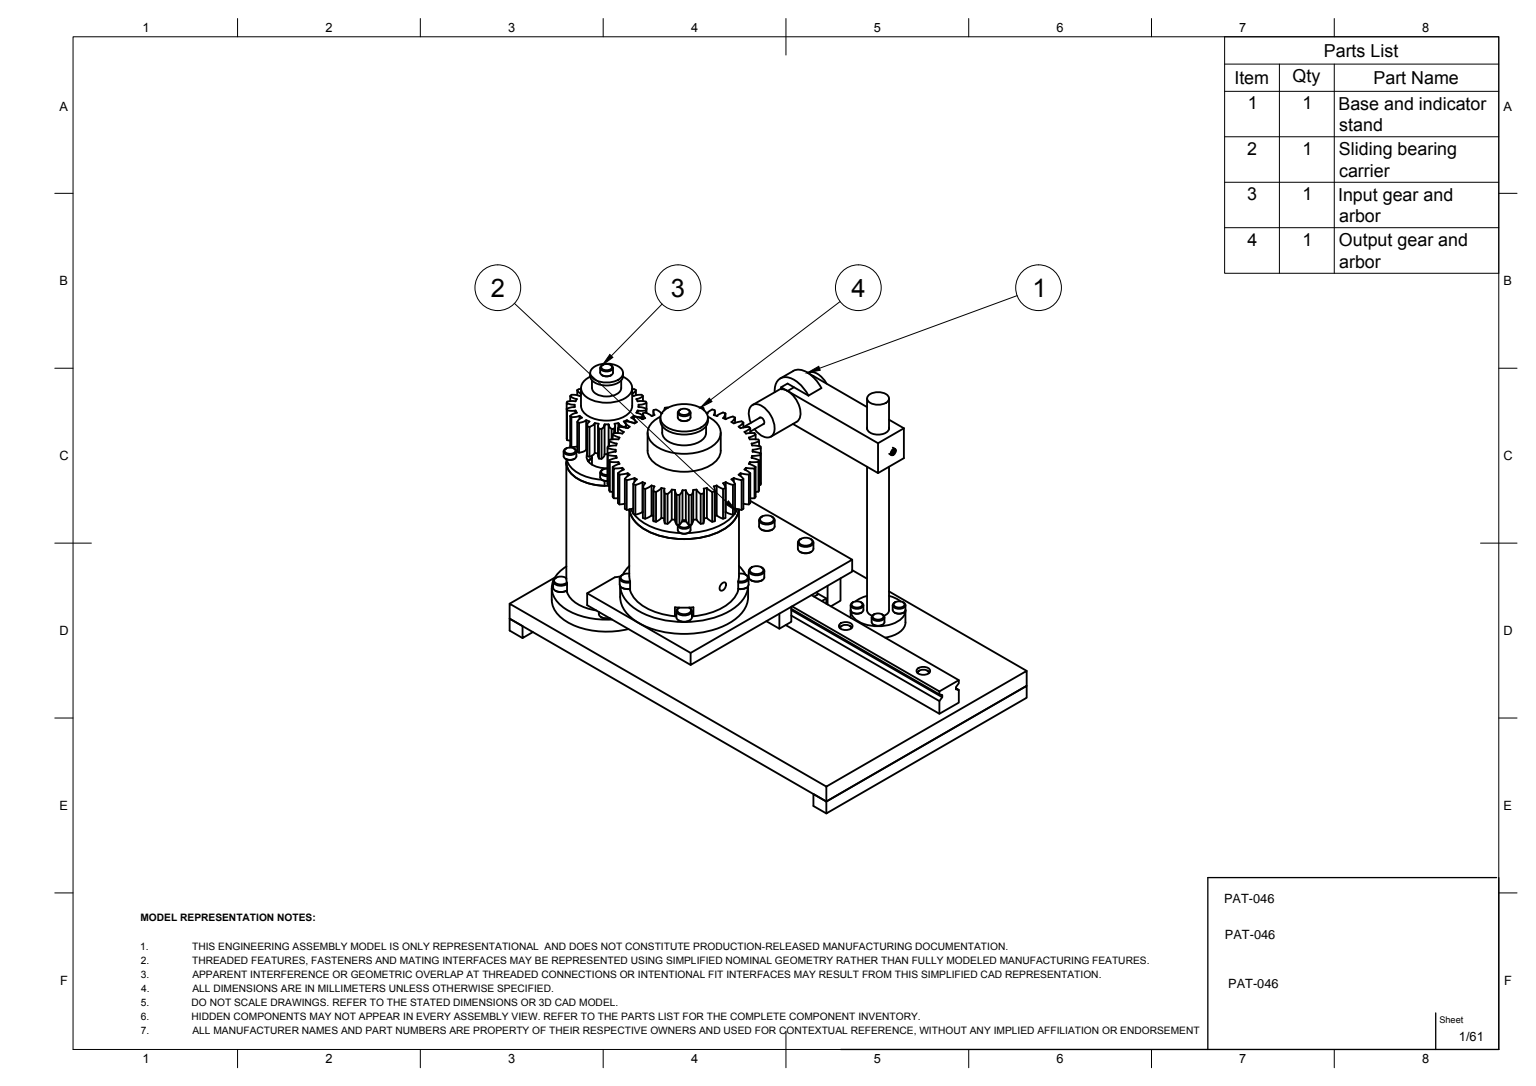
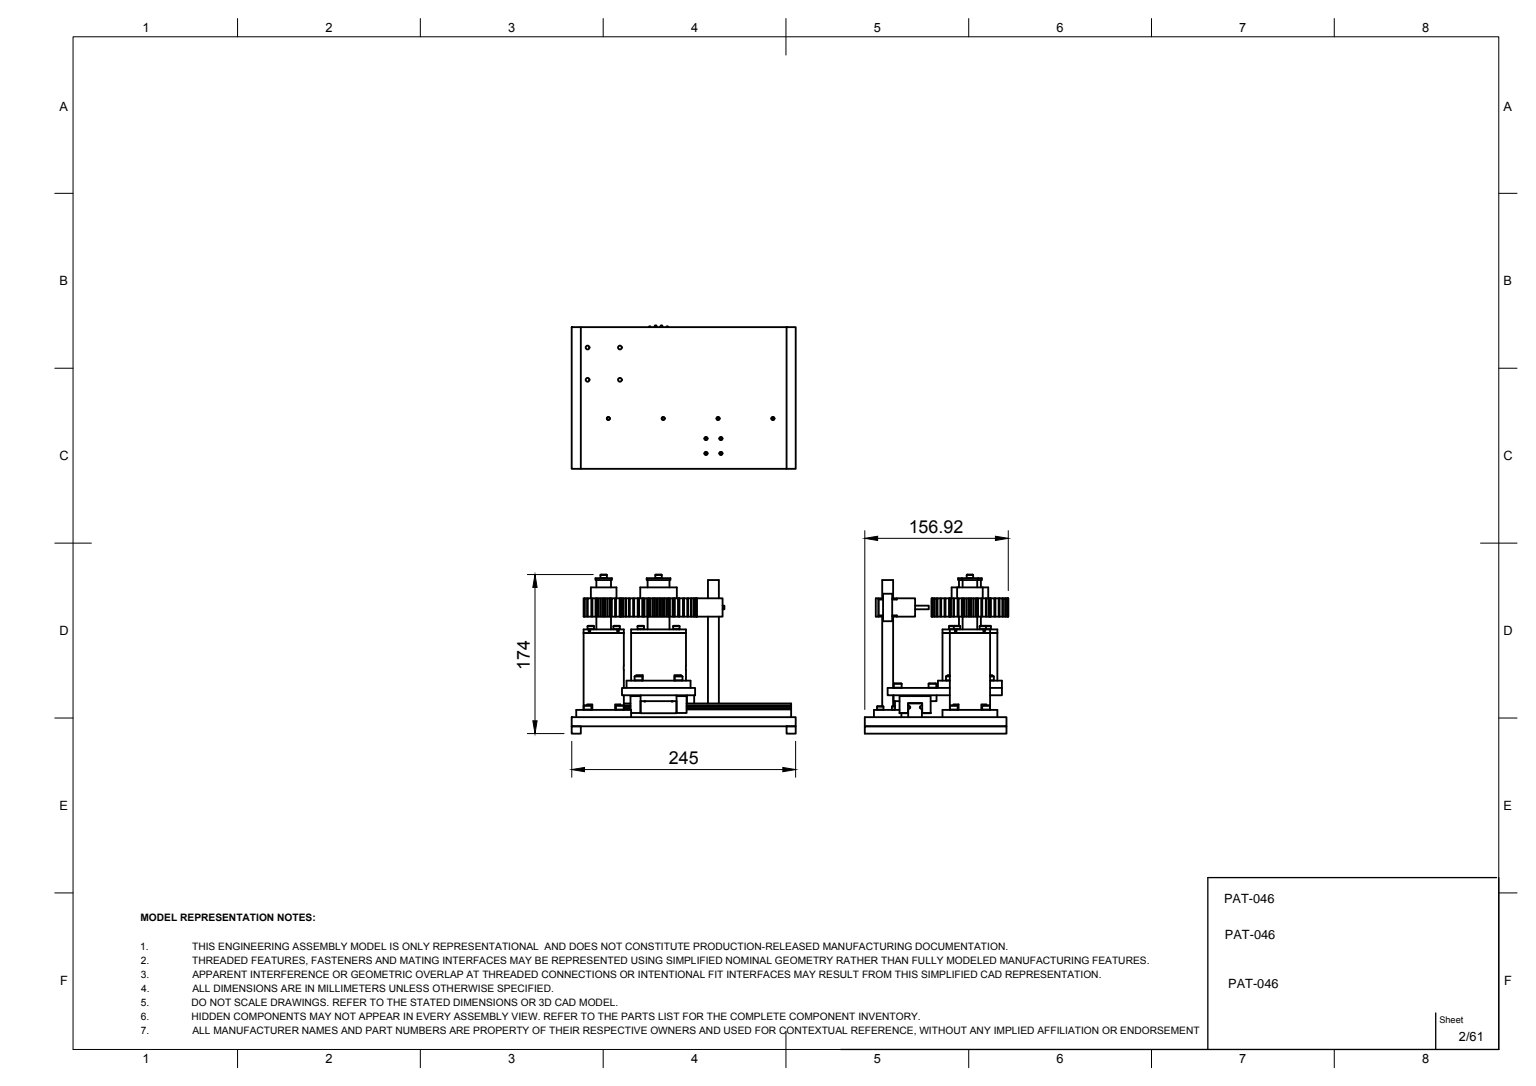
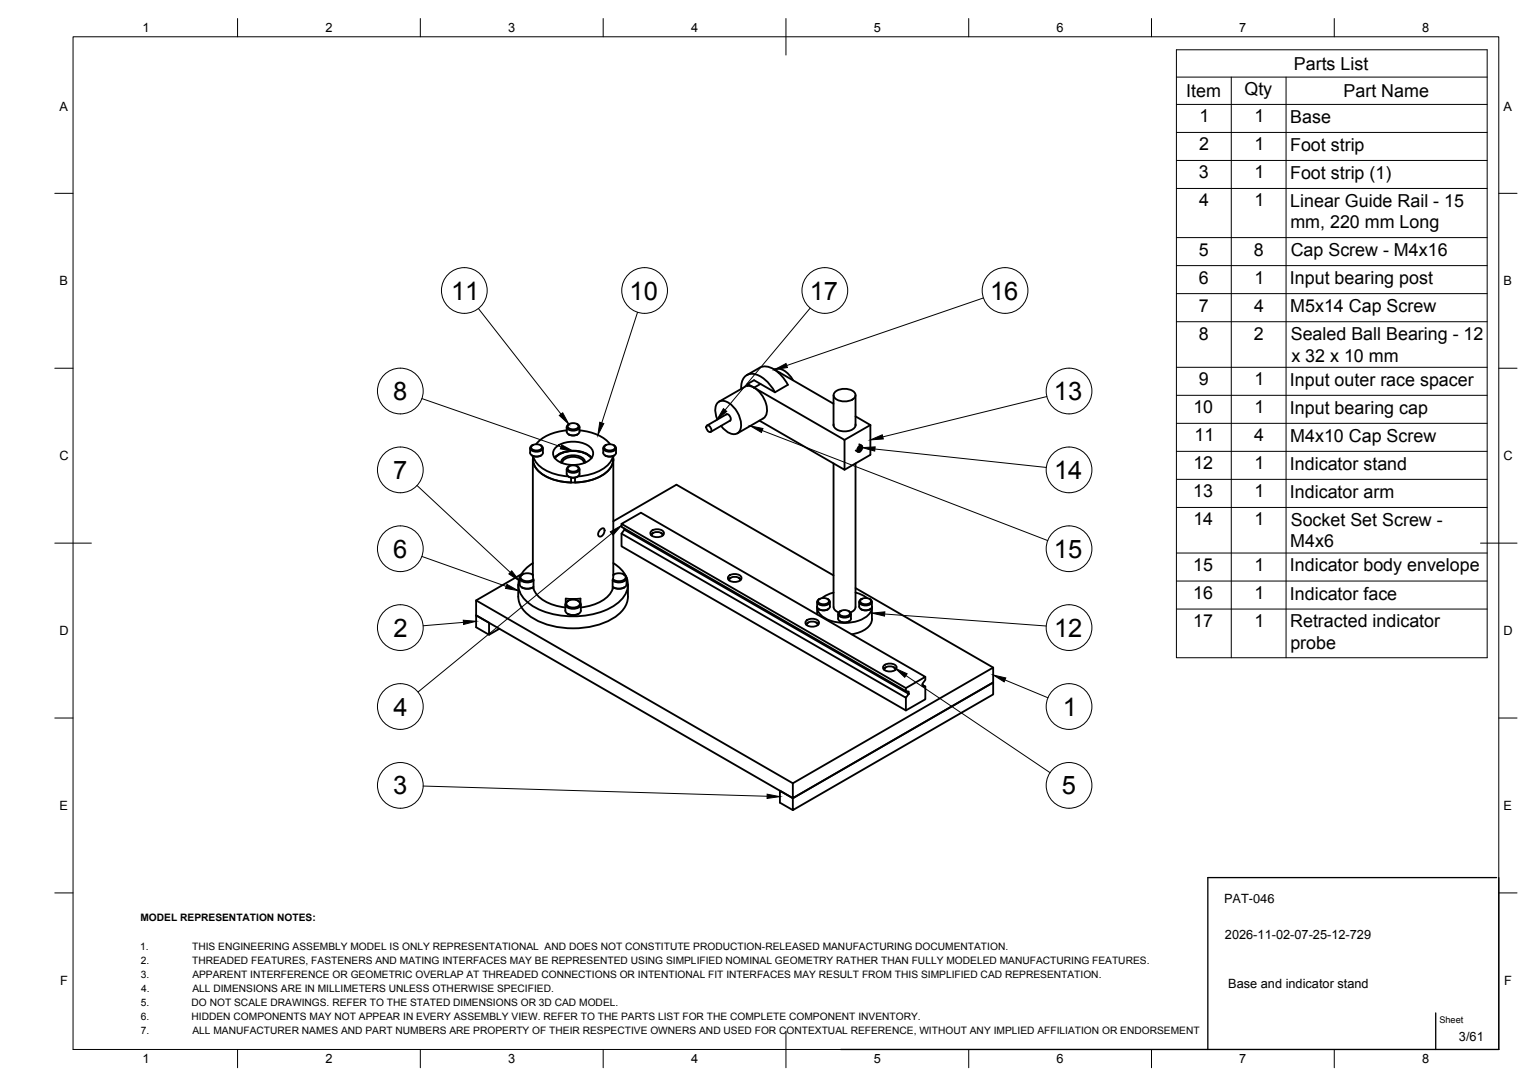
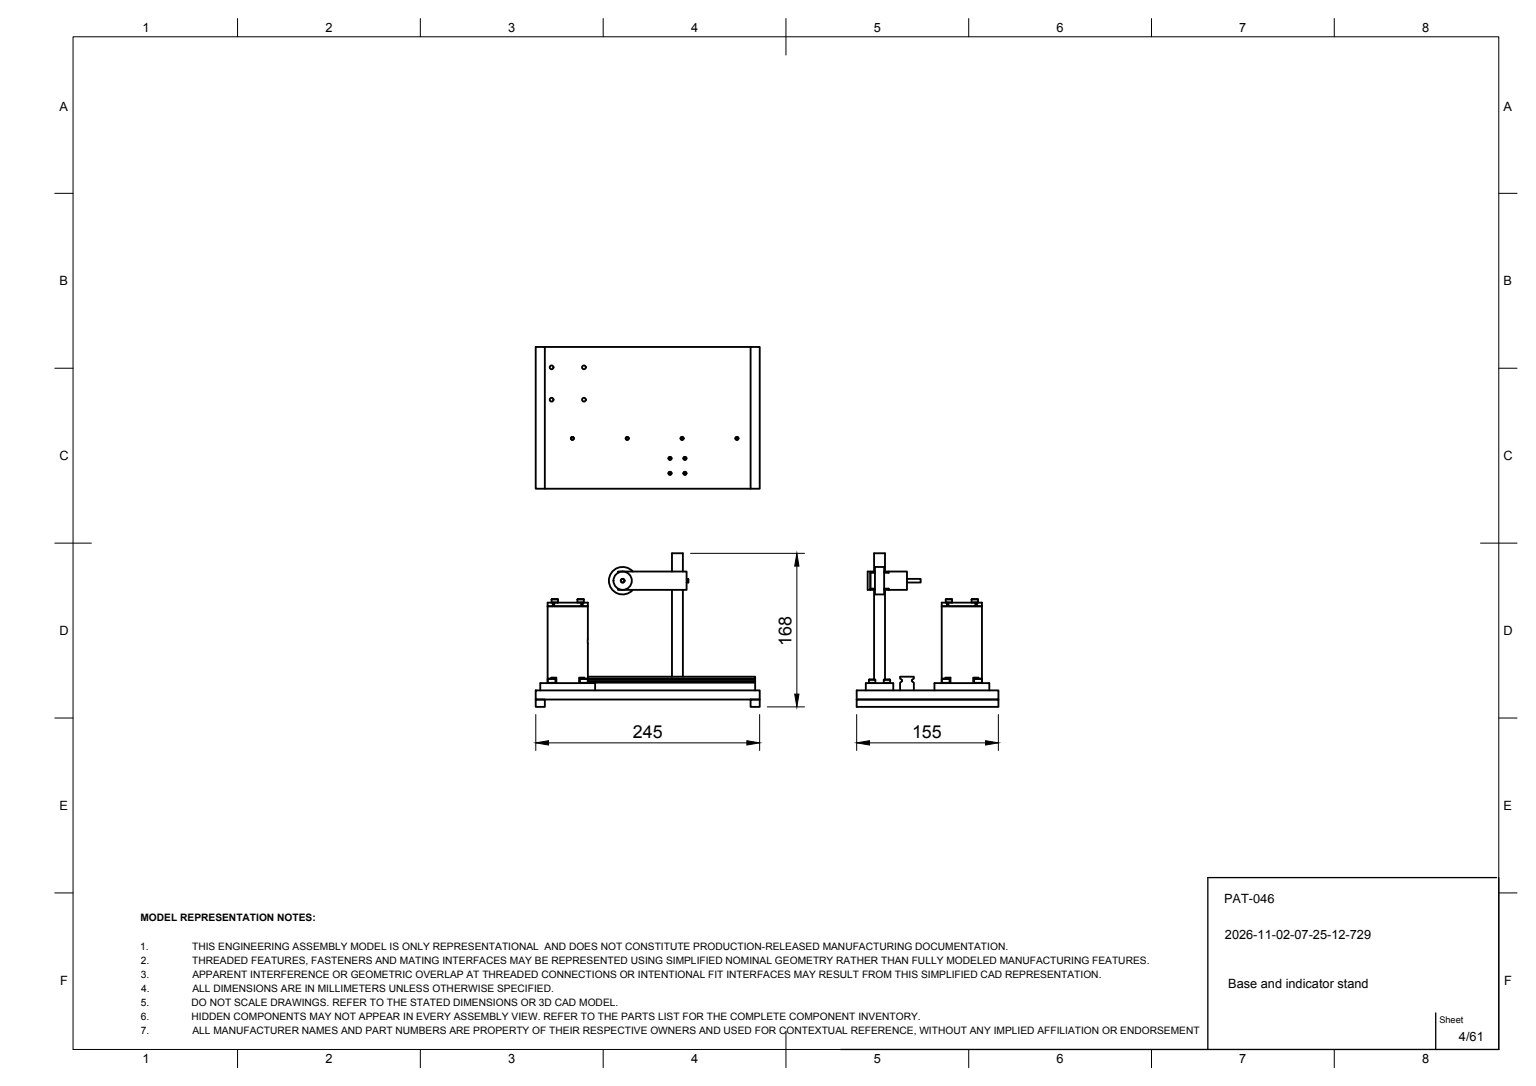
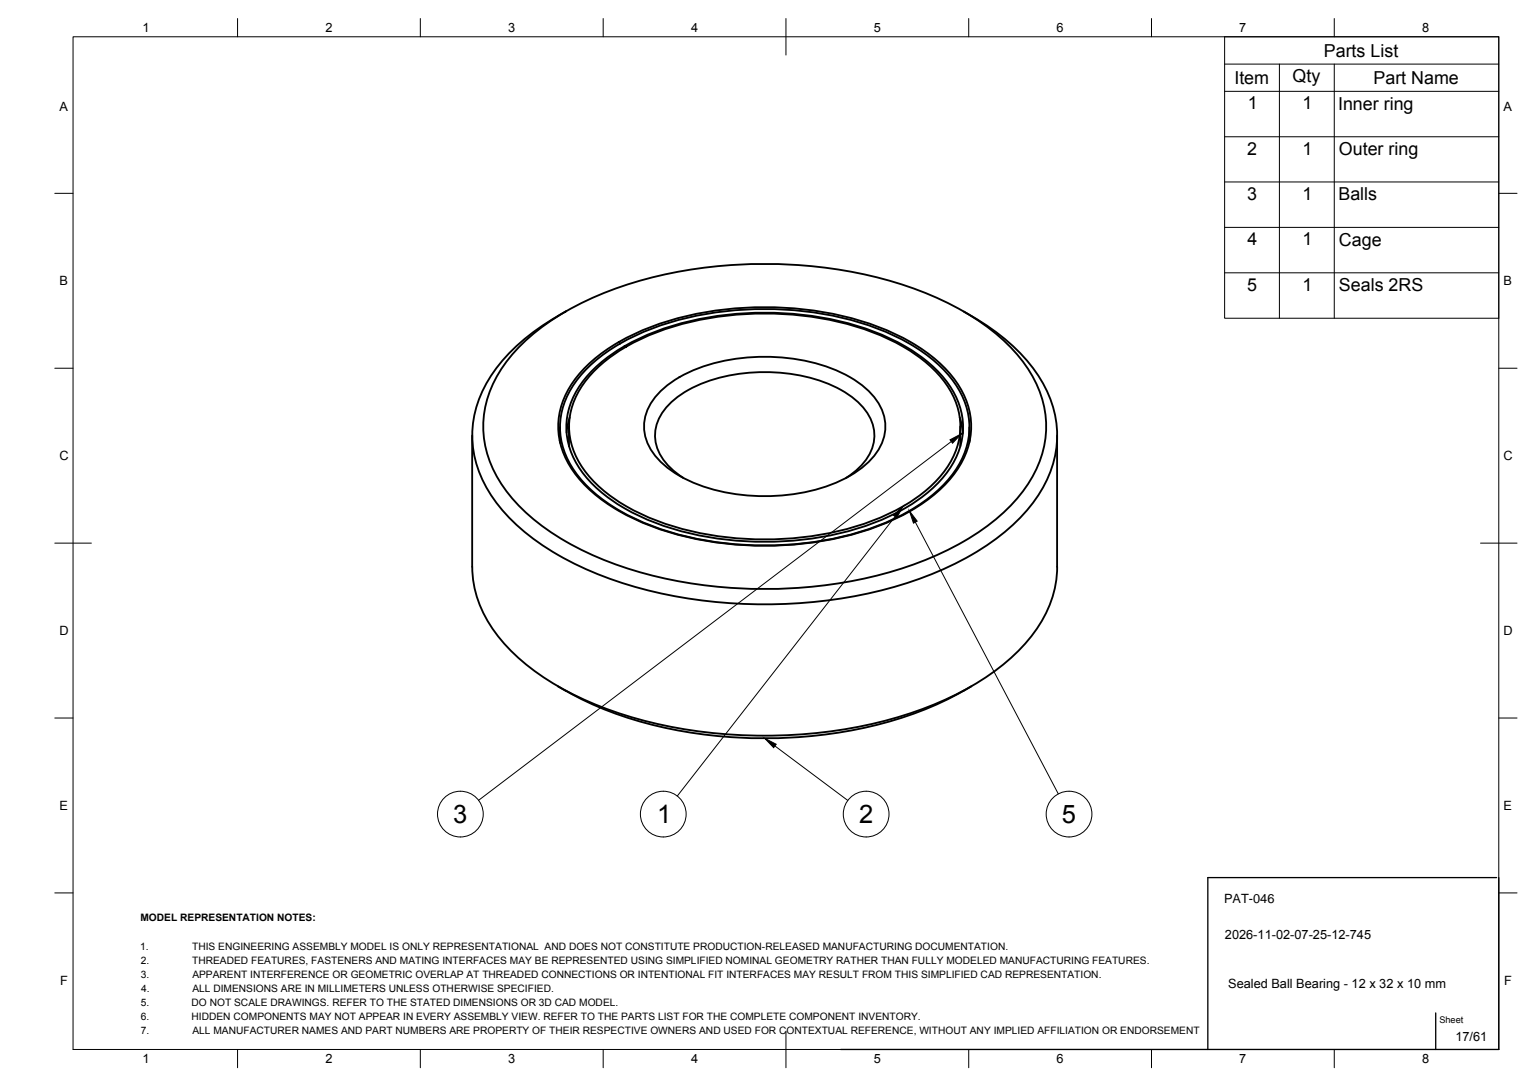
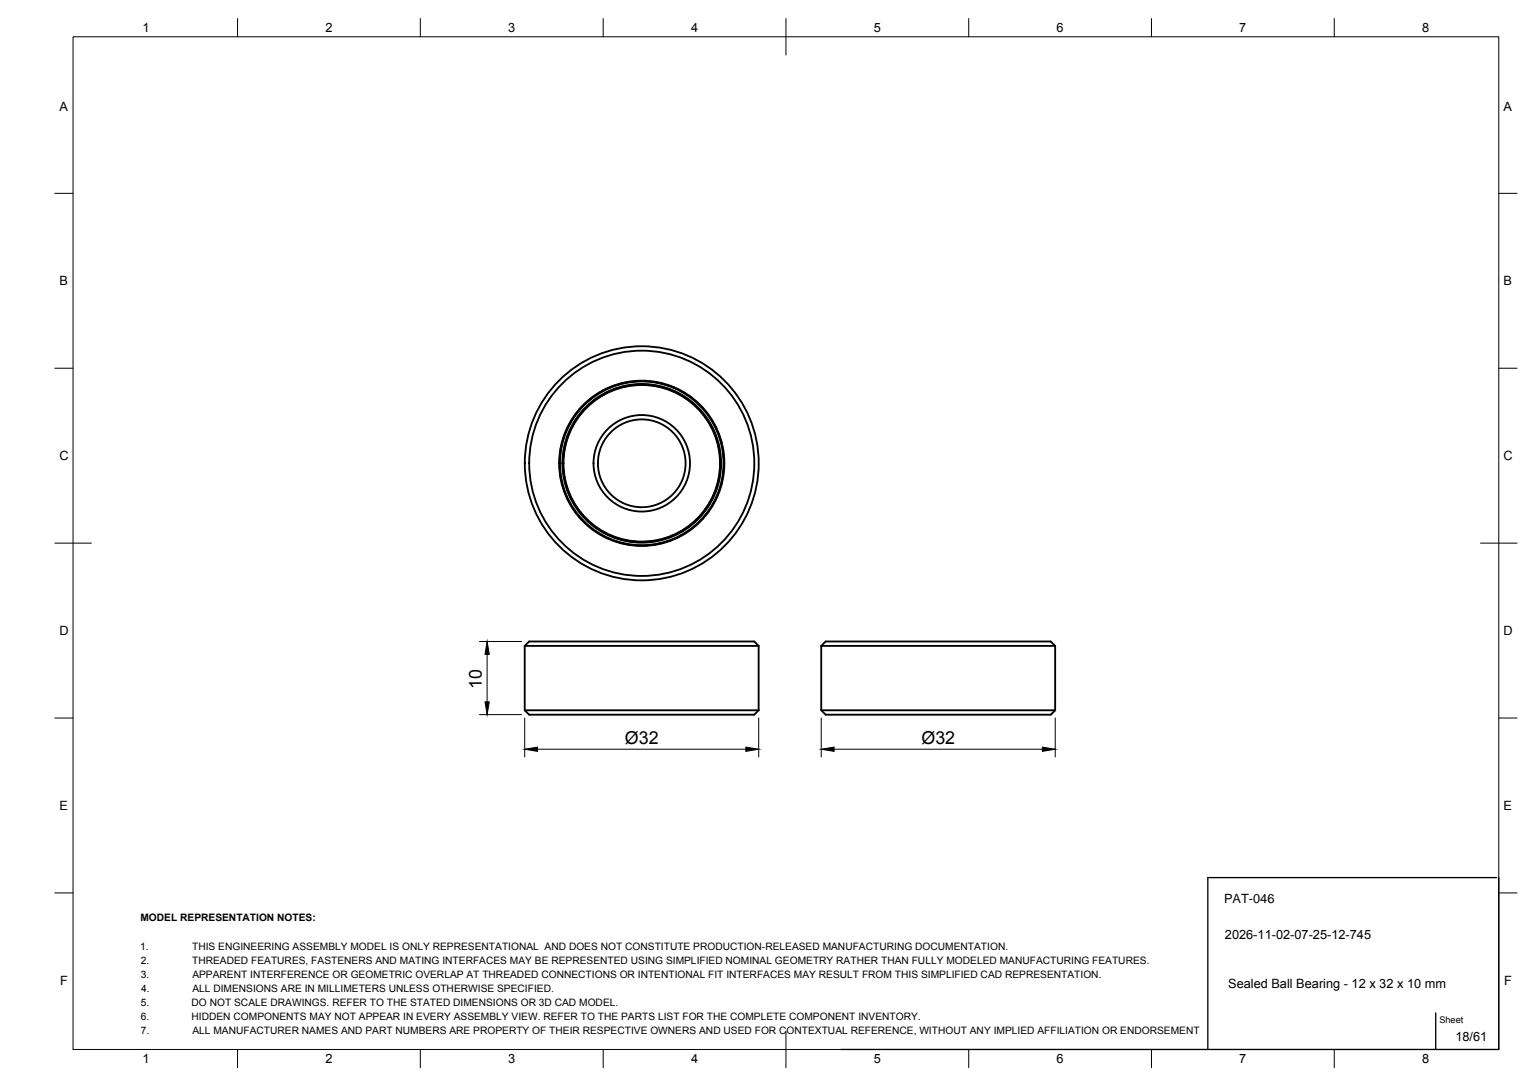
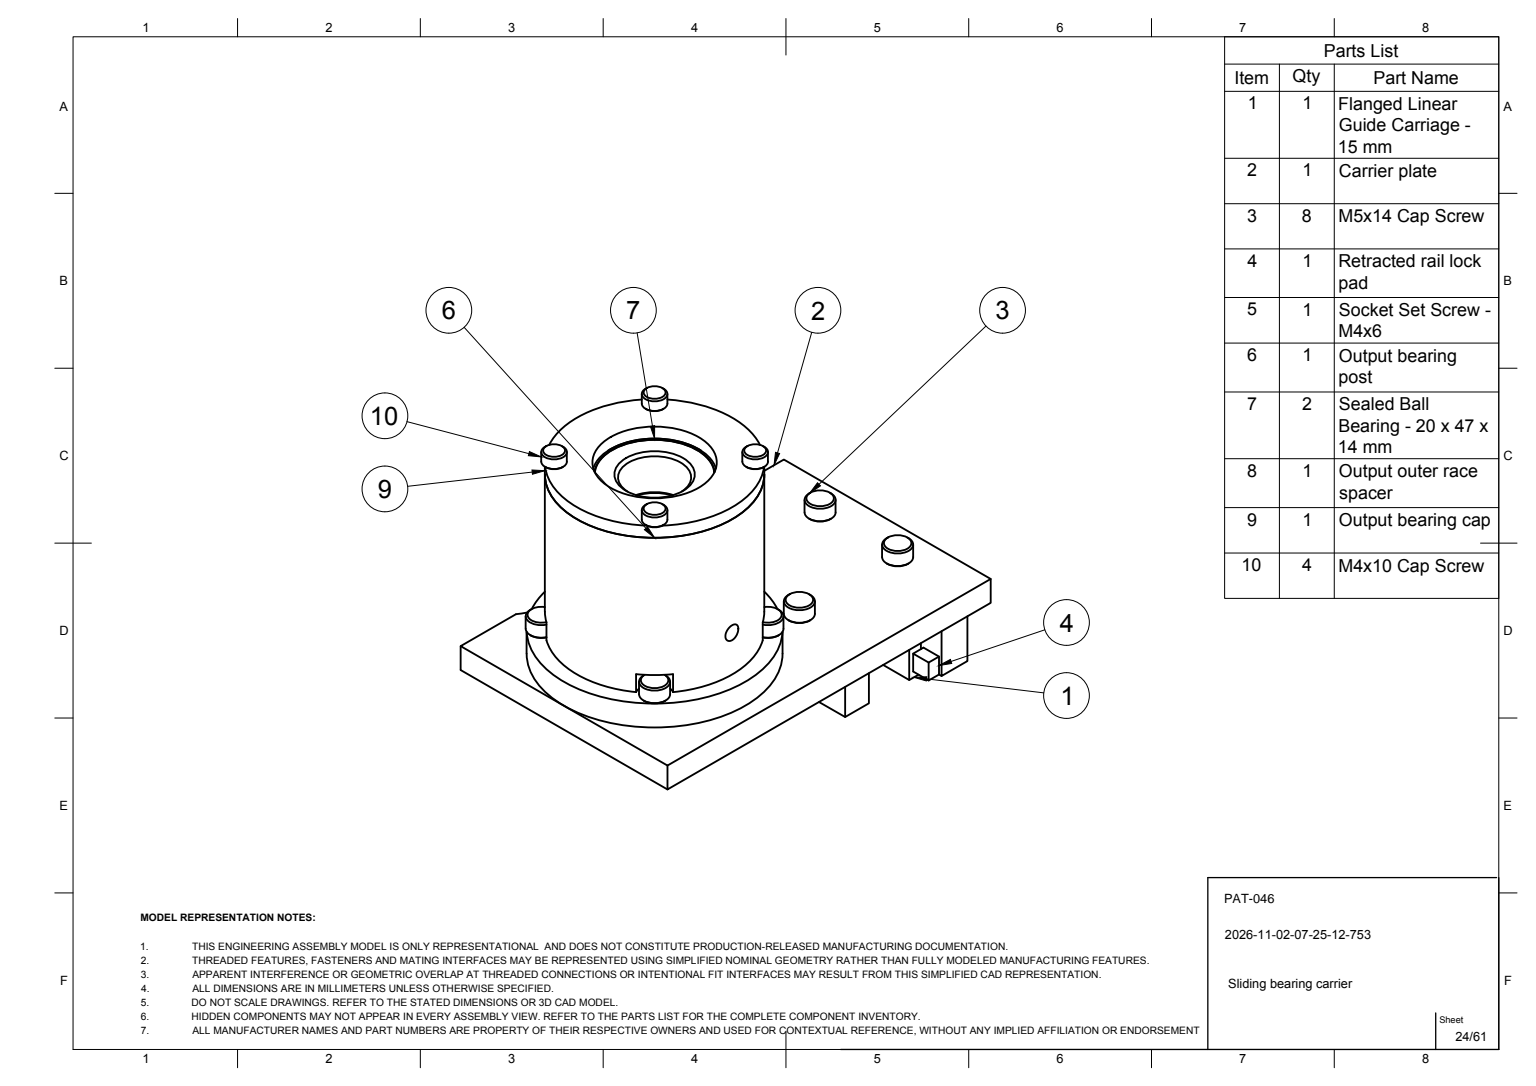
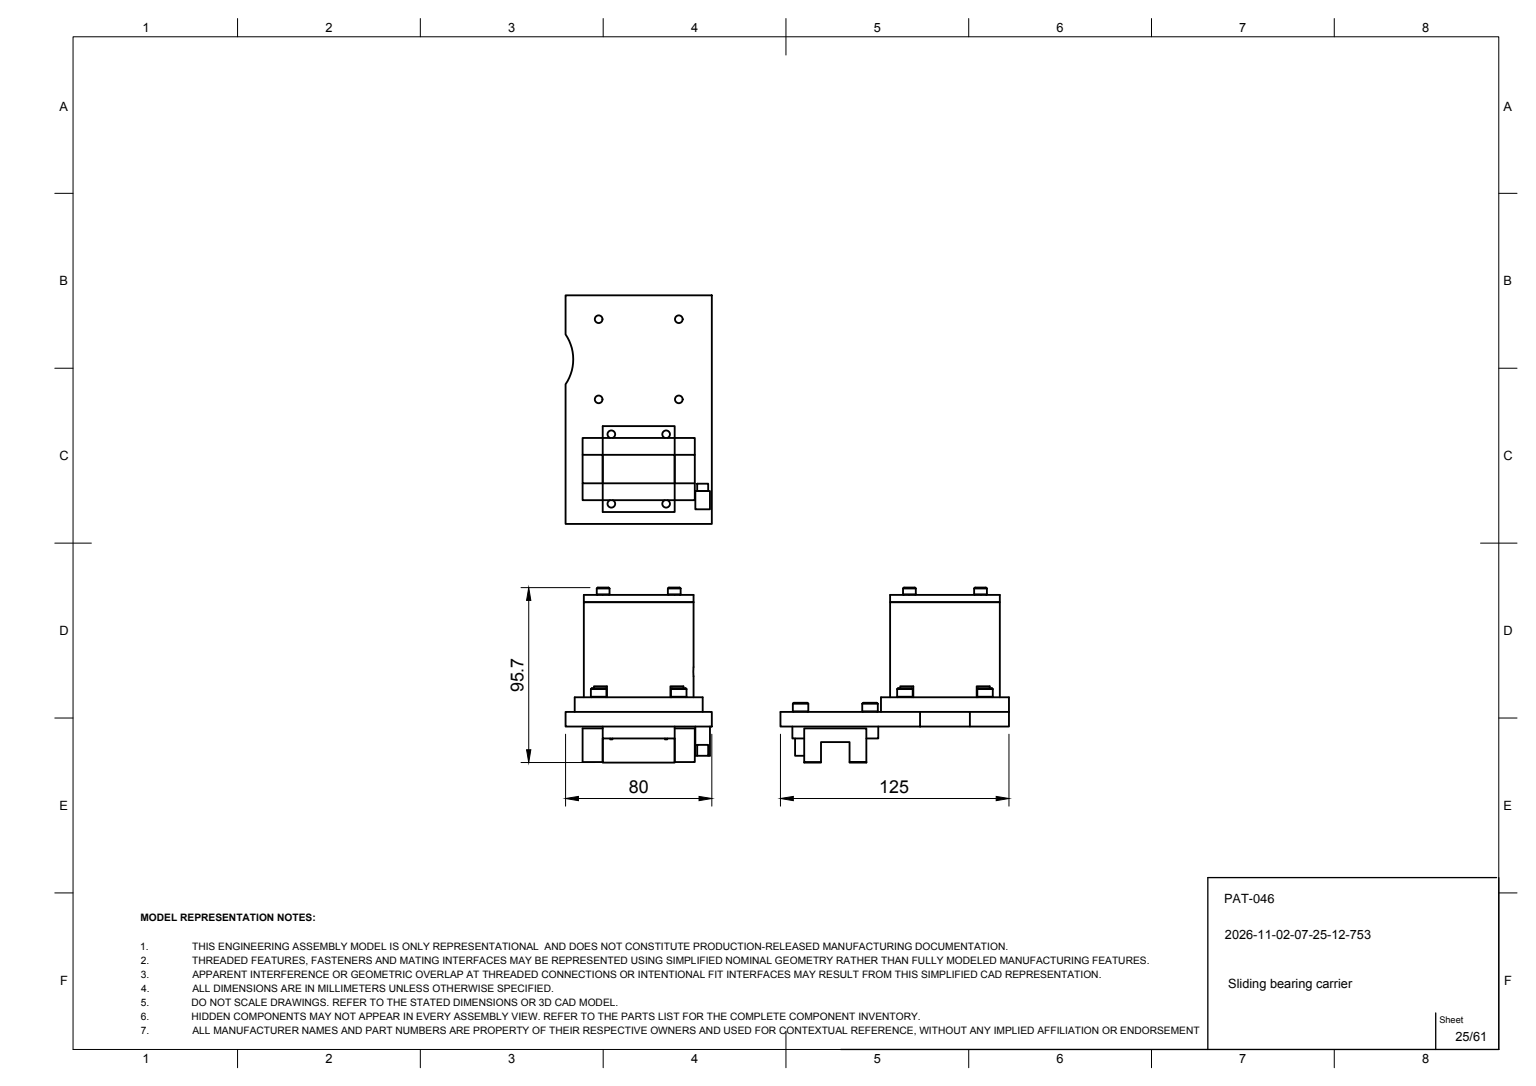
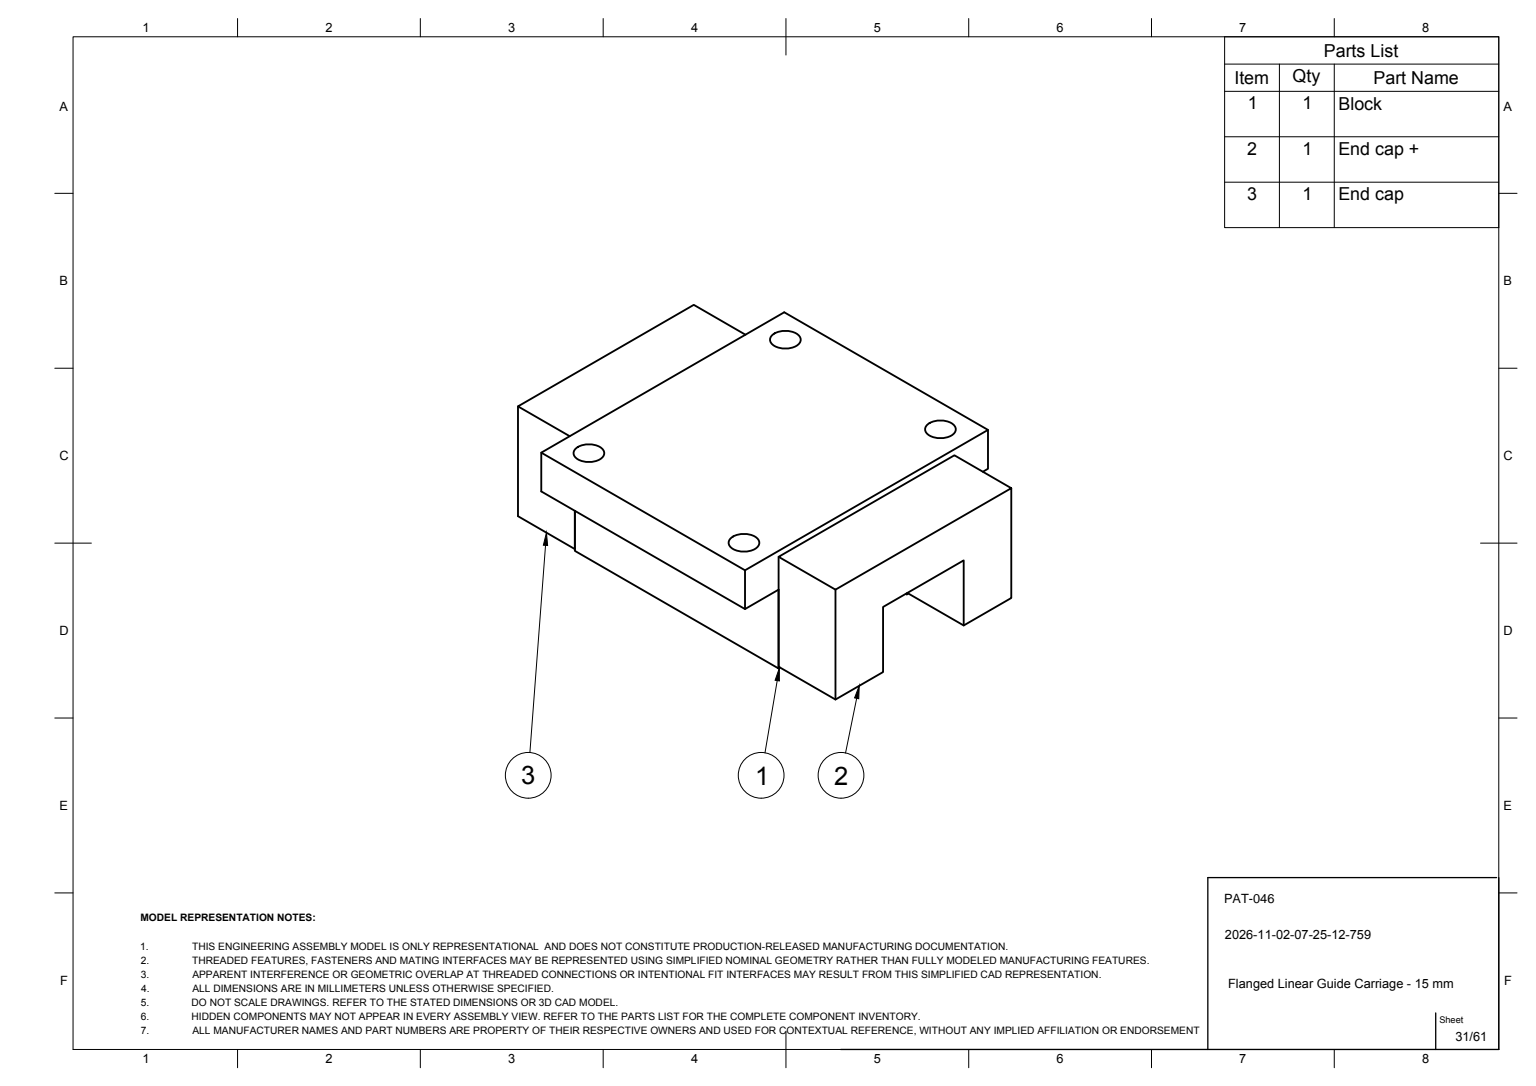
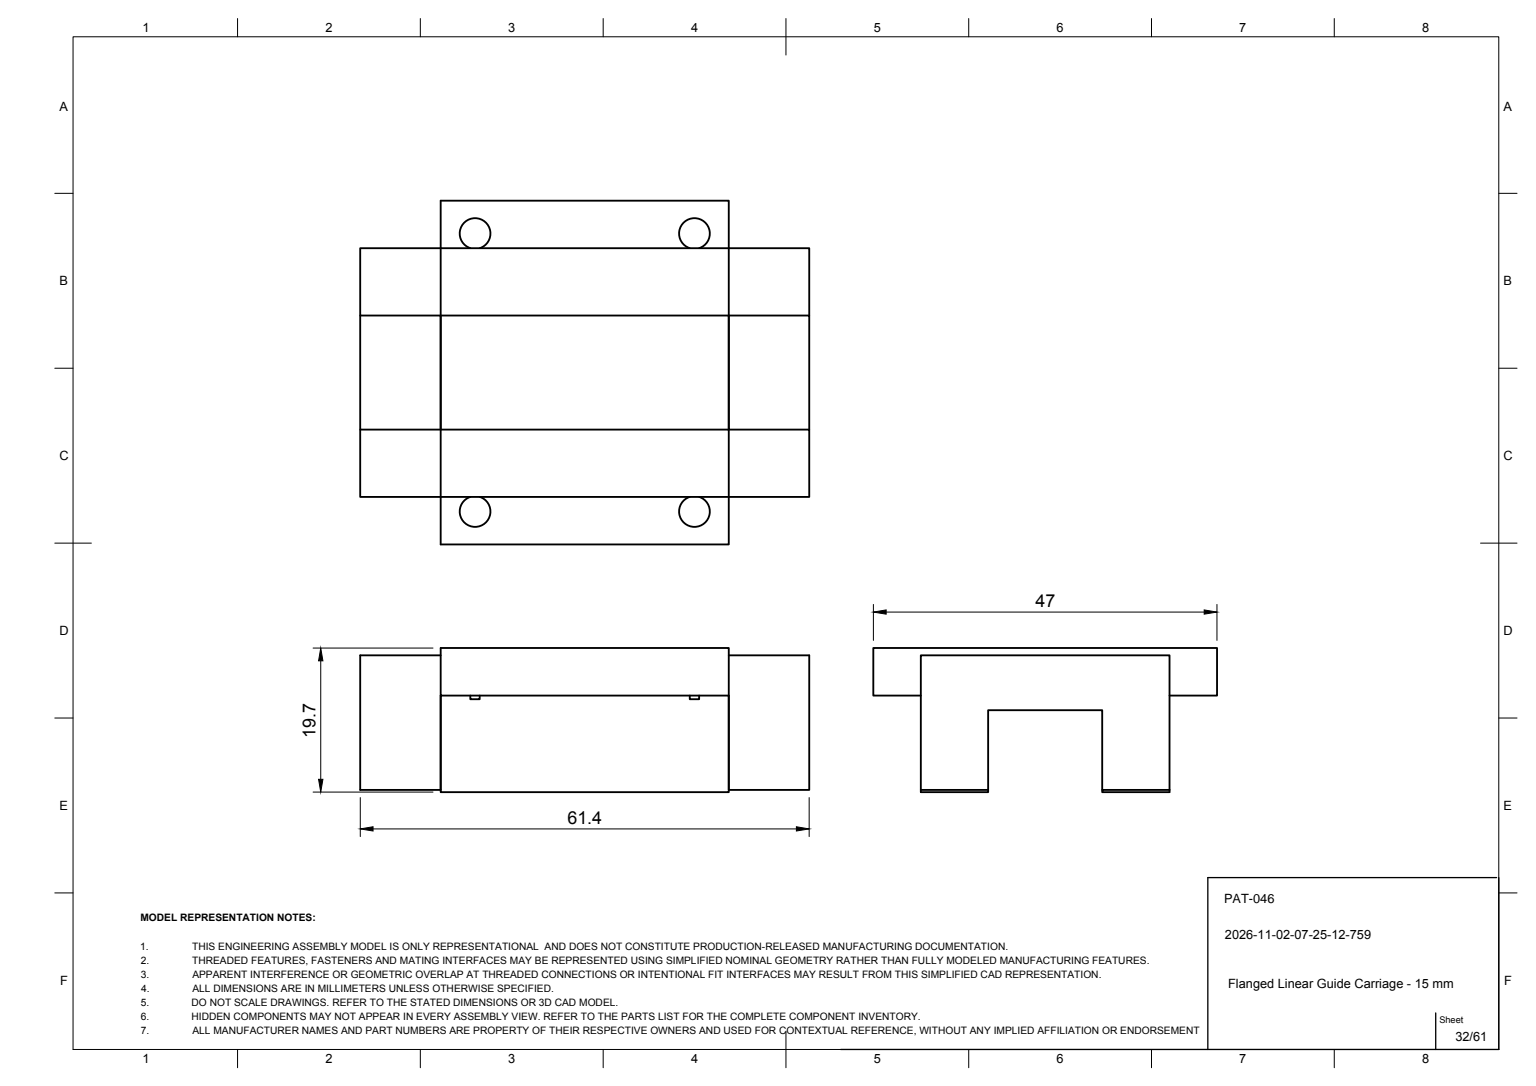
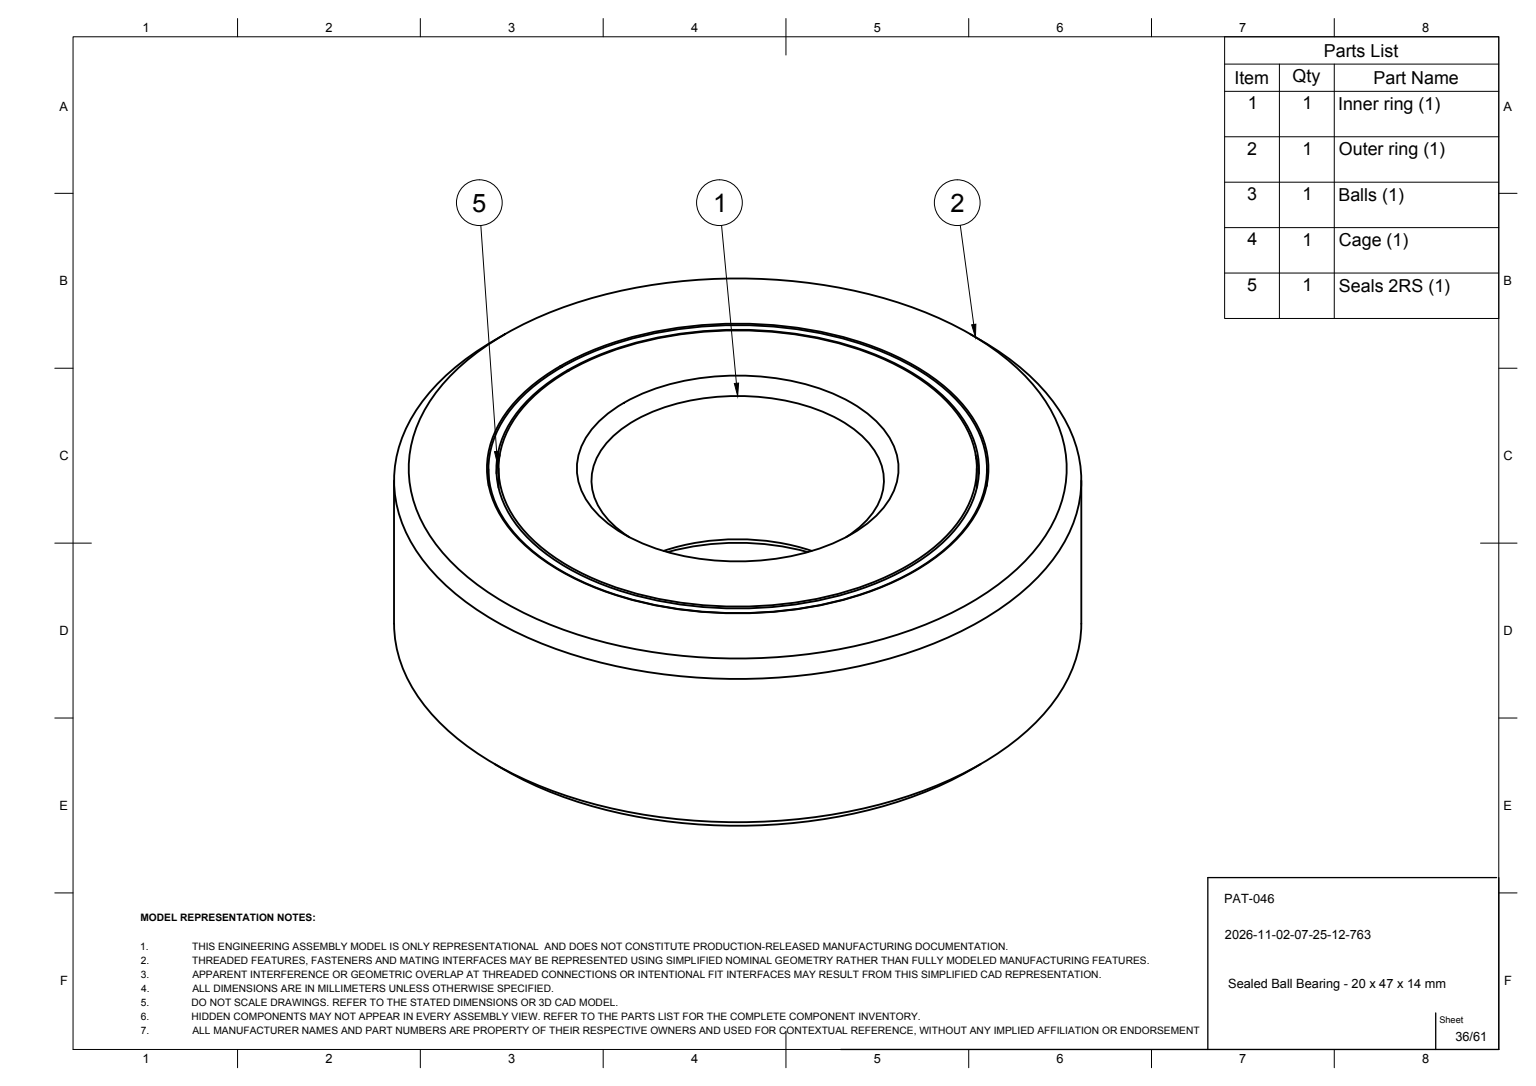
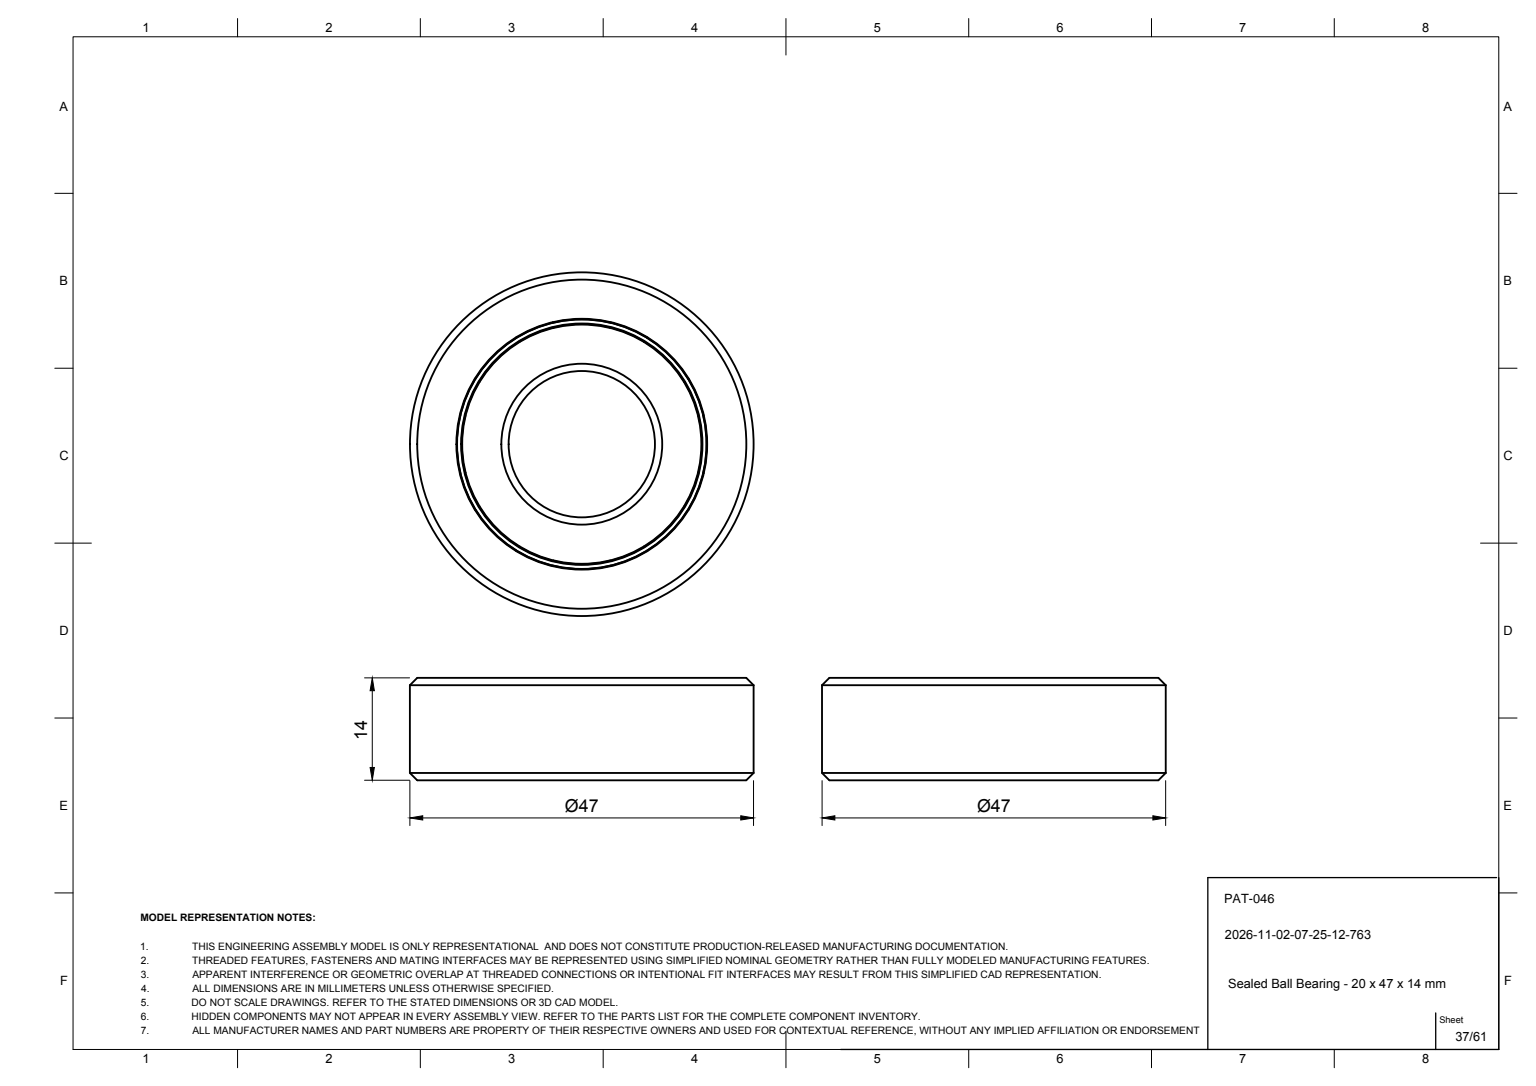
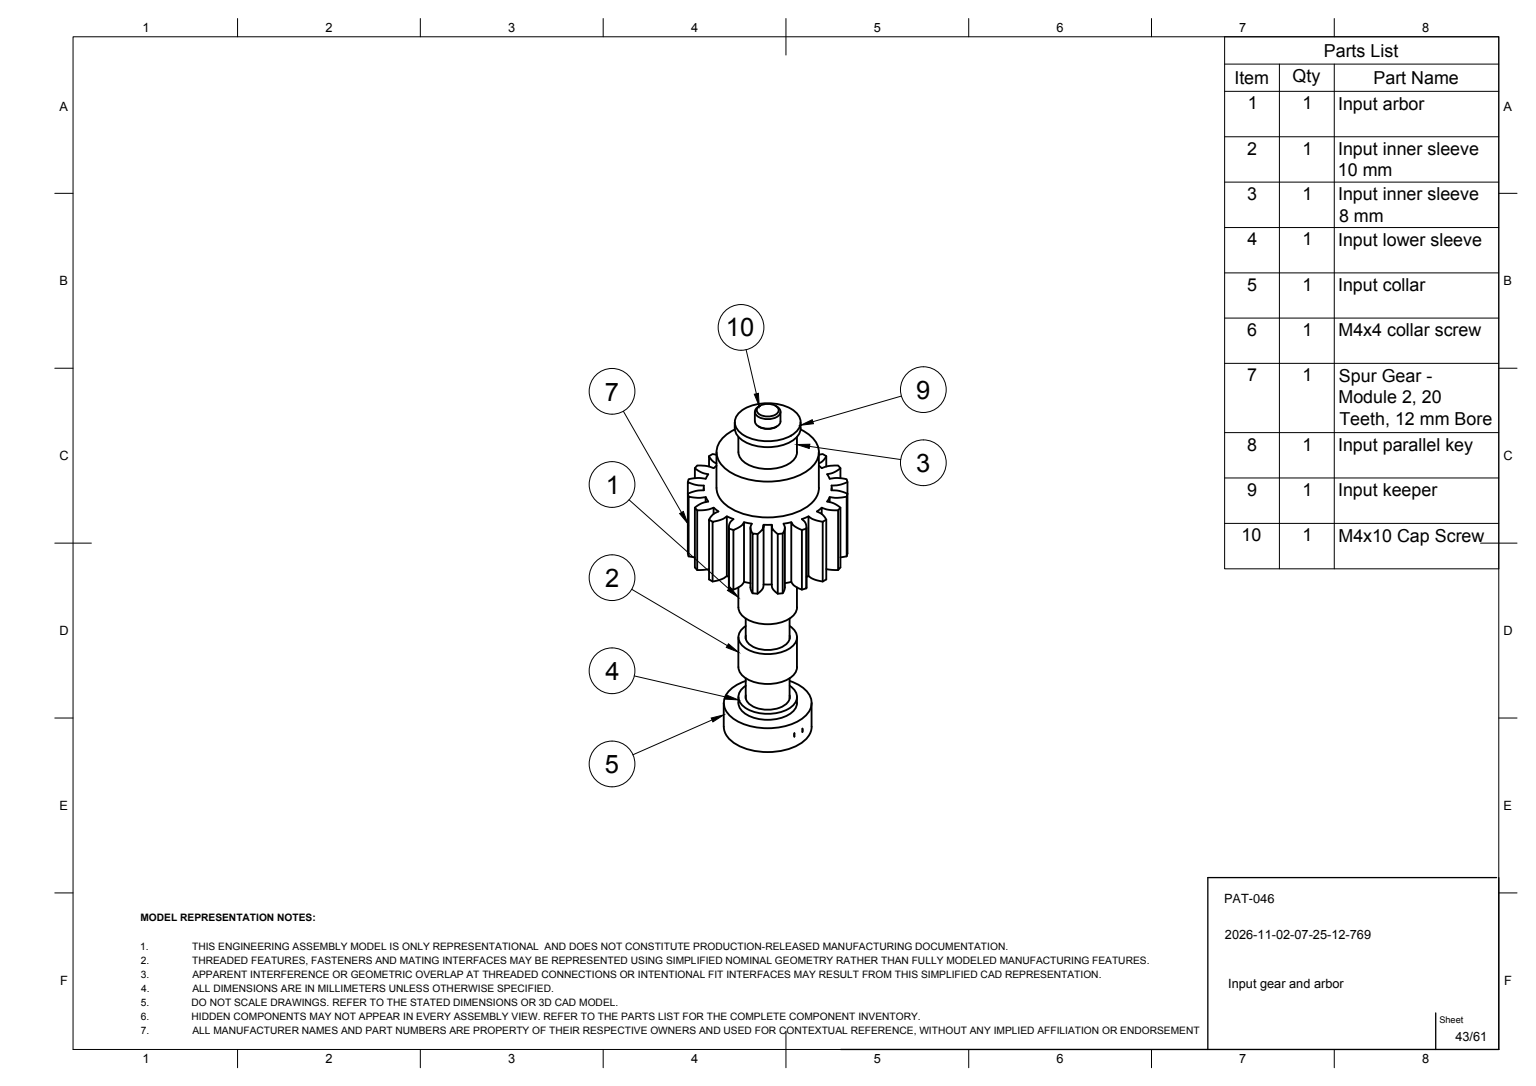
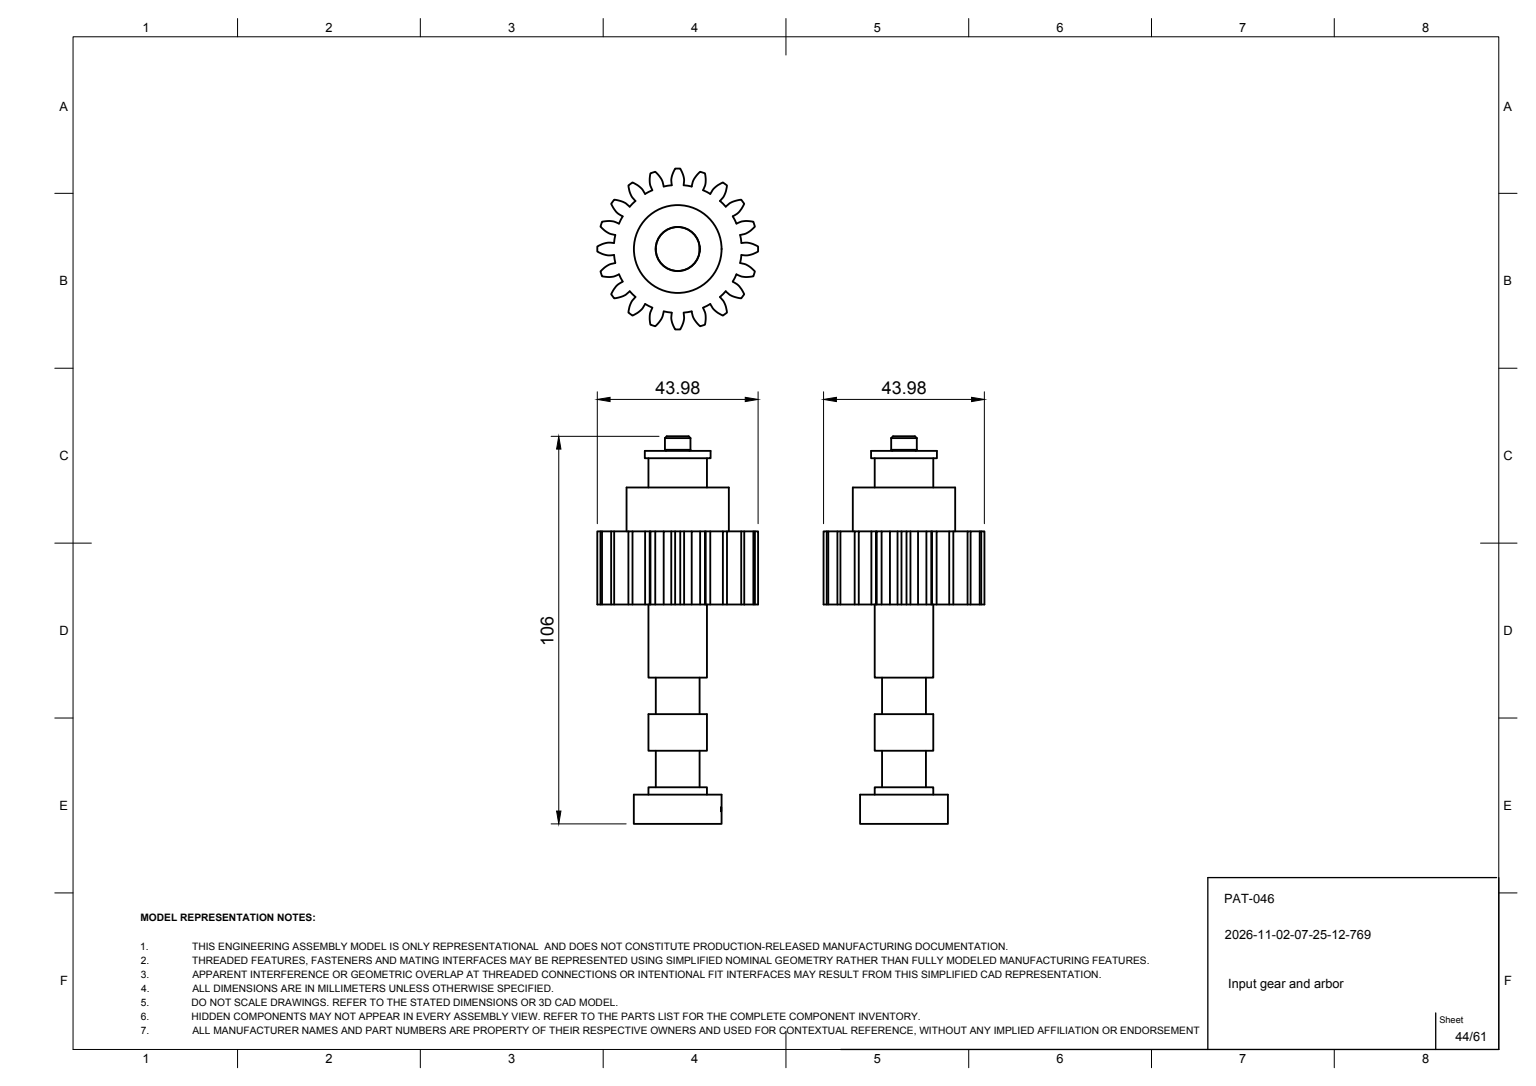
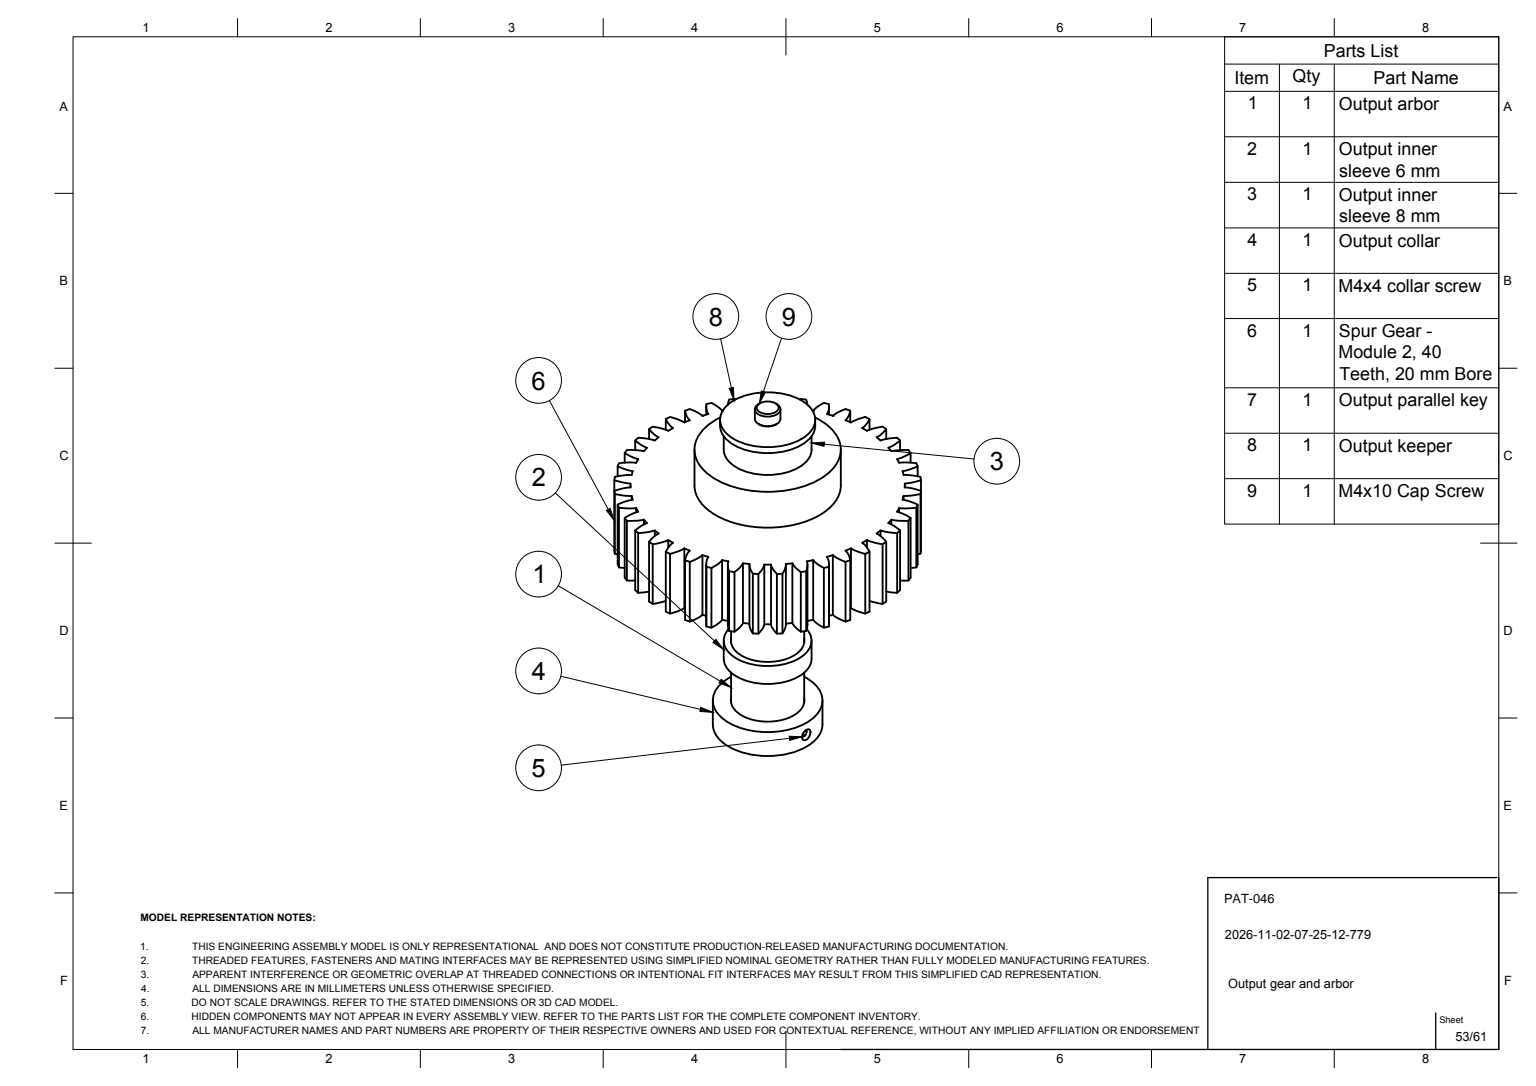
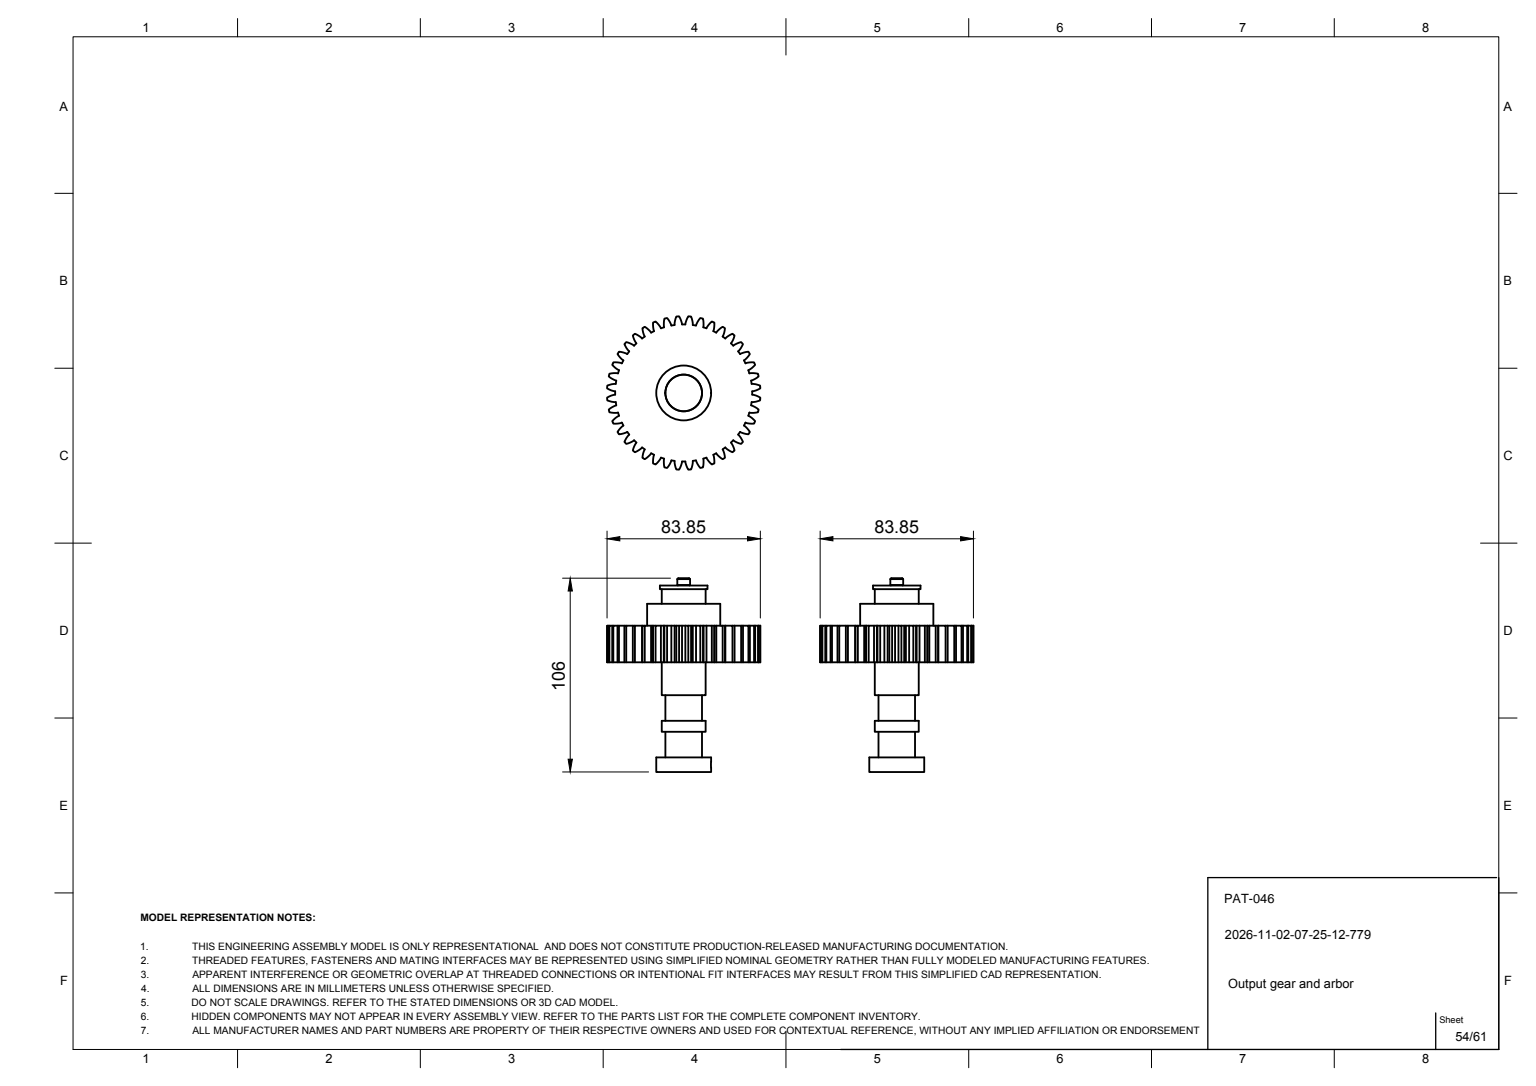
ISO-10303-21;
HEADER;
/* Generated by software containing ST-Developer
 * from STEP Tools, Inc. (www.steptools.com) 
 */

FILE_DESCRIPTION(
/* description */ ('Gear mesh backlash fixture'),
/* implementation_level */ '2;1');

FILE_NAME(
/* name */ 'PAT-046',
/* time_stamp */ '2026-10-28T03:26:00-07:00',
/* author */ (''),
/* organization */ (''),
/* preprocessor_version */ 'ST-DEVELOPER v20.2',
/* originating_system */ 'Autodesk Translation Framework v15.17.0.0',
/* authorisation */ '');

FILE_SCHEMA (('AUTOMOTIVE_DESIGN { 1 0 10303 214 3 1 1 }'));
ENDSEC;

DATA;
#10=MECHANICAL_DESIGN_GEOMETRIC_PRESENTATION_REPRESENTATION('',(#1016,#1017,
#1018,#1019,#1020,#1021,#1022,#1023,#1024,#1025,#1026,#1027,#1028,#1029,
#1030,#1031,#1032,#1033,#1034,#1035,#1036,#1037,#1038,#1039,#1040,#1041,
#1042,#1043,#1044,#1045,#1046,#1047,#1048,#1049,#1050,#1051,#1052,#1053,
#1054,#1055,#1056,#1057,#1058,#1059,#1060,#1061,#1062,#1063,#1064,#1065,
#1066,#1067,#1068,#1069,#1070,#1071,#1072,#1073,#1074,#1075,#1076,#1077,
#1078,#1079,#1080),#57900);
#11=(
BOUNDED_SURFACE()
B_SPLINE_SURFACE(5,1,((#25176,#25177),(#25178,#25179),(#25180,#25181),(#25182,
#25183),(#25184,#25185),(#25186,#25187),(#25188,#25189),(#25190,#25191),
(#25192,#25193),(#25194,#25195),(#25196,#25197),(#25198,#25199),(#25200,
#25201),(#25202,#25203),(#25204,#25205),(#25206,#25207),(#25208,#25209),
(#25210,#25211),(#25212,#25213),(#25214,#25215),(#25216,#25217),(#25218,
#25219),(#25220,#25221),(#25222,#25223),(#25224,#25225),(#25226,#25227),
(#25228,#25229),(#25230,#25231),(#25232,#25233),(#25234,#25235),(#25236,
#25237),(#25238,#25239),(#25240,#25241),(#25242,#25243),(#25244,#25245),
(#25246,#25247),(#25248,#25249),(#25250,#25251),(#25252,#25253),(#25254,
#25255),(#25256,#25257),(#25258,#25259),(#25260,#25261),(#25262,#25263),
(#25264,#25265),(#25266,#25267),(#25268,#25269),(#25270,#25271),(#25272,
#25273),(#25274,#25275),(#25276,#25277),(#25278,#25279),(#25280,#25281),
(#25282,#25283),(#25284,#25285),(#25286,#25287),(#25288,#25289),(#25290,
#25291),(#25292,#25293),(#25294,#25295),(#25296,#25297),(#25298,#25299),
(#25300,#25301),(#25302,#25303),(#25304,#25305),(#25306,#25307),(#25308,
#25309),(#25310,#25311),(#25312,#25313),(#25314,#25315)),.UNSPECIFIED.,
 .F.,.F.,.F.)
B_SPLINE_SURFACE_WITH_KNOTS((6,1,1,1,1,1,1,1,1,1,1,1,1,1,1,1,1,1,1,1,1,
1,1,1,1,1,1,1,1,1,1,1,1,1,1,1,1,1,1,1,1,1,1,1,1,1,1,1,1,1,1,1,1,1,1,1,1,
1,1,1,1,1,1,1,1,6),(2,2),(-1.,-0.984615384615383,-0.969230769230768,-0.953846153846152,
-0.938461538461537,-0.923076923076922,-0.907692307692306,-0.892307692307691,
-0.876923076923076,-0.86153846153846,-0.846153846153845,-0.83076923076923,
-0.815384615384614,-0.799999999999999,-0.784615384615384,-0.769230769230768,
-0.753846153846153,-0.738461538461538,-0.723076923076922,-0.707692307692307,
-0.692307692307692,-0.676923076923076,-0.661538461538461,-0.646153846153846,
-0.63076923076923,-0.615384615384615,-0.6,-0.584615384615384,-0.569230769230769,
-0.553846153846154,-0.538461538461538,-0.523076923076923,-0.507692307692308,
-0.492307692307692,-0.476923076923077,-0.461538461538462,-0.446153846153846,
-0.430769230769231,-0.415384615384615,-0.4,-0.384615384615385,-0.369230769230769,
-0.353846153846154,-0.338461538461538,-0.323076923076923,-0.307692307692308,
-0.292307692307692,-0.276923076923077,-0.261538461538462,-0.246153846153846,
-0.230769230769231,-0.215384615384615,-0.2,-0.184615384615385,-0.169230769230769,
-0.153846153846154,-0.138461538461538,-0.123076923076923,-0.107692307692308,
-0.0923076923076923,-0.0769230769230769,-0.0615384615384615,-0.0461538461538462,
-0.0307692307692308,-0.0153846153846154,0.),(-1.,1.),.UNSPECIFIED.)
GEOMETRIC_REPRESENTATION_ITEM()
RATIONAL_B_SPLINE_SURFACE(((1.,1.),(1.,1.),(1.,1.),(1.,1.),(1.,1.),(1.,
1.),(1.,1.),(1.,1.),(1.,1.),(1.,1.),(1.,1.),(1.,1.),(1.,1.),(1.,1.),(1.,
1.),(1.,1.),(1.,1.),(1.,1.),(1.,1.),(1.,1.),(1.,1.),(1.,1.),(1.,1.),(1.,
1.),(1.,1.),(1.,1.),(1.,1.),(1.,1.),(1.,1.),(1.,1.),(1.,1.),(1.,1.),(1.,
1.),(1.,1.),(1.,1.),(1.,1.),(1.,1.),(1.,1.),(1.,1.),(1.,1.),(1.,1.),(1.,
1.),(1.,1.),(1.,1.),(1.,1.),(1.,1.),(1.,1.),(1.,1.),(1.,1.),(1.,1.),(1.,
1.),(1.,1.),(1.,1.),(1.,1.),(1.,1.),(1.,1.),(1.,1.),(1.,1.),(1.,1.),(1.,
1.),(1.,1.),(1.,1.),(1.,1.),(1.,1.),(1.,1.),(1.,1.),(1.,1.),(1.,1.),(1.,
1.),(1.,1.)))
REPRESENTATION_ITEM('')
SURFACE()
);
#12=(
BOUNDED_SURFACE()
B_SPLINE_SURFACE(5,1,((#25394,#25395),(#25396,#25397),(#25398,#25399),(#25400,
#25401),(#25402,#25403),(#25404,#25405),(#25406,#25407),(#25408,#25409),
(#25410,#25411),(#25412,#25413),(#25414,#25415),(#25416,#25417),(#25418,
#25419),(#25420,#25421),(#25422,#25423),(#25424,#25425),(#25426,#25427),
(#25428,#25429),(#25430,#25431),(#25432,#25433),(#25434,#25435),(#25436,
#25437),(#25438,#25439),(#25440,#25441),(#25442,#25443),(#25444,#25445),
(#25446,#25447),(#25448,#25449),(#25450,#25451),(#25452,#25453),(#25454,
#25455),(#25456,#25457),(#25458,#25459),(#25460,#25461),(#25462,#25463),
(#25464,#25465),(#25466,#25467),(#25468,#25469),(#25470,#25471),(#25472,
#25473),(#25474,#25475),(#25476,#25477),(#25478,#25479),(#25480,#25481),
(#25482,#25483),(#25484,#25485),(#25486,#25487),(#25488,#25489),(#25490,
#25491),(#25492,#25493),(#25494,#25495),(#25496,#25497),(#25498,#25499),
(#25500,#25501),(#25502,#25503),(#25504,#25505),(#25506,#25507),(#25508,
#25509),(#25510,#25511),(#25512,#25513),(#25514,#25515),(#25516,#25517),
(#25518,#25519),(#25520,#25521),(#25522,#25523),(#25524,#25525),(#25526,
#25527),(#25528,#25529),(#25530,#25531),(#25532,#25533)),.UNSPECIFIED.,
 .F.,.F.,.F.)
B_SPLINE_SURFACE_WITH_KNOTS((6,1,1,1,1,1,1,1,1,1,1,1,1,1,1,1,1,1,1,1,1,
1,1,1,1,1,1,1,1,1,1,1,1,1,1,1,1,1,1,1,1,1,1,1,1,1,1,1,1,1,1,1,1,1,1,1,1,
1,1,1,1,1,1,1,1,6),(2,2),(-1.,-0.984615384615383,-0.969230769230768,-0.953846153846152,
-0.938461538461537,-0.923076923076922,-0.907692307692306,-0.892307692307691,
-0.876923076923076,-0.86153846153846,-0.846153846153845,-0.83076923076923,
-0.815384615384614,-0.799999999999999,-0.784615384615384,-0.769230769230768,
-0.753846153846153,-0.738461538461538,-0.723076923076922,-0.707692307692307,
-0.692307692307692,-0.676923076923076,-0.661538461538461,-0.646153846153846,
-0.63076923076923,-0.615384615384615,-0.6,-0.584615384615384,-0.569230769230769,
-0.553846153846154,-0.538461538461538,-0.523076923076923,-0.507692307692308,
-0.492307692307692,-0.476923076923077,-0.461538461538462,-0.446153846153846,
-0.430769230769231,-0.415384615384615,-0.4,-0.384615384615385,-0.369230769230769,
-0.353846153846154,-0.338461538461538,-0.323076923076923,-0.307692307692308,
-0.292307692307692,-0.276923076923077,-0.261538461538462,-0.246153846153846,
-0.230769230769231,-0.215384615384615,-0.2,-0.184615384615385,-0.169230769230769,
-0.153846153846154,-0.138461538461538,-0.123076923076923,-0.107692307692308,
-0.0923076923076923,-0.0769230769230769,-0.0615384615384615,-0.0461538461538462,
-0.0307692307692308,-0.0153846153846154,0.),(-1.,1.),.UNSPECIFIED.)
GEOMETRIC_REPRESENTATION_ITEM()
RATIONAL_B_SPLINE_SURFACE(((1.,1.),(1.,1.),(1.,1.),(1.,1.),(1.,1.),(1.,
1.),(1.,1.),(1.,1.),(1.,1.),(1.,1.),(1.,1.),(1.,1.),(1.,1.),(1.,1.),(1.,
1.),(1.,1.),(1.,1.),(1.,1.),(1.,1.),(1.,1.),(1.,1.),(1.,1.),(1.,1.),(1.,
1.),(1.,1.),(1.,1.),(1.,1.),(1.,1.),(1.,1.),(1.,1.),(1.,1.),(1.,1.),(1.,
1.),(1.,1.),(1.,1.),(1.,1.),(1.,1.),(1.,1.),(1.,1.),(1.,1.),(1.,1.),(1.,
1.),(1.,1.),(1.,1.),(1.,1.),(1.,1.),(1.,1.),(1.,1.),(1.,1.),(1.,1.),(1.,
1.),(1.,1.),(1.,1.),(1.,1.),(1.,1.),(1.,1.),(1.,1.),(1.,1.),(1.,1.),(1.,
1.),(1.,1.),(1.,1.),(1.,1.),(1.,1.),(1.,1.),(1.,1.),(1.,1.),(1.,1.),(1.,
1.),(1.,1.)))
REPRESENTATION_ITEM('')
SURFACE()
);
#13=(
BOUNDED_SURFACE()
B_SPLINE_SURFACE(5,1,((#25610,#25611),(#25612,#25613),(#25614,#25615),(#25616,
#25617),(#25618,#25619),(#25620,#25621),(#25622,#25623),(#25624,#25625),
(#25626,#25627),(#25628,#25629),(#25630,#25631),(#25632,#25633),(#25634,
#25635),(#25636,#25637),(#25638,#25639),(#25640,#25641),(#25642,#25643),
(#25644,#25645),(#25646,#25647),(#25648,#25649),(#25650,#25651),(#25652,
#25653),(#25654,#25655),(#25656,#25657),(#25658,#25659),(#25660,#25661),
(#25662,#25663),(#25664,#25665),(#25666,#25667),(#25668,#25669),(#25670,
#25671),(#25672,#25673),(#25674,#25675),(#25676,#25677),(#25678,#25679),
(#25680,#25681),(#25682,#25683),(#25684,#25685),(#25686,#25687),(#25688,
#25689),(#25690,#25691),(#25692,#25693),(#25694,#25695),(#25696,#25697),
(#25698,#25699),(#25700,#25701),(#25702,#25703),(#25704,#25705),(#25706,
#25707),(#25708,#25709),(#25710,#25711),(#25712,#25713),(#25714,#25715),
(#25716,#25717),(#25718,#25719),(#25720,#25721),(#25722,#25723),(#25724,
#25725),(#25726,#25727),(#25728,#25729),(#25730,#25731),(#25732,#25733),
(#25734,#25735),(#25736,#25737),(#25738,#25739),(#25740,#25741),(#25742,
#25743),(#25744,#25745),(#25746,#25747),(#25748,#25749)),.UNSPECIFIED.,
 .F.,.F.,.F.)
B_SPLINE_SURFACE_WITH_KNOTS((6,1,1,1,1,1,1,1,1,1,1,1,1,1,1,1,1,1,1,1,1,
1,1,1,1,1,1,1,1,1,1,1,1,1,1,1,1,1,1,1,1,1,1,1,1,1,1,1,1,1,1,1,1,1,1,1,1,
1,1,1,1,1,1,1,1,6),(2,2),(-1.,-0.984615384615383,-0.969230769230768,-0.953846153846152,
-0.938461538461537,-0.923076923076922,-0.907692307692306,-0.892307692307691,
-0.876923076923076,-0.86153846153846,-0.846153846153845,-0.83076923076923,
-0.815384615384614,-0.799999999999999,-0.784615384615384,-0.769230769230768,
-0.753846153846153,-0.738461538461538,-0.723076923076922,-0.707692307692307,
-0.692307692307692,-0.676923076923076,-0.661538461538461,-0.646153846153846,
-0.63076923076923,-0.615384615384615,-0.6,-0.584615384615384,-0.569230769230769,
-0.553846153846154,-0.538461538461538,-0.523076923076923,-0.507692307692308,
-0.492307692307692,-0.476923076923077,-0.461538461538462,-0.446153846153846,
-0.430769230769231,-0.415384615384615,-0.4,-0.384615384615385,-0.369230769230769,
-0.353846153846154,-0.338461538461538,-0.323076923076923,-0.307692307692308,
-0.292307692307692,-0.276923076923077,-0.261538461538462,-0.246153846153846,
-0.230769230769231,-0.215384615384615,-0.2,-0.184615384615385,-0.169230769230769,
-0.153846153846154,-0.138461538461538,-0.123076923076923,-0.107692307692308,
-0.0923076923076923,-0.0769230769230769,-0.0615384615384615,-0.0461538461538462,
-0.0307692307692308,-0.0153846153846154,0.),(-1.,1.),.UNSPECIFIED.)
GEOMETRIC_REPRESENTATION_ITEM()
RATIONAL_B_SPLINE_SURFACE(((1.,1.),(1.,1.),(1.,1.),(1.,1.),(1.,1.),(1.,
1.),(1.,1.),(1.,1.),(1.,1.),(1.,1.),(1.,1.),(1.,1.),(1.,1.),(1.,1.),(1.,
1.),(1.,1.),(1.,1.),(1.,1.),(1.,1.),(1.,1.),(1.,1.),(1.,1.),(1.,1.),(1.,
1.),(1.,1.),(1.,1.),(1.,1.),(1.,1.),(1.,1.),(1.,1.),(1.,1.),(1.,1.),(1.,
1.),(1.,1.),(1.,1.),(1.,1.),(1.,1.),(1.,1.),(1.,1.),(1.,1.),(1.,1.),(1.,
1.),(1.,1.),(1.,1.),(1.,1.),(1.,1.),(1.,1.),(1.,1.),(1.,1.),(1.,1.),(1.,
1.),(1.,1.),(1.,1.),(1.,1.),(1.,1.),(1.,1.),(1.,1.),(1.,1.),(1.,1.),(1.,
1.),(1.,1.),(1.,1.),(1.,1.),(1.,1.),(1.,1.),(1.,1.),(1.,1.),(1.,1.),(1.,
1.),(1.,1.)))
REPRESENTATION_ITEM('')
SURFACE()
);
#14=(
BOUNDED_SURFACE()
B_SPLINE_SURFACE(5,1,((#25826,#25827),(#25828,#25829),(#25830,#25831),(#25832,
#25833),(#25834,#25835),(#25836,#25837),(#25838,#25839),(#25840,#25841),
(#25842,#25843),(#25844,#25845),(#25846,#25847),(#25848,#25849),(#25850,
#25851),(#25852,#25853),(#25854,#25855),(#25856,#25857),(#25858,#25859),
(#25860,#25861),(#25862,#25863),(#25864,#25865),(#25866,#25867),(#25868,
#25869),(#25870,#25871),(#25872,#25873),(#25874,#25875),(#25876,#25877),
(#25878,#25879),(#25880,#25881),(#25882,#25883),(#25884,#25885),(#25886,
#25887),(#25888,#25889),(#25890,#25891),(#25892,#25893),(#25894,#25895),
(#25896,#25897),(#25898,#25899),(#25900,#25901),(#25902,#25903),(#25904,
#25905),(#25906,#25907),(#25908,#25909),(#25910,#25911),(#25912,#25913),
(#25914,#25915),(#25916,#25917),(#25918,#25919),(#25920,#25921),(#25922,
#25923),(#25924,#25925),(#25926,#25927),(#25928,#25929),(#25930,#25931),
(#25932,#25933),(#25934,#25935),(#25936,#25937),(#25938,#25939),(#25940,
#25941),(#25942,#25943),(#25944,#25945),(#25946,#25947),(#25948,#25949),
(#25950,#25951),(#25952,#25953),(#25954,#25955),(#25956,#25957),(#25958,
#25959),(#25960,#25961),(#25962,#25963),(#25964,#25965)),.UNSPECIFIED.,
 .F.,.F.,.F.)
B_SPLINE_SURFACE_WITH_KNOTS((6,1,1,1,1,1,1,1,1,1,1,1,1,1,1,1,1,1,1,1,1,
1,1,1,1,1,1,1,1,1,1,1,1,1,1,1,1,1,1,1,1,1,1,1,1,1,1,1,1,1,1,1,1,1,1,1,1,
1,1,1,1,1,1,1,1,6),(2,2),(-1.,-0.984615384615383,-0.969230769230768,-0.953846153846152,
-0.938461538461537,-0.923076923076922,-0.907692307692306,-0.892307692307691,
-0.876923076923076,-0.86153846153846,-0.846153846153845,-0.83076923076923,
-0.815384615384614,-0.799999999999999,-0.784615384615384,-0.769230769230768,
-0.753846153846153,-0.738461538461538,-0.723076923076922,-0.707692307692307,
-0.692307692307692,-0.676923076923076,-0.661538461538461,-0.646153846153846,
-0.63076923076923,-0.615384615384615,-0.6,-0.584615384615384,-0.569230769230769,
-0.553846153846154,-0.538461538461538,-0.523076923076923,-0.507692307692308,
-0.492307692307692,-0.476923076923077,-0.461538461538462,-0.446153846153846,
-0.430769230769231,-0.415384615384615,-0.4,-0.384615384615385,-0.369230769230769,
-0.353846153846154,-0.338461538461538,-0.323076923076923,-0.307692307692308,
-0.292307692307692,-0.276923076923077,-0.261538461538462,-0.246153846153846,
-0.230769230769231,-0.215384615384615,-0.2,-0.184615384615385,-0.169230769230769,
-0.153846153846154,-0.138461538461538,-0.123076923076923,-0.107692307692308,
-0.0923076923076923,-0.0769230769230769,-0.0615384615384615,-0.0461538461538462,
-0.0307692307692308,-0.0153846153846154,0.),(-1.,1.),.UNSPECIFIED.)
GEOMETRIC_REPRESENTATION_ITEM()
RATIONAL_B_SPLINE_SURFACE(((1.,1.),(1.,1.),(1.,1.),(1.,1.),(1.,1.),(1.,
1.),(1.,1.),(1.,1.),(1.,1.),(1.,1.),(1.,1.),(1.,1.),(1.,1.),(1.,1.),(1.,
1.),(1.,1.),(1.,1.),(1.,1.),(1.,1.),(1.,1.),(1.,1.),(1.,1.),(1.,1.),(1.,
1.),(1.,1.),(1.,1.),(1.,1.),(1.,1.),(1.,1.),(1.,1.),(1.,1.),(1.,1.),(1.,
1.),(1.,1.),(1.,1.),(1.,1.),(1.,1.),(1.,1.),(1.,1.),(1.,1.),(1.,1.),(1.,
1.),(1.,1.),(1.,1.),(1.,1.),(1.,1.),(1.,1.),(1.,1.),(1.,1.),(1.,1.),(1.,
1.),(1.,1.),(1.,1.),(1.,1.),(1.,1.),(1.,1.),(1.,1.),(1.,1.),(1.,1.),(1.,
1.),(1.,1.),(1.,1.),(1.,1.),(1.,1.),(1.,1.),(1.,1.),(1.,1.),(1.,1.),(1.,
1.),(1.,1.)))
REPRESENTATION_ITEM('')
SURFACE()
);
#15=(
BOUNDED_SURFACE()
B_SPLINE_SURFACE(5,1,((#26042,#26043),(#26044,#26045),(#26046,#26047),(#26048,
#26049),(#26050,#26051),(#26052,#26053),(#26054,#26055),(#26056,#26057),
(#26058,#26059),(#26060,#26061),(#26062,#26063),(#26064,#26065),(#26066,
#26067),(#26068,#26069),(#26070,#26071),(#26072,#26073),(#26074,#26075),
(#26076,#26077),(#26078,#26079),(#26080,#26081),(#26082,#26083),(#26084,
#26085),(#26086,#26087),(#26088,#26089),(#26090,#26091),(#26092,#26093),
(#26094,#26095),(#26096,#26097),(#26098,#26099),(#26100,#26101),(#26102,
#26103),(#26104,#26105),(#26106,#26107),(#26108,#26109),(#26110,#26111),
(#26112,#26113),(#26114,#26115),(#26116,#26117),(#26118,#26119),(#26120,
#26121),(#26122,#26123),(#26124,#26125),(#26126,#26127),(#26128,#26129),
(#26130,#26131),(#26132,#26133),(#26134,#26135),(#26136,#26137),(#26138,
#26139),(#26140,#26141),(#26142,#26143),(#26144,#26145),(#26146,#26147),
(#26148,#26149),(#26150,#26151),(#26152,#26153),(#26154,#26155),(#26156,
#26157),(#26158,#26159),(#26160,#26161),(#26162,#26163),(#26164,#26165),
(#26166,#26167),(#26168,#26169),(#26170,#26171),(#26172,#26173),(#26174,
#26175),(#26176,#26177),(#26178,#26179),(#26180,#26181)),.UNSPECIFIED.,
 .F.,.F.,.F.)
B_SPLINE_SURFACE_WITH_KNOTS((6,1,1,1,1,1,1,1,1,1,1,1,1,1,1,1,1,1,1,1,1,
1,1,1,1,1,1,1,1,1,1,1,1,1,1,1,1,1,1,1,1,1,1,1,1,1,1,1,1,1,1,1,1,1,1,1,1,
1,1,1,1,1,1,1,1,6),(2,2),(-1.,-0.984615384615383,-0.969230769230768,-0.953846153846152,
-0.938461538461537,-0.923076923076922,-0.907692307692306,-0.892307692307691,
-0.876923076923076,-0.86153846153846,-0.846153846153845,-0.83076923076923,
-0.815384615384614,-0.799999999999999,-0.784615384615384,-0.769230769230768,
-0.753846153846153,-0.738461538461538,-0.723076923076922,-0.707692307692307,
-0.692307692307692,-0.676923076923076,-0.661538461538461,-0.646153846153846,
-0.63076923076923,-0.615384615384615,-0.6,-0.584615384615384,-0.569230769230769,
-0.553846153846154,-0.538461538461538,-0.523076923076923,-0.507692307692308,
-0.492307692307692,-0.476923076923077,-0.461538461538462,-0.446153846153846,
-0.430769230769231,-0.415384615384615,-0.4,-0.384615384615385,-0.369230769230769,
-0.353846153846154,-0.338461538461538,-0.323076923076923,-0.307692307692308,
-0.292307692307692,-0.276923076923077,-0.261538461538462,-0.246153846153846,
-0.230769230769231,-0.215384615384615,-0.2,-0.184615384615385,-0.169230769230769,
-0.153846153846154,-0.138461538461538,-0.123076923076923,-0.107692307692308,
-0.0923076923076923,-0.0769230769230769,-0.0615384615384615,-0.0461538461538462,
-0.0307692307692308,-0.0153846153846154,0.),(-1.,1.),.UNSPECIFIED.)
GEOMETRIC_REPRESENTATION_ITEM()
RATIONAL_B_SPLINE_SURFACE(((1.,1.),(1.,1.),(1.,1.),(1.,1.),(1.,1.),(1.,
1.),(1.,1.),(1.,1.),(1.,1.),(1.,1.),(1.,1.),(1.,1.),(1.,1.),(1.,1.),(1.,
1.),(1.,1.),(1.,1.),(1.,1.),(1.,1.),(1.,1.),(1.,1.),(1.,1.),(1.,1.),(1.,
1.),(1.,1.),(1.,1.),(1.,1.),(1.,1.),(1.,1.),(1.,1.),(1.,1.),(1.,1.),(1.,
1.),(1.,1.),(1.,1.),(1.,1.),(1.,1.),(1.,1.),(1.,1.),(1.,1.),(1.,1.),(1.,
1.),(1.,1.),(1.,1.),(1.,1.),(1.,1.),(1.,1.),(1.,1.),(1.,1.),(1.,1.),(1.,
1.),(1.,1.),(1.,1.),(1.,1.),(1.,1.),(1.,1.),(1.,1.),(1.,1.),(1.,1.),(1.,
1.),(1.,1.),(1.,1.),(1.,1.),(1.,1.),(1.,1.),(1.,1.),(1.,1.),(1.,1.),(1.,
1.),(1.,1.)))
REPRESENTATION_ITEM('')
SURFACE()
);
#16=(
BOUNDED_SURFACE()
B_SPLINE_SURFACE(5,1,((#26258,#26259),(#26260,#26261),(#26262,#26263),(#26264,
#26265),(#26266,#26267),(#26268,#26269),(#26270,#26271),(#26272,#26273),
(#26274,#26275),(#26276,#26277),(#26278,#26279),(#26280,#26281),(#26282,
#26283),(#26284,#26285),(#26286,#26287),(#26288,#26289),(#26290,#26291),
(#26292,#26293),(#26294,#26295),(#26296,#26297),(#26298,#26299),(#26300,
#26301),(#26302,#26303),(#26304,#26305),(#26306,#26307),(#26308,#26309),
(#26310,#26311),(#26312,#26313),(#26314,#26315),(#26316,#26317),(#26318,
#26319),(#26320,#26321),(#26322,#26323),(#26324,#26325),(#26326,#26327),
(#26328,#26329),(#26330,#26331),(#26332,#26333),(#26334,#26335),(#26336,
#26337),(#26338,#26339),(#26340,#26341),(#26342,#26343),(#26344,#26345),
(#26346,#26347),(#26348,#26349),(#26350,#26351),(#26352,#26353),(#26354,
#26355),(#26356,#26357),(#26358,#26359),(#26360,#26361),(#26362,#26363),
(#26364,#26365),(#26366,#26367),(#26368,#26369),(#26370,#26371),(#26372,
#26373),(#26374,#26375),(#26376,#26377),(#26378,#26379),(#26380,#26381),
(#26382,#26383),(#26384,#26385),(#26386,#26387),(#26388,#26389),(#26390,
#26391),(#26392,#26393),(#26394,#26395),(#26396,#26397)),.UNSPECIFIED.,
 .F.,.F.,.F.)
B_SPLINE_SURFACE_WITH_KNOTS((6,1,1,1,1,1,1,1,1,1,1,1,1,1,1,1,1,1,1,1,1,
1,1,1,1,1,1,1,1,1,1,1,1,1,1,1,1,1,1,1,1,1,1,1,1,1,1,1,1,1,1,1,1,1,1,1,1,
1,1,1,1,1,1,1,1,6),(2,2),(-1.,-0.984615384615383,-0.969230769230768,-0.953846153846152,
-0.938461538461537,-0.923076923076922,-0.907692307692306,-0.892307692307691,
-0.876923076923076,-0.86153846153846,-0.846153846153845,-0.83076923076923,
-0.815384615384614,-0.799999999999999,-0.784615384615384,-0.769230769230768,
-0.753846153846153,-0.738461538461538,-0.723076923076922,-0.707692307692307,
-0.692307692307692,-0.676923076923076,-0.661538461538461,-0.646153846153846,
-0.63076923076923,-0.615384615384615,-0.6,-0.584615384615384,-0.569230769230769,
-0.553846153846154,-0.538461538461538,-0.523076923076923,-0.507692307692308,
-0.492307692307692,-0.476923076923077,-0.461538461538462,-0.446153846153846,
-0.430769230769231,-0.415384615384615,-0.4,-0.384615384615385,-0.369230769230769,
-0.353846153846154,-0.338461538461538,-0.323076923076923,-0.307692307692308,
-0.292307692307692,-0.276923076923077,-0.261538461538462,-0.246153846153846,
-0.230769230769231,-0.215384615384615,-0.2,-0.184615384615385,-0.169230769230769,
-0.153846153846154,-0.138461538461538,-0.123076923076923,-0.107692307692308,
-0.0923076923076923,-0.0769230769230769,-0.0615384615384615,-0.0461538461538462,
-0.0307692307692308,-0.0153846153846154,0.),(-1.,1.),.UNSPECIFIED.)
GEOMETRIC_REPRESENTATION_ITEM()
RATIONAL_B_SPLINE_SURFACE(((1.,1.),(1.,1.),(1.,1.),(1.,1.),(1.,1.),(1.,
1.),(1.,1.),(1.,1.),(1.,1.),(1.,1.),(1.,1.),(1.,1.),(1.,1.),(1.,1.),(1.,
1.),(1.,1.),(1.,1.),(1.,1.),(1.,1.),(1.,1.),(1.,1.),(1.,1.),(1.,1.),(1.,
1.),(1.,1.),(1.,1.),(1.,1.),(1.,1.),(1.,1.),(1.,1.),(1.,1.),(1.,1.),(1.,
1.),(1.,1.),(1.,1.),(1.,1.),(1.,1.),(1.,1.),(1.,1.),(1.,1.),(1.,1.),(1.,
1.),(1.,1.),(1.,1.),(1.,1.),(1.,1.),(1.,1.),(1.,1.),(1.,1.),(1.,1.),(1.,
1.),(1.,1.),(1.,1.),(1.,1.),(1.,1.),(1.,1.),(1.,1.),(1.,1.),(1.,1.),(1.,
1.),(1.,1.),(1.,1.),(1.,1.),(1.,1.),(1.,1.),(1.,1.),(1.,1.),(1.,1.),(1.,
1.),(1.,1.)))
REPRESENTATION_ITEM('')
SURFACE()
);
#17=(
BOUNDED_SURFACE()
B_SPLINE_SURFACE(5,1,((#26474,#26475),(#26476,#26477),(#26478,#26479),(#26480,
#26481),(#26482,#26483),(#26484,#26485),(#26486,#26487),(#26488,#26489),
(#26490,#26491),(#26492,#26493),(#26494,#26495),(#26496,#26497),(#26498,
#26499),(#26500,#26501),(#26502,#26503),(#26504,#26505),(#26506,#26507),
(#26508,#26509),(#26510,#26511),(#26512,#26513),(#26514,#26515),(#26516,
#26517),(#26518,#26519),(#26520,#26521),(#26522,#26523),(#26524,#26525),
(#26526,#26527),(#26528,#26529),(#26530,#26531),(#26532,#26533),(#26534,
#26535),(#26536,#26537),(#26538,#26539),(#26540,#26541),(#26542,#26543),
(#26544,#26545),(#26546,#26547),(#26548,#26549),(#26550,#26551),(#26552,
#26553),(#26554,#26555),(#26556,#26557),(#26558,#26559),(#26560,#26561),
(#26562,#26563),(#26564,#26565),(#26566,#26567),(#26568,#26569),(#26570,
#26571),(#26572,#26573),(#26574,#26575),(#26576,#26577),(#26578,#26579),
(#26580,#26581),(#26582,#26583),(#26584,#26585),(#26586,#26587),(#26588,
#26589),(#26590,#26591),(#26592,#26593),(#26594,#26595),(#26596,#26597),
(#26598,#26599),(#26600,#26601),(#26602,#26603),(#26604,#26605),(#26606,
#26607),(#26608,#26609),(#26610,#26611),(#26612,#26613)),.UNSPECIFIED.,
 .F.,.F.,.F.)
B_SPLINE_SURFACE_WITH_KNOTS((6,1,1,1,1,1,1,1,1,1,1,1,1,1,1,1,1,1,1,1,1,
1,1,1,1,1,1,1,1,1,1,1,1,1,1,1,1,1,1,1,1,1,1,1,1,1,1,1,1,1,1,1,1,1,1,1,1,
1,1,1,1,1,1,1,1,6),(2,2),(-1.,-0.984615384615383,-0.969230769230768,-0.953846153846152,
-0.938461538461537,-0.923076923076922,-0.907692307692306,-0.892307692307691,
-0.876923076923076,-0.86153846153846,-0.846153846153845,-0.83076923076923,
-0.815384615384614,-0.799999999999999,-0.784615384615384,-0.769230769230768,
-0.753846153846153,-0.738461538461538,-0.723076923076922,-0.707692307692307,
-0.692307692307692,-0.676923076923076,-0.661538461538461,-0.646153846153846,
-0.63076923076923,-0.615384615384615,-0.6,-0.584615384615384,-0.569230769230769,
-0.553846153846154,-0.538461538461538,-0.523076923076923,-0.507692307692308,
-0.492307692307692,-0.476923076923077,-0.461538461538462,-0.446153846153846,
-0.430769230769231,-0.415384615384615,-0.4,-0.384615384615385,-0.369230769230769,
-0.353846153846154,-0.338461538461538,-0.323076923076923,-0.307692307692308,
-0.292307692307692,-0.276923076923077,-0.261538461538462,-0.246153846153846,
-0.230769230769231,-0.215384615384615,-0.2,-0.184615384615385,-0.169230769230769,
-0.153846153846154,-0.138461538461538,-0.123076923076923,-0.107692307692308,
-0.0923076923076923,-0.0769230769230769,-0.0615384615384615,-0.0461538461538462,
-0.0307692307692308,-0.0153846153846154,0.),(-1.,1.),.UNSPECIFIED.)
GEOMETRIC_REPRESENTATION_ITEM()
RATIONAL_B_SPLINE_SURFACE(((1.,1.),(1.,1.),(1.,1.),(1.,1.),(1.,1.),(1.,
1.),(1.,1.),(1.,1.),(1.,1.),(1.,1.),(1.,1.),(1.,1.),(1.,1.),(1.,1.),(1.,
1.),(1.,1.),(1.,1.),(1.,1.),(1.,1.),(1.,1.),(1.,1.),(1.,1.),(1.,1.),(1.,
1.),(1.,1.),(1.,1.),(1.,1.),(1.,1.),(1.,1.),(1.,1.),(1.,1.),(1.,1.),(1.,
1.),(1.,1.),(1.,1.),(1.,1.),(1.,1.),(1.,1.),(1.,1.),(1.,1.),(1.,1.),(1.,
1.),(1.,1.),(1.,1.),(1.,1.),(1.,1.),(1.,1.),(1.,1.),(1.,1.),(1.,1.),(1.,
1.),(1.,1.),(1.,1.),(1.,1.),(1.,1.),(1.,1.),(1.,1.),(1.,1.),(1.,1.),(1.,
1.),(1.,1.),(1.,1.),(1.,1.),(1.,1.),(1.,1.),(1.,1.),(1.,1.),(1.,1.),(1.,
1.),(1.,1.)))
REPRESENTATION_ITEM('')
SURFACE()
);
#18=(
BOUNDED_SURFACE()
B_SPLINE_SURFACE(5,1,((#26690,#26691),(#26692,#26693),(#26694,#26695),(#26696,
#26697),(#26698,#26699),(#26700,#26701),(#26702,#26703),(#26704,#26705),
(#26706,#26707),(#26708,#26709),(#26710,#26711),(#26712,#26713),(#26714,
#26715),(#26716,#26717),(#26718,#26719),(#26720,#26721),(#26722,#26723),
(#26724,#26725),(#26726,#26727),(#26728,#26729),(#26730,#26731),(#26732,
#26733),(#26734,#26735),(#26736,#26737),(#26738,#26739),(#26740,#26741),
(#26742,#26743),(#26744,#26745),(#26746,#26747),(#26748,#26749),(#26750,
#26751),(#26752,#26753),(#26754,#26755),(#26756,#26757),(#26758,#26759),
(#26760,#26761),(#26762,#26763),(#26764,#26765),(#26766,#26767),(#26768,
#26769),(#26770,#26771),(#26772,#26773),(#26774,#26775),(#26776,#26777),
(#26778,#26779),(#26780,#26781),(#26782,#26783),(#26784,#26785),(#26786,
#26787),(#26788,#26789),(#26790,#26791),(#26792,#26793),(#26794,#26795),
(#26796,#26797),(#26798,#26799),(#26800,#26801),(#26802,#26803),(#26804,
#26805),(#26806,#26807),(#26808,#26809),(#26810,#26811),(#26812,#26813),
(#26814,#26815),(#26816,#26817),(#26818,#26819),(#26820,#26821),(#26822,
#26823),(#26824,#26825),(#26826,#26827),(#26828,#26829)),.UNSPECIFIED.,
 .F.,.F.,.F.)
B_SPLINE_SURFACE_WITH_KNOTS((6,1,1,1,1,1,1,1,1,1,1,1,1,1,1,1,1,1,1,1,1,
1,1,1,1,1,1,1,1,1,1,1,1,1,1,1,1,1,1,1,1,1,1,1,1,1,1,1,1,1,1,1,1,1,1,1,1,
1,1,1,1,1,1,1,1,6),(2,2),(-1.,-0.984615384615383,-0.969230769230768,-0.953846153846152,
-0.938461538461537,-0.923076923076922,-0.907692307692306,-0.892307692307691,
-0.876923076923076,-0.86153846153846,-0.846153846153845,-0.83076923076923,
-0.815384615384614,-0.799999999999999,-0.784615384615384,-0.769230769230768,
-0.753846153846153,-0.738461538461538,-0.723076923076922,-0.707692307692307,
-0.692307692307692,-0.676923076923076,-0.661538461538461,-0.646153846153846,
-0.63076923076923,-0.615384615384615,-0.6,-0.584615384615384,-0.569230769230769,
-0.553846153846154,-0.538461538461538,-0.523076923076923,-0.507692307692308,
-0.492307692307692,-0.476923076923077,-0.461538461538462,-0.446153846153846,
-0.430769230769231,-0.415384615384615,-0.4,-0.384615384615385,-0.369230769230769,
-0.353846153846154,-0.338461538461538,-0.323076923076923,-0.307692307692308,
-0.292307692307692,-0.276923076923077,-0.261538461538462,-0.246153846153846,
-0.230769230769231,-0.215384615384615,-0.2,-0.184615384615385,-0.169230769230769,
-0.153846153846154,-0.138461538461538,-0.123076923076923,-0.107692307692308,
-0.0923076923076923,-0.0769230769230769,-0.0615384615384615,-0.0461538461538462,
-0.0307692307692308,-0.0153846153846154,0.),(-1.,1.),.UNSPECIFIED.)
GEOMETRIC_REPRESENTATION_ITEM()
RATIONAL_B_SPLINE_SURFACE(((1.,1.),(1.,1.),(1.,1.),(1.,1.),(1.,1.),(1.,
1.),(1.,1.),(1.,1.),(1.,1.),(1.,1.),(1.,1.),(1.,1.),(1.,1.),(1.,1.),(1.,
1.),(1.,1.),(1.,1.),(1.,1.),(1.,1.),(1.,1.),(1.,1.),(1.,1.),(1.,1.),(1.,
1.),(1.,1.),(1.,1.),(1.,1.),(1.,1.),(1.,1.),(1.,1.),(1.,1.),(1.,1.),(1.,
1.),(1.,1.),(1.,1.),(1.,1.),(1.,1.),(1.,1.),(1.,1.),(1.,1.),(1.,1.),(1.,
1.),(1.,1.),(1.,1.),(1.,1.),(1.,1.),(1.,1.),(1.,1.),(1.,1.),(1.,1.),(1.,
1.),(1.,1.),(1.,1.),(1.,1.),(1.,1.),(1.,1.),(1.,1.),(1.,1.),(1.,1.),(1.,
1.),(1.,1.),(1.,1.),(1.,1.),(1.,1.),(1.,1.),(1.,1.),(1.,1.),(1.,1.),(1.,
1.),(1.,1.)))
REPRESENTATION_ITEM('')
SURFACE()
);
#19=(
BOUNDED_SURFACE()
B_SPLINE_SURFACE(5,1,((#26906,#26907),(#26908,#26909),(#26910,#26911),(#26912,
#26913),(#26914,#26915),(#26916,#26917),(#26918,#26919),(#26920,#26921),
(#26922,#26923),(#26924,#26925),(#26926,#26927),(#26928,#26929),(#26930,
#26931),(#26932,#26933),(#26934,#26935),(#26936,#26937),(#26938,#26939),
(#26940,#26941),(#26942,#26943),(#26944,#26945),(#26946,#26947),(#26948,
#26949),(#26950,#26951),(#26952,#26953),(#26954,#26955),(#26956,#26957),
(#26958,#26959),(#26960,#26961),(#26962,#26963),(#26964,#26965),(#26966,
#26967),(#26968,#26969),(#26970,#26971),(#26972,#26973),(#26974,#26975),
(#26976,#26977),(#26978,#26979),(#26980,#26981),(#26982,#26983),(#26984,
#26985),(#26986,#26987),(#26988,#26989),(#26990,#26991),(#26992,#26993),
(#26994,#26995),(#26996,#26997),(#26998,#26999),(#27000,#27001),(#27002,
#27003),(#27004,#27005),(#27006,#27007),(#27008,#27009),(#27010,#27011),
(#27012,#27013),(#27014,#27015),(#27016,#27017),(#27018,#27019),(#27020,
#27021),(#27022,#27023),(#27024,#27025),(#27026,#27027),(#27028,#27029),
(#27030,#27031),(#27032,#27033),(#27034,#27035),(#27036,#27037),(#27038,
#27039),(#27040,#27041),(#27042,#27043),(#27044,#27045)),.UNSPECIFIED.,
 .F.,.F.,.F.)
B_SPLINE_SURFACE_WITH_KNOTS((6,1,1,1,1,1,1,1,1,1,1,1,1,1,1,1,1,1,1,1,1,
1,1,1,1,1,1,1,1,1,1,1,1,1,1,1,1,1,1,1,1,1,1,1,1,1,1,1,1,1,1,1,1,1,1,1,1,
1,1,1,1,1,1,1,1,6),(2,2),(-1.,-0.984615384615383,-0.969230769230768,-0.953846153846152,
-0.938461538461537,-0.923076923076922,-0.907692307692306,-0.892307692307691,
-0.876923076923076,-0.86153846153846,-0.846153846153845,-0.83076923076923,
-0.815384615384614,-0.799999999999999,-0.784615384615384,-0.769230769230768,
-0.753846153846153,-0.738461538461538,-0.723076923076922,-0.707692307692307,
-0.692307692307692,-0.676923076923076,-0.661538461538461,-0.646153846153846,
-0.63076923076923,-0.615384615384615,-0.6,-0.584615384615384,-0.569230769230769,
-0.553846153846154,-0.538461538461538,-0.523076923076923,-0.507692307692308,
-0.492307692307692,-0.476923076923077,-0.461538461538462,-0.446153846153846,
-0.430769230769231,-0.415384615384615,-0.4,-0.384615384615385,-0.369230769230769,
-0.353846153846154,-0.338461538461538,-0.323076923076923,-0.307692307692308,
-0.292307692307692,-0.276923076923077,-0.261538461538462,-0.246153846153846,
-0.230769230769231,-0.215384615384615,-0.2,-0.184615384615385,-0.169230769230769,
-0.153846153846154,-0.138461538461538,-0.123076923076923,-0.107692307692308,
-0.0923076923076923,-0.0769230769230769,-0.0615384615384615,-0.0461538461538462,
-0.0307692307692308,-0.0153846153846154,0.),(-1.,1.),.UNSPECIFIED.)
GEOMETRIC_REPRESENTATION_ITEM()
RATIONAL_B_SPLINE_SURFACE(((1.,1.),(1.,1.),(1.,1.),(1.,1.),(1.,1.),(1.,
1.),(1.,1.),(1.,1.),(1.,1.),(1.,1.),(1.,1.),(1.,1.),(1.,1.),(1.,1.),(1.,
1.),(1.,1.),(1.,1.),(1.,1.),(1.,1.),(1.,1.),(1.,1.),(1.,1.),(1.,1.),(1.,
1.),(1.,1.),(1.,1.),(1.,1.),(1.,1.),(1.,1.),(1.,1.),(1.,1.),(1.,1.),(1.,
1.),(1.,1.),(1.,1.),(1.,1.),(1.,1.),(1.,1.),(1.,1.),(1.,1.),(1.,1.),(1.,
1.),(1.,1.),(1.,1.),(1.,1.),(1.,1.),(1.,1.),(1.,1.),(1.,1.),(1.,1.),(1.,
1.),(1.,1.),(1.,1.),(1.,1.),(1.,1.),(1.,1.),(1.,1.),(1.,1.),(1.,1.),(1.,
1.),(1.,1.),(1.,1.),(1.,1.),(1.,1.),(1.,1.),(1.,1.),(1.,1.),(1.,1.),(1.,
1.),(1.,1.)))
REPRESENTATION_ITEM('')
SURFACE()
);
#20=(
BOUNDED_SURFACE()
B_SPLINE_SURFACE(5,1,((#27122,#27123),(#27124,#27125),(#27126,#27127),(#27128,
#27129),(#27130,#27131),(#27132,#27133),(#27134,#27135),(#27136,#27137),
(#27138,#27139),(#27140,#27141),(#27142,#27143),(#27144,#27145),(#27146,
#27147),(#27148,#27149),(#27150,#27151),(#27152,#27153),(#27154,#27155),
(#27156,#27157),(#27158,#27159),(#27160,#27161),(#27162,#27163),(#27164,
#27165),(#27166,#27167),(#27168,#27169),(#27170,#27171),(#27172,#27173),
(#27174,#27175),(#27176,#27177),(#27178,#27179),(#27180,#27181),(#27182,
#27183),(#27184,#27185),(#27186,#27187),(#27188,#27189),(#27190,#27191),
(#27192,#27193),(#27194,#27195),(#27196,#27197),(#27198,#27199),(#27200,
#27201),(#27202,#27203),(#27204,#27205),(#27206,#27207),(#27208,#27209),
(#27210,#27211),(#27212,#27213),(#27214,#27215),(#27216,#27217),(#27218,
#27219),(#27220,#27221),(#27222,#27223),(#27224,#27225),(#27226,#27227),
(#27228,#27229),(#27230,#27231),(#27232,#27233),(#27234,#27235),(#27236,
#27237),(#27238,#27239),(#27240,#27241),(#27242,#27243),(#27244,#27245),
(#27246,#27247),(#27248,#27249),(#27250,#27251),(#27252,#27253),(#27254,
#27255),(#27256,#27257),(#27258,#27259),(#27260,#27261)),.UNSPECIFIED.,
 .F.,.F.,.F.)
B_SPLINE_SURFACE_WITH_KNOTS((6,1,1,1,1,1,1,1,1,1,1,1,1,1,1,1,1,1,1,1,1,
1,1,1,1,1,1,1,1,1,1,1,1,1,1,1,1,1,1,1,1,1,1,1,1,1,1,1,1,1,1,1,1,1,1,1,1,
1,1,1,1,1,1,1,1,6),(2,2),(-1.,-0.984615384615383,-0.969230769230768,-0.953846153846152,
-0.938461538461537,-0.923076923076922,-0.907692307692306,-0.892307692307691,
-0.876923076923076,-0.86153846153846,-0.846153846153845,-0.83076923076923,
-0.815384615384614,-0.799999999999999,-0.784615384615384,-0.769230769230768,
-0.753846153846153,-0.738461538461538,-0.723076923076922,-0.707692307692307,
-0.692307692307692,-0.676923076923076,-0.661538461538461,-0.646153846153846,
-0.63076923076923,-0.615384615384615,-0.6,-0.584615384615384,-0.569230769230769,
-0.553846153846154,-0.538461538461538,-0.523076923076923,-0.507692307692308,
-0.492307692307692,-0.476923076923077,-0.461538461538462,-0.446153846153846,
-0.430769230769231,-0.415384615384615,-0.4,-0.384615384615385,-0.369230769230769,
-0.353846153846154,-0.338461538461538,-0.323076923076923,-0.307692307692308,
-0.292307692307692,-0.276923076923077,-0.261538461538462,-0.246153846153846,
-0.230769230769231,-0.215384615384615,-0.2,-0.184615384615385,-0.169230769230769,
-0.153846153846154,-0.138461538461538,-0.123076923076923,-0.107692307692308,
-0.0923076923076923,-0.0769230769230769,-0.0615384615384615,-0.0461538461538462,
-0.0307692307692308,-0.0153846153846154,0.),(-1.,1.),.UNSPECIFIED.)
GEOMETRIC_REPRESENTATION_ITEM()
RATIONAL_B_SPLINE_SURFACE(((1.,1.),(1.,1.),(1.,1.),(1.,1.),(1.,1.),(1.,
1.),(1.,1.),(1.,1.),(1.,1.),(1.,1.),(1.,1.),(1.,1.),(1.,1.),(1.,1.),(1.,
1.),(1.,1.),(1.,1.),(1.,1.),(1.,1.),(1.,1.),(1.,1.),(1.,1.),(1.,1.),(1.,
1.),(1.,1.),(1.,1.),(1.,1.),(1.,1.),(1.,1.),(1.,1.),(1.,1.),(1.,1.),(1.,
1.),(1.,1.),(1.,1.),(1.,1.),(1.,1.),(1.,1.),(1.,1.),(1.,1.),(1.,1.),(1.,
1.),(1.,1.),(1.,1.),(1.,1.),(1.,1.),(1.,1.),(1.,1.),(1.,1.),(1.,1.),(1.,
1.),(1.,1.),(1.,1.),(1.,1.),(1.,1.),(1.,1.),(1.,1.),(1.,1.),(1.,1.),(1.,
1.),(1.,1.),(1.,1.),(1.,1.),(1.,1.),(1.,1.),(1.,1.),(1.,1.),(1.,1.),(1.,
1.),(1.,1.)))
REPRESENTATION_ITEM('')
SURFACE()
);
#21=(
BOUNDED_SURFACE()
B_SPLINE_SURFACE(5,1,((#27338,#27339),(#27340,#27341),(#27342,#27343),(#27344,
#27345),(#27346,#27347),(#27348,#27349),(#27350,#27351),(#27352,#27353),
(#27354,#27355),(#27356,#27357),(#27358,#27359),(#27360,#27361),(#27362,
#27363),(#27364,#27365),(#27366,#27367),(#27368,#27369),(#27370,#27371),
(#27372,#27373),(#27374,#27375),(#27376,#27377),(#27378,#27379),(#27380,
#27381),(#27382,#27383),(#27384,#27385),(#27386,#27387),(#27388,#27389),
(#27390,#27391),(#27392,#27393),(#27394,#27395),(#27396,#27397),(#27398,
#27399),(#27400,#27401),(#27402,#27403),(#27404,#27405),(#27406,#27407),
(#27408,#27409),(#27410,#27411),(#27412,#27413),(#27414,#27415),(#27416,
#27417),(#27418,#27419),(#27420,#27421),(#27422,#27423),(#27424,#27425),
(#27426,#27427),(#27428,#27429),(#27430,#27431),(#27432,#27433),(#27434,
#27435),(#27436,#27437),(#27438,#27439),(#27440,#27441),(#27442,#27443),
(#27444,#27445),(#27446,#27447),(#27448,#27449),(#27450,#27451),(#27452,
#27453),(#27454,#27455),(#27456,#27457),(#27458,#27459),(#27460,#27461),
(#27462,#27463),(#27464,#27465),(#27466,#27467),(#27468,#27469),(#27470,
#27471),(#27472,#27473),(#27474,#27475),(#27476,#27477)),.UNSPECIFIED.,
 .F.,.F.,.F.)
B_SPLINE_SURFACE_WITH_KNOTS((6,1,1,1,1,1,1,1,1,1,1,1,1,1,1,1,1,1,1,1,1,
1,1,1,1,1,1,1,1,1,1,1,1,1,1,1,1,1,1,1,1,1,1,1,1,1,1,1,1,1,1,1,1,1,1,1,1,
1,1,1,1,1,1,1,1,6),(2,2),(-1.,-0.984615384615383,-0.969230769230768,-0.953846153846152,
-0.938461538461537,-0.923076923076922,-0.907692307692306,-0.892307692307691,
-0.876923076923076,-0.86153846153846,-0.846153846153845,-0.83076923076923,
-0.815384615384614,-0.799999999999999,-0.784615384615384,-0.769230769230768,
-0.753846153846153,-0.738461538461538,-0.723076923076922,-0.707692307692307,
-0.692307692307692,-0.676923076923076,-0.661538461538461,-0.646153846153846,
-0.63076923076923,-0.615384615384615,-0.6,-0.584615384615384,-0.569230769230769,
-0.553846153846154,-0.538461538461538,-0.523076923076923,-0.507692307692308,
-0.492307692307692,-0.476923076923077,-0.461538461538462,-0.446153846153846,
-0.430769230769231,-0.415384615384615,-0.4,-0.384615384615385,-0.369230769230769,
-0.353846153846154,-0.338461538461538,-0.323076923076923,-0.307692307692308,
-0.292307692307692,-0.276923076923077,-0.261538461538462,-0.246153846153846,
-0.230769230769231,-0.215384615384615,-0.2,-0.184615384615385,-0.169230769230769,
-0.153846153846154,-0.138461538461538,-0.123076923076923,-0.107692307692308,
-0.0923076923076923,-0.0769230769230769,-0.0615384615384615,-0.0461538461538462,
-0.0307692307692308,-0.0153846153846154,0.),(-1.,1.),.UNSPECIFIED.)
GEOMETRIC_REPRESENTATION_ITEM()
RATIONAL_B_SPLINE_SURFACE(((1.,1.),(1.,1.),(1.,1.),(1.,1.),(1.,1.),(1.,
1.),(1.,1.),(1.,1.),(1.,1.),(1.,1.),(1.,1.),(1.,1.),(1.,1.),(1.,1.),(1.,
1.),(1.,1.),(1.,1.),(1.,1.),(1.,1.),(1.,1.),(1.,1.),(1.,1.),(1.,1.),(1.,
1.),(1.,1.),(1.,1.),(1.,1.),(1.,1.),(1.,1.),(1.,1.),(1.,1.),(1.,1.),(1.,
1.),(1.,1.),(1.,1.),(1.,1.),(1.,1.),(1.,1.),(1.,1.),(1.,1.),(1.,1.),(1.,
1.),(1.,1.),(1.,1.),(1.,1.),(1.,1.),(1.,1.),(1.,1.),(1.,1.),(1.,1.),(1.,
1.),(1.,1.),(1.,1.),(1.,1.),(1.,1.),(1.,1.),(1.,1.),(1.,1.),(1.,1.),(1.,
1.),(1.,1.),(1.,1.),(1.,1.),(1.,1.),(1.,1.),(1.,1.),(1.,1.),(1.,1.),(1.,
1.),(1.,1.)))
REPRESENTATION_ITEM('')
SURFACE()
);
#22=(
BOUNDED_SURFACE()
B_SPLINE_SURFACE(5,1,((#27554,#27555),(#27556,#27557),(#27558,#27559),(#27560,
#27561),(#27562,#27563),(#27564,#27565),(#27566,#27567),(#27568,#27569),
(#27570,#27571),(#27572,#27573),(#27574,#27575),(#27576,#27577),(#27578,
#27579),(#27580,#27581),(#27582,#27583),(#27584,#27585),(#27586,#27587),
(#27588,#27589),(#27590,#27591),(#27592,#27593),(#27594,#27595),(#27596,
#27597),(#27598,#27599),(#27600,#27601),(#27602,#27603),(#27604,#27605),
(#27606,#27607),(#27608,#27609),(#27610,#27611),(#27612,#27613),(#27614,
#27615),(#27616,#27617),(#27618,#27619),(#27620,#27621),(#27622,#27623),
(#27624,#27625),(#27626,#27627),(#27628,#27629),(#27630,#27631),(#27632,
#27633),(#27634,#27635),(#27636,#27637),(#27638,#27639),(#27640,#27641),
(#27642,#27643),(#27644,#27645),(#27646,#27647),(#27648,#27649),(#27650,
#27651),(#27652,#27653),(#27654,#27655),(#27656,#27657),(#27658,#27659),
(#27660,#27661),(#27662,#27663),(#27664,#27665),(#27666,#27667),(#27668,
#27669),(#27670,#27671),(#27672,#27673),(#27674,#27675),(#27676,#27677),
(#27678,#27679),(#27680,#27681),(#27682,#27683),(#27684,#27685),(#27686,
#27687),(#27688,#27689),(#27690,#27691),(#27692,#27693)),.UNSPECIFIED.,
 .F.,.F.,.F.)
B_SPLINE_SURFACE_WITH_KNOTS((6,1,1,1,1,1,1,1,1,1,1,1,1,1,1,1,1,1,1,1,1,
1,1,1,1,1,1,1,1,1,1,1,1,1,1,1,1,1,1,1,1,1,1,1,1,1,1,1,1,1,1,1,1,1,1,1,1,
1,1,1,1,1,1,1,1,6),(2,2),(-1.,-0.984615384615383,-0.969230769230768,-0.953846153846152,
-0.938461538461537,-0.923076923076922,-0.907692307692306,-0.892307692307691,
-0.876923076923076,-0.86153846153846,-0.846153846153845,-0.83076923076923,
-0.815384615384614,-0.799999999999999,-0.784615384615384,-0.769230769230768,
-0.753846153846153,-0.738461538461538,-0.723076923076922,-0.707692307692307,
-0.692307692307692,-0.676923076923076,-0.661538461538461,-0.646153846153846,
-0.63076923076923,-0.615384615384615,-0.6,-0.584615384615384,-0.569230769230769,
-0.553846153846154,-0.538461538461538,-0.523076923076923,-0.507692307692308,
-0.492307692307692,-0.476923076923077,-0.461538461538462,-0.446153846153846,
-0.430769230769231,-0.415384615384615,-0.4,-0.384615384615385,-0.369230769230769,
-0.353846153846154,-0.338461538461538,-0.323076923076923,-0.307692307692308,
-0.292307692307692,-0.276923076923077,-0.261538461538462,-0.246153846153846,
-0.230769230769231,-0.215384615384615,-0.2,-0.184615384615385,-0.169230769230769,
-0.153846153846154,-0.138461538461538,-0.123076923076923,-0.107692307692308,
-0.0923076923076923,-0.0769230769230769,-0.0615384615384615,-0.0461538461538462,
-0.0307692307692308,-0.0153846153846154,0.),(-1.,1.),.UNSPECIFIED.)
GEOMETRIC_REPRESENTATION_ITEM()
RATIONAL_B_SPLINE_SURFACE(((1.,1.),(1.,1.),(1.,1.),(1.,1.),(1.,1.),(1.,
1.),(1.,1.),(1.,1.),(1.,1.),(1.,1.),(1.,1.),(1.,1.),(1.,1.),(1.,1.),(1.,
1.),(1.,1.),(1.,1.),(1.,1.),(1.,1.),(1.,1.),(1.,1.),(1.,1.),(1.,1.),(1.,
1.),(1.,1.),(1.,1.),(1.,1.),(1.,1.),(1.,1.),(1.,1.),(1.,1.),(1.,1.),(1.,
1.),(1.,1.),(1.,1.),(1.,1.),(1.,1.),(1.,1.),(1.,1.),(1.,1.),(1.,1.),(1.,
1.),(1.,1.),(1.,1.),(1.,1.),(1.,1.),(1.,1.),(1.,1.),(1.,1.),(1.,1.),(1.,
1.),(1.,1.),(1.,1.),(1.,1.),(1.,1.),(1.,1.),(1.,1.),(1.,1.),(1.,1.),(1.,
1.),(1.,1.),(1.,1.),(1.,1.),(1.,1.),(1.,1.),(1.,1.),(1.,1.),(1.,1.),(1.,
1.),(1.,1.)))
REPRESENTATION_ITEM('')
SURFACE()
);
#23=(
BOUNDED_SURFACE()
B_SPLINE_SURFACE(5,1,((#27770,#27771),(#27772,#27773),(#27774,#27775),(#27776,
#27777),(#27778,#27779),(#27780,#27781),(#27782,#27783),(#27784,#27785),
(#27786,#27787),(#27788,#27789),(#27790,#27791),(#27792,#27793),(#27794,
#27795),(#27796,#27797),(#27798,#27799),(#27800,#27801),(#27802,#27803),
(#27804,#27805),(#27806,#27807),(#27808,#27809),(#27810,#27811),(#27812,
#27813),(#27814,#27815),(#27816,#27817),(#27818,#27819),(#27820,#27821),
(#27822,#27823),(#27824,#27825),(#27826,#27827),(#27828,#27829),(#27830,
#27831),(#27832,#27833),(#27834,#27835),(#27836,#27837),(#27838,#27839),
(#27840,#27841),(#27842,#27843),(#27844,#27845),(#27846,#27847),(#27848,
#27849),(#27850,#27851),(#27852,#27853),(#27854,#27855),(#27856,#27857),
(#27858,#27859),(#27860,#27861),(#27862,#27863),(#27864,#27865),(#27866,
#27867),(#27868,#27869),(#27870,#27871),(#27872,#27873),(#27874,#27875),
(#27876,#27877),(#27878,#27879),(#27880,#27881),(#27882,#27883),(#27884,
#27885),(#27886,#27887),(#27888,#27889),(#27890,#27891),(#27892,#27893),
(#27894,#27895),(#27896,#27897),(#27898,#27899),(#27900,#27901),(#27902,
#27903),(#27904,#27905),(#27906,#27907),(#27908,#27909)),.UNSPECIFIED.,
 .F.,.F.,.F.)
B_SPLINE_SURFACE_WITH_KNOTS((6,1,1,1,1,1,1,1,1,1,1,1,1,1,1,1,1,1,1,1,1,
1,1,1,1,1,1,1,1,1,1,1,1,1,1,1,1,1,1,1,1,1,1,1,1,1,1,1,1,1,1,1,1,1,1,1,1,
1,1,1,1,1,1,1,1,6),(2,2),(-1.,-0.984615384615383,-0.969230769230768,-0.953846153846152,
-0.938461538461537,-0.923076923076922,-0.907692307692306,-0.892307692307691,
-0.876923076923076,-0.86153846153846,-0.846153846153845,-0.83076923076923,
-0.815384615384614,-0.799999999999999,-0.784615384615384,-0.769230769230768,
-0.753846153846153,-0.738461538461538,-0.723076923076922,-0.707692307692307,
-0.692307692307692,-0.676923076923076,-0.661538461538461,-0.646153846153846,
-0.63076923076923,-0.615384615384615,-0.6,-0.584615384615384,-0.569230769230769,
-0.553846153846154,-0.538461538461538,-0.523076923076923,-0.507692307692308,
-0.492307692307692,-0.476923076923077,-0.461538461538462,-0.446153846153846,
-0.430769230769231,-0.415384615384615,-0.4,-0.384615384615385,-0.369230769230769,
-0.353846153846154,-0.338461538461538,-0.323076923076923,-0.307692307692308,
-0.292307692307692,-0.276923076923077,-0.261538461538462,-0.246153846153846,
-0.230769230769231,-0.215384615384615,-0.2,-0.184615384615385,-0.169230769230769,
-0.153846153846154,-0.138461538461538,-0.123076923076923,-0.107692307692308,
-0.0923076923076923,-0.0769230769230769,-0.0615384615384615,-0.0461538461538462,
-0.0307692307692308,-0.0153846153846154,0.),(-1.,1.),.UNSPECIFIED.)
GEOMETRIC_REPRESENTATION_ITEM()
RATIONAL_B_SPLINE_SURFACE(((1.,1.),(1.,1.),(1.,1.),(1.,1.),(1.,1.),(1.,
1.),(1.,1.),(1.,1.),(1.,1.),(1.,1.),(1.,1.),(1.,1.),(1.,1.),(1.,1.),(1.,
1.),(1.,1.),(1.,1.),(1.,1.),(1.,1.),(1.,1.),(1.,1.),(1.,1.),(1.,1.),(1.,
1.),(1.,1.),(1.,1.),(1.,1.),(1.,1.),(1.,1.),(1.,1.),(1.,1.),(1.,1.),(1.,
1.),(1.,1.),(1.,1.),(1.,1.),(1.,1.),(1.,1.),(1.,1.),(1.,1.),(1.,1.),(1.,
1.),(1.,1.),(1.,1.),(1.,1.),(1.,1.),(1.,1.),(1.,1.),(1.,1.),(1.,1.),(1.,
1.),(1.,1.),(1.,1.),(1.,1.),(1.,1.),(1.,1.),(1.,1.),(1.,1.),(1.,1.),(1.,
1.),(1.,1.),(1.,1.),(1.,1.),(1.,1.),(1.,1.),(1.,1.),(1.,1.),(1.,1.),(1.,
1.),(1.,1.)))
REPRESENTATION_ITEM('')
SURFACE()
);
#24=(
BOUNDED_SURFACE()
B_SPLINE_SURFACE(5,1,((#27986,#27987),(#27988,#27989),(#27990,#27991),(#27992,
#27993),(#27994,#27995),(#27996,#27997),(#27998,#27999),(#28000,#28001),
(#28002,#28003),(#28004,#28005),(#28006,#28007),(#28008,#28009),(#28010,
#28011),(#28012,#28013),(#28014,#28015),(#28016,#28017),(#28018,#28019),
(#28020,#28021),(#28022,#28023),(#28024,#28025),(#28026,#28027),(#28028,
#28029),(#28030,#28031),(#28032,#28033),(#28034,#28035),(#28036,#28037),
(#28038,#28039),(#28040,#28041),(#28042,#28043),(#28044,#28045),(#28046,
#28047),(#28048,#28049),(#28050,#28051),(#28052,#28053),(#28054,#28055),
(#28056,#28057),(#28058,#28059),(#28060,#28061),(#28062,#28063),(#28064,
#28065),(#28066,#28067),(#28068,#28069),(#28070,#28071),(#28072,#28073),
(#28074,#28075),(#28076,#28077),(#28078,#28079),(#28080,#28081),(#28082,
#28083),(#28084,#28085),(#28086,#28087),(#28088,#28089),(#28090,#28091),
(#28092,#28093),(#28094,#28095),(#28096,#28097),(#28098,#28099),(#28100,
#28101),(#28102,#28103),(#28104,#28105),(#28106,#28107),(#28108,#28109),
(#28110,#28111),(#28112,#28113),(#28114,#28115),(#28116,#28117),(#28118,
#28119),(#28120,#28121),(#28122,#28123),(#28124,#28125)),.UNSPECIFIED.,
 .F.,.F.,.F.)
B_SPLINE_SURFACE_WITH_KNOTS((6,1,1,1,1,1,1,1,1,1,1,1,1,1,1,1,1,1,1,1,1,
1,1,1,1,1,1,1,1,1,1,1,1,1,1,1,1,1,1,1,1,1,1,1,1,1,1,1,1,1,1,1,1,1,1,1,1,
1,1,1,1,1,1,1,1,6),(2,2),(-1.,-0.984615384615383,-0.969230769230768,-0.953846153846152,
-0.938461538461537,-0.923076923076922,-0.907692307692306,-0.892307692307691,
-0.876923076923076,-0.86153846153846,-0.846153846153845,-0.83076923076923,
-0.815384615384614,-0.799999999999999,-0.784615384615384,-0.769230769230768,
-0.753846153846153,-0.738461538461538,-0.723076923076922,-0.707692307692307,
-0.692307692307692,-0.676923076923076,-0.661538461538461,-0.646153846153846,
-0.63076923076923,-0.615384615384615,-0.6,-0.584615384615384,-0.569230769230769,
-0.553846153846154,-0.538461538461538,-0.523076923076923,-0.507692307692308,
-0.492307692307692,-0.476923076923077,-0.461538461538462,-0.446153846153846,
-0.430769230769231,-0.415384615384615,-0.4,-0.384615384615385,-0.369230769230769,
-0.353846153846154,-0.338461538461538,-0.323076923076923,-0.307692307692308,
-0.292307692307692,-0.276923076923077,-0.261538461538462,-0.246153846153846,
-0.230769230769231,-0.215384615384615,-0.2,-0.184615384615385,-0.169230769230769,
-0.153846153846154,-0.138461538461538,-0.123076923076923,-0.107692307692308,
-0.0923076923076923,-0.0769230769230769,-0.0615384615384615,-0.0461538461538462,
-0.0307692307692308,-0.0153846153846154,0.),(-1.,1.),.UNSPECIFIED.)
GEOMETRIC_REPRESENTATION_ITEM()
RATIONAL_B_SPLINE_SURFACE(((1.,1.),(1.,1.),(1.,1.),(1.,1.),(1.,1.),(1.,
1.),(1.,1.),(1.,1.),(1.,1.),(1.,1.),(1.,1.),(1.,1.),(1.,1.),(1.,1.),(1.,
1.),(1.,1.),(1.,1.),(1.,1.),(1.,1.),(1.,1.),(1.,1.),(1.,1.),(1.,1.),(1.,
1.),(1.,1.),(1.,1.),(1.,1.),(1.,1.),(1.,1.),(1.,1.),(1.,1.),(1.,1.),(1.,
1.),(1.,1.),(1.,1.),(1.,1.),(1.,1.),(1.,1.),(1.,1.),(1.,1.),(1.,1.),(1.,
1.),(1.,1.),(1.,1.),(1.,1.),(1.,1.),(1.,1.),(1.,1.),(1.,1.),(1.,1.),(1.,
1.),(1.,1.),(1.,1.),(1.,1.),(1.,1.),(1.,1.),(1.,1.),(1.,1.),(1.,1.),(1.,
1.),(1.,1.),(1.,1.),(1.,1.),(1.,1.),(1.,1.),(1.,1.),(1.,1.),(1.,1.),(1.,
1.),(1.,1.)))
REPRESENTATION_ITEM('')
SURFACE()
);
#25=(
BOUNDED_SURFACE()
B_SPLINE_SURFACE(5,1,((#28202,#28203),(#28204,#28205),(#28206,#28207),(#28208,
#28209),(#28210,#28211),(#28212,#28213),(#28214,#28215),(#28216,#28217),
(#28218,#28219),(#28220,#28221),(#28222,#28223),(#28224,#28225),(#28226,
#28227),(#28228,#28229),(#28230,#28231),(#28232,#28233),(#28234,#28235),
(#28236,#28237),(#28238,#28239),(#28240,#28241),(#28242,#28243),(#28244,
#28245),(#28246,#28247),(#28248,#28249),(#28250,#28251),(#28252,#28253),
(#28254,#28255),(#28256,#28257),(#28258,#28259),(#28260,#28261),(#28262,
#28263),(#28264,#28265),(#28266,#28267),(#28268,#28269),(#28270,#28271),
(#28272,#28273),(#28274,#28275),(#28276,#28277),(#28278,#28279),(#28280,
#28281),(#28282,#28283),(#28284,#28285),(#28286,#28287),(#28288,#28289),
(#28290,#28291),(#28292,#28293),(#28294,#28295),(#28296,#28297),(#28298,
#28299),(#28300,#28301),(#28302,#28303),(#28304,#28305),(#28306,#28307),
(#28308,#28309),(#28310,#28311),(#28312,#28313),(#28314,#28315),(#28316,
#28317),(#28318,#28319),(#28320,#28321),(#28322,#28323),(#28324,#28325),
(#28326,#28327),(#28328,#28329),(#28330,#28331),(#28332,#28333),(#28334,
#28335),(#28336,#28337),(#28338,#28339),(#28340,#28341)),.UNSPECIFIED.,
 .F.,.F.,.F.)
B_SPLINE_SURFACE_WITH_KNOTS((6,1,1,1,1,1,1,1,1,1,1,1,1,1,1,1,1,1,1,1,1,
1,1,1,1,1,1,1,1,1,1,1,1,1,1,1,1,1,1,1,1,1,1,1,1,1,1,1,1,1,1,1,1,1,1,1,1,
1,1,1,1,1,1,1,1,6),(2,2),(-1.,-0.984615384615383,-0.969230769230768,-0.953846153846152,
-0.938461538461537,-0.923076923076922,-0.907692307692306,-0.892307692307691,
-0.876923076923076,-0.86153846153846,-0.846153846153845,-0.83076923076923,
-0.815384615384614,-0.799999999999999,-0.784615384615384,-0.769230769230768,
-0.753846153846153,-0.738461538461538,-0.723076923076922,-0.707692307692307,
-0.692307692307692,-0.676923076923076,-0.661538461538461,-0.646153846153846,
-0.63076923076923,-0.615384615384615,-0.6,-0.584615384615384,-0.569230769230769,
-0.553846153846154,-0.538461538461538,-0.523076923076923,-0.507692307692308,
-0.492307692307692,-0.476923076923077,-0.461538461538462,-0.446153846153846,
-0.430769230769231,-0.415384615384615,-0.4,-0.384615384615385,-0.369230769230769,
-0.353846153846154,-0.338461538461538,-0.323076923076923,-0.307692307692308,
-0.292307692307692,-0.276923076923077,-0.261538461538462,-0.246153846153846,
-0.230769230769231,-0.215384615384615,-0.2,-0.184615384615385,-0.169230769230769,
-0.153846153846154,-0.138461538461538,-0.123076923076923,-0.107692307692308,
-0.0923076923076923,-0.0769230769230769,-0.0615384615384615,-0.0461538461538462,
-0.0307692307692308,-0.0153846153846154,0.),(-1.,1.),.UNSPECIFIED.)
GEOMETRIC_REPRESENTATION_ITEM()
RATIONAL_B_SPLINE_SURFACE(((1.,1.),(1.,1.),(1.,1.),(1.,1.),(1.,1.),(1.,
1.),(1.,1.),(1.,1.),(1.,1.),(1.,1.),(1.,1.),(1.,1.),(1.,1.),(1.,1.),(1.,
1.),(1.,1.),(1.,1.),(1.,1.),(1.,1.),(1.,1.),(1.,1.),(1.,1.),(1.,1.),(1.,
1.),(1.,1.),(1.,1.),(1.,1.),(1.,1.),(1.,1.),(1.,1.),(1.,1.),(1.,1.),(1.,
1.),(1.,1.),(1.,1.),(1.,1.),(1.,1.),(1.,1.),(1.,1.),(1.,1.),(1.,1.),(1.,
1.),(1.,1.),(1.,1.),(1.,1.),(1.,1.),(1.,1.),(1.,1.),(1.,1.),(1.,1.),(1.,
1.),(1.,1.),(1.,1.),(1.,1.),(1.,1.),(1.,1.),(1.,1.),(1.,1.),(1.,1.),(1.,
1.),(1.,1.),(1.,1.),(1.,1.),(1.,1.),(1.,1.),(1.,1.),(1.,1.),(1.,1.),(1.,
1.),(1.,1.)))
REPRESENTATION_ITEM('')
SURFACE()
);
#26=(
BOUNDED_SURFACE()
B_SPLINE_SURFACE(5,1,((#28418,#28419),(#28420,#28421),(#28422,#28423),(#28424,
#28425),(#28426,#28427),(#28428,#28429),(#28430,#28431),(#28432,#28433),
(#28434,#28435),(#28436,#28437),(#28438,#28439),(#28440,#28441),(#28442,
#28443),(#28444,#28445),(#28446,#28447),(#28448,#28449),(#28450,#28451),
(#28452,#28453),(#28454,#28455),(#28456,#28457),(#28458,#28459),(#28460,
#28461),(#28462,#28463),(#28464,#28465),(#28466,#28467),(#28468,#28469),
(#28470,#28471),(#28472,#28473),(#28474,#28475),(#28476,#28477),(#28478,
#28479),(#28480,#28481),(#28482,#28483),(#28484,#28485),(#28486,#28487),
(#28488,#28489),(#28490,#28491),(#28492,#28493),(#28494,#28495),(#28496,
#28497),(#28498,#28499),(#28500,#28501),(#28502,#28503),(#28504,#28505),
(#28506,#28507),(#28508,#28509),(#28510,#28511),(#28512,#28513),(#28514,
#28515),(#28516,#28517),(#28518,#28519),(#28520,#28521),(#28522,#28523),
(#28524,#28525),(#28526,#28527),(#28528,#28529),(#28530,#28531),(#28532,
#28533),(#28534,#28535),(#28536,#28537),(#28538,#28539),(#28540,#28541),
(#28542,#28543),(#28544,#28545),(#28546,#28547),(#28548,#28549),(#28550,
#28551),(#28552,#28553),(#28554,#28555),(#28556,#28557)),.UNSPECIFIED.,
 .F.,.F.,.F.)
B_SPLINE_SURFACE_WITH_KNOTS((6,1,1,1,1,1,1,1,1,1,1,1,1,1,1,1,1,1,1,1,1,
1,1,1,1,1,1,1,1,1,1,1,1,1,1,1,1,1,1,1,1,1,1,1,1,1,1,1,1,1,1,1,1,1,1,1,1,
1,1,1,1,1,1,1,1,6),(2,2),(-1.,-0.984615384615383,-0.969230769230768,-0.953846153846152,
-0.938461538461537,-0.923076923076922,-0.907692307692306,-0.892307692307691,
-0.876923076923076,-0.86153846153846,-0.846153846153845,-0.83076923076923,
-0.815384615384614,-0.799999999999999,-0.784615384615384,-0.769230769230768,
-0.753846153846153,-0.738461538461538,-0.723076923076922,-0.707692307692307,
-0.692307692307692,-0.676923076923076,-0.661538461538461,-0.646153846153846,
-0.63076923076923,-0.615384615384615,-0.6,-0.584615384615384,-0.569230769230769,
-0.553846153846154,-0.538461538461538,-0.523076923076923,-0.507692307692308,
-0.492307692307692,-0.476923076923077,-0.461538461538462,-0.446153846153846,
-0.430769230769231,-0.415384615384615,-0.4,-0.384615384615385,-0.369230769230769,
-0.353846153846154,-0.338461538461538,-0.323076923076923,-0.307692307692308,
-0.292307692307692,-0.276923076923077,-0.261538461538462,-0.246153846153846,
-0.230769230769231,-0.215384615384615,-0.2,-0.184615384615385,-0.169230769230769,
-0.153846153846154,-0.138461538461538,-0.123076923076923,-0.107692307692308,
-0.0923076923076923,-0.0769230769230769,-0.0615384615384615,-0.0461538461538462,
-0.0307692307692308,-0.0153846153846154,0.),(-1.,1.),.UNSPECIFIED.)
GEOMETRIC_REPRESENTATION_ITEM()
RATIONAL_B_SPLINE_SURFACE(((1.,1.),(1.,1.),(1.,1.),(1.,1.),(1.,1.),(1.,
1.),(1.,1.),(1.,1.),(1.,1.),(1.,1.),(1.,1.),(1.,1.),(1.,1.),(1.,1.),(1.,
1.),(1.,1.),(1.,1.),(1.,1.),(1.,1.),(1.,1.),(1.,1.),(1.,1.),(1.,1.),(1.,
1.),(1.,1.),(1.,1.),(1.,1.),(1.,1.),(1.,1.),(1.,1.),(1.,1.),(1.,1.),(1.,
1.),(1.,1.),(1.,1.),(1.,1.),(1.,1.),(1.,1.),(1.,1.),(1.,1.),(1.,1.),(1.,
1.),(1.,1.),(1.,1.),(1.,1.),(1.,1.),(1.,1.),(1.,1.),(1.,1.),(1.,1.),(1.,
1.),(1.,1.),(1.,1.),(1.,1.),(1.,1.),(1.,1.),(1.,1.),(1.,1.),(1.,1.),(1.,
1.),(1.,1.),(1.,1.),(1.,1.),(1.,1.),(1.,1.),(1.,1.),(1.,1.),(1.,1.),(1.,
1.),(1.,1.)))
REPRESENTATION_ITEM('')
SURFACE()
);
#27=(
BOUNDED_SURFACE()
B_SPLINE_SURFACE(5,1,((#28634,#28635),(#28636,#28637),(#28638,#28639),(#28640,
#28641),(#28642,#28643),(#28644,#28645),(#28646,#28647),(#28648,#28649),
(#28650,#28651),(#28652,#28653),(#28654,#28655),(#28656,#28657),(#28658,
#28659),(#28660,#28661),(#28662,#28663),(#28664,#28665),(#28666,#28667),
(#28668,#28669),(#28670,#28671),(#28672,#28673),(#28674,#28675),(#28676,
#28677),(#28678,#28679),(#28680,#28681),(#28682,#28683),(#28684,#28685),
(#28686,#28687),(#28688,#28689),(#28690,#28691),(#28692,#28693),(#28694,
#28695),(#28696,#28697),(#28698,#28699),(#28700,#28701),(#28702,#28703),
(#28704,#28705),(#28706,#28707),(#28708,#28709),(#28710,#28711),(#28712,
#28713),(#28714,#28715),(#28716,#28717),(#28718,#28719),(#28720,#28721),
(#28722,#28723),(#28724,#28725),(#28726,#28727),(#28728,#28729),(#28730,
#28731),(#28732,#28733),(#28734,#28735),(#28736,#28737),(#28738,#28739),
(#28740,#28741),(#28742,#28743),(#28744,#28745),(#28746,#28747),(#28748,
#28749),(#28750,#28751),(#28752,#28753),(#28754,#28755),(#28756,#28757),
(#28758,#28759),(#28760,#28761),(#28762,#28763),(#28764,#28765),(#28766,
#28767),(#28768,#28769),(#28770,#28771),(#28772,#28773)),.UNSPECIFIED.,
 .F.,.F.,.F.)
B_SPLINE_SURFACE_WITH_KNOTS((6,1,1,1,1,1,1,1,1,1,1,1,1,1,1,1,1,1,1,1,1,
1,1,1,1,1,1,1,1,1,1,1,1,1,1,1,1,1,1,1,1,1,1,1,1,1,1,1,1,1,1,1,1,1,1,1,1,
1,1,1,1,1,1,1,1,6),(2,2),(-1.,-0.984615384615383,-0.969230769230768,-0.953846153846152,
-0.938461538461537,-0.923076923076922,-0.907692307692306,-0.892307692307691,
-0.876923076923076,-0.86153846153846,-0.846153846153845,-0.83076923076923,
-0.815384615384614,-0.799999999999999,-0.784615384615384,-0.769230769230768,
-0.753846153846153,-0.738461538461538,-0.723076923076922,-0.707692307692307,
-0.692307692307692,-0.676923076923076,-0.661538461538461,-0.646153846153846,
-0.63076923076923,-0.615384615384615,-0.6,-0.584615384615384,-0.569230769230769,
-0.553846153846154,-0.538461538461538,-0.523076923076923,-0.507692307692308,
-0.492307692307692,-0.476923076923077,-0.461538461538462,-0.446153846153846,
-0.430769230769231,-0.415384615384615,-0.4,-0.384615384615385,-0.369230769230769,
-0.353846153846154,-0.338461538461538,-0.323076923076923,-0.307692307692308,
-0.292307692307692,-0.276923076923077,-0.261538461538462,-0.246153846153846,
-0.230769230769231,-0.215384615384615,-0.2,-0.184615384615385,-0.169230769230769,
-0.153846153846154,-0.138461538461538,-0.123076923076923,-0.107692307692308,
-0.0923076923076923,-0.0769230769230769,-0.0615384615384615,-0.0461538461538462,
-0.0307692307692308,-0.0153846153846154,0.),(-1.,1.),.UNSPECIFIED.)
GEOMETRIC_REPRESENTATION_ITEM()
RATIONAL_B_SPLINE_SURFACE(((1.,1.),(1.,1.),(1.,1.),(1.,1.),(1.,1.),(1.,
1.),(1.,1.),(1.,1.),(1.,1.),(1.,1.),(1.,1.),(1.,1.),(1.,1.),(1.,1.),(1.,
1.),(1.,1.),(1.,1.),(1.,1.),(1.,1.),(1.,1.),(1.,1.),(1.,1.),(1.,1.),(1.,
1.),(1.,1.),(1.,1.),(1.,1.),(1.,1.),(1.,1.),(1.,1.),(1.,1.),(1.,1.),(1.,
1.),(1.,1.),(1.,1.),(1.,1.),(1.,1.),(1.,1.),(1.,1.),(1.,1.),(1.,1.),(1.,
1.),(1.,1.),(1.,1.),(1.,1.),(1.,1.),(1.,1.),(1.,1.),(1.,1.),(1.,1.),(1.,
1.),(1.,1.),(1.,1.),(1.,1.),(1.,1.),(1.,1.),(1.,1.),(1.,1.),(1.,1.),(1.,
1.),(1.,1.),(1.,1.),(1.,1.),(1.,1.),(1.,1.),(1.,1.),(1.,1.),(1.,1.),(1.,
1.),(1.,1.)))
REPRESENTATION_ITEM('')
SURFACE()
);
#28=(
BOUNDED_SURFACE()
B_SPLINE_SURFACE(5,1,((#28850,#28851),(#28852,#28853),(#28854,#28855),(#28856,
#28857),(#28858,#28859),(#28860,#28861),(#28862,#28863),(#28864,#28865),
(#28866,#28867),(#28868,#28869),(#28870,#28871),(#28872,#28873),(#28874,
#28875),(#28876,#28877),(#28878,#28879),(#28880,#28881),(#28882,#28883),
(#28884,#28885),(#28886,#28887),(#28888,#28889),(#28890,#28891),(#28892,
#28893),(#28894,#28895),(#28896,#28897),(#28898,#28899),(#28900,#28901),
(#28902,#28903),(#28904,#28905),(#28906,#28907),(#28908,#28909),(#28910,
#28911),(#28912,#28913),(#28914,#28915),(#28916,#28917),(#28918,#28919),
(#28920,#28921),(#28922,#28923),(#28924,#28925),(#28926,#28927),(#28928,
#28929),(#28930,#28931),(#28932,#28933),(#28934,#28935),(#28936,#28937),
(#28938,#28939),(#28940,#28941),(#28942,#28943),(#28944,#28945),(#28946,
#28947),(#28948,#28949),(#28950,#28951),(#28952,#28953),(#28954,#28955),
(#28956,#28957),(#28958,#28959),(#28960,#28961),(#28962,#28963),(#28964,
#28965),(#28966,#28967),(#28968,#28969),(#28970,#28971),(#28972,#28973),
(#28974,#28975),(#28976,#28977),(#28978,#28979),(#28980,#28981),(#28982,
#28983),(#28984,#28985),(#28986,#28987),(#28988,#28989)),.UNSPECIFIED.,
 .F.,.F.,.F.)
B_SPLINE_SURFACE_WITH_KNOTS((6,1,1,1,1,1,1,1,1,1,1,1,1,1,1,1,1,1,1,1,1,
1,1,1,1,1,1,1,1,1,1,1,1,1,1,1,1,1,1,1,1,1,1,1,1,1,1,1,1,1,1,1,1,1,1,1,1,
1,1,1,1,1,1,1,1,6),(2,2),(-1.,-0.984615384615383,-0.969230769230768,-0.953846153846152,
-0.938461538461537,-0.923076923076922,-0.907692307692306,-0.892307692307691,
-0.876923076923076,-0.86153846153846,-0.846153846153845,-0.83076923076923,
-0.815384615384614,-0.799999999999999,-0.784615384615384,-0.769230769230768,
-0.753846153846153,-0.738461538461538,-0.723076923076922,-0.707692307692307,
-0.692307692307692,-0.676923076923076,-0.661538461538461,-0.646153846153846,
-0.63076923076923,-0.615384615384615,-0.6,-0.584615384615384,-0.569230769230769,
-0.553846153846154,-0.538461538461538,-0.523076923076923,-0.507692307692308,
-0.492307692307692,-0.476923076923077,-0.461538461538462,-0.446153846153846,
-0.430769230769231,-0.415384615384615,-0.4,-0.384615384615385,-0.369230769230769,
-0.353846153846154,-0.338461538461538,-0.323076923076923,-0.307692307692308,
-0.292307692307692,-0.276923076923077,-0.261538461538462,-0.246153846153846,
-0.230769230769231,-0.215384615384615,-0.2,-0.184615384615385,-0.169230769230769,
-0.153846153846154,-0.138461538461538,-0.123076923076923,-0.107692307692308,
-0.0923076923076923,-0.0769230769230769,-0.0615384615384615,-0.0461538461538462,
-0.0307692307692308,-0.0153846153846154,0.),(-1.,1.),.UNSPECIFIED.)
GEOMETRIC_REPRESENTATION_ITEM()
RATIONAL_B_SPLINE_SURFACE(((1.,1.),(1.,1.),(1.,1.),(1.,1.),(1.,1.),(1.,
1.),(1.,1.),(1.,1.),(1.,1.),(1.,1.),(1.,1.),(1.,1.),(1.,1.),(1.,1.),(1.,
1.),(1.,1.),(1.,1.),(1.,1.),(1.,1.),(1.,1.),(1.,1.),(1.,1.),(1.,1.),(1.,
1.),(1.,1.),(1.,1.),(1.,1.),(1.,1.),(1.,1.),(1.,1.),(1.,1.),(1.,1.),(1.,
1.),(1.,1.),(1.,1.),(1.,1.),(1.,1.),(1.,1.),(1.,1.),(1.,1.),(1.,1.),(1.,
1.),(1.,1.),(1.,1.),(1.,1.),(1.,1.),(1.,1.),(1.,1.),(1.,1.),(1.,1.),(1.,
1.),(1.,1.),(1.,1.),(1.,1.),(1.,1.),(1.,1.),(1.,1.),(1.,1.),(1.,1.),(1.,
1.),(1.,1.),(1.,1.),(1.,1.),(1.,1.),(1.,1.),(1.,1.),(1.,1.),(1.,1.),(1.,
1.),(1.,1.)))
REPRESENTATION_ITEM('')
SURFACE()
);
#29=(
BOUNDED_SURFACE()
B_SPLINE_SURFACE(5,1,((#29066,#29067),(#29068,#29069),(#29070,#29071),(#29072,
#29073),(#29074,#29075),(#29076,#29077),(#29078,#29079),(#29080,#29081),
(#29082,#29083),(#29084,#29085),(#29086,#29087),(#29088,#29089),(#29090,
#29091),(#29092,#29093),(#29094,#29095),(#29096,#29097),(#29098,#29099),
(#29100,#29101),(#29102,#29103),(#29104,#29105),(#29106,#29107),(#29108,
#29109),(#29110,#29111),(#29112,#29113),(#29114,#29115),(#29116,#29117),
(#29118,#29119),(#29120,#29121),(#29122,#29123),(#29124,#29125),(#29126,
#29127),(#29128,#29129),(#29130,#29131),(#29132,#29133),(#29134,#29135),
(#29136,#29137),(#29138,#29139),(#29140,#29141),(#29142,#29143),(#29144,
#29145),(#29146,#29147),(#29148,#29149),(#29150,#29151),(#29152,#29153),
(#29154,#29155),(#29156,#29157),(#29158,#29159),(#29160,#29161),(#29162,
#29163),(#29164,#29165),(#29166,#29167),(#29168,#29169),(#29170,#29171),
(#29172,#29173),(#29174,#29175),(#29176,#29177),(#29178,#29179),(#29180,
#29181),(#29182,#29183),(#29184,#29185),(#29186,#29187),(#29188,#29189),
(#29190,#29191),(#29192,#29193),(#29194,#29195),(#29196,#29197),(#29198,
#29199),(#29200,#29201),(#29202,#29203),(#29204,#29205)),.UNSPECIFIED.,
 .F.,.F.,.F.)
B_SPLINE_SURFACE_WITH_KNOTS((6,1,1,1,1,1,1,1,1,1,1,1,1,1,1,1,1,1,1,1,1,
1,1,1,1,1,1,1,1,1,1,1,1,1,1,1,1,1,1,1,1,1,1,1,1,1,1,1,1,1,1,1,1,1,1,1,1,
1,1,1,1,1,1,1,1,6),(2,2),(-1.,-0.984615384615383,-0.969230769230768,-0.953846153846152,
-0.938461538461537,-0.923076923076922,-0.907692307692306,-0.892307692307691,
-0.876923076923076,-0.86153846153846,-0.846153846153845,-0.83076923076923,
-0.815384615384614,-0.799999999999999,-0.784615384615384,-0.769230769230768,
-0.753846153846153,-0.738461538461538,-0.723076923076922,-0.707692307692307,
-0.692307692307692,-0.676923076923076,-0.661538461538461,-0.646153846153846,
-0.63076923076923,-0.615384615384615,-0.6,-0.584615384615384,-0.569230769230769,
-0.553846153846154,-0.538461538461538,-0.523076923076923,-0.507692307692308,
-0.492307692307692,-0.476923076923077,-0.461538461538462,-0.446153846153846,
-0.430769230769231,-0.415384615384615,-0.4,-0.384615384615385,-0.369230769230769,
-0.353846153846154,-0.338461538461538,-0.323076923076923,-0.307692307692308,
-0.292307692307692,-0.276923076923077,-0.261538461538462,-0.246153846153846,
-0.230769230769231,-0.215384615384615,-0.2,-0.184615384615385,-0.169230769230769,
-0.153846153846154,-0.138461538461538,-0.123076923076923,-0.107692307692308,
-0.0923076923076923,-0.0769230769230769,-0.0615384615384615,-0.0461538461538462,
-0.0307692307692308,-0.0153846153846154,0.),(-1.,1.),.UNSPECIFIED.)
GEOMETRIC_REPRESENTATION_ITEM()
RATIONAL_B_SPLINE_SURFACE(((1.,1.),(1.,1.),(1.,1.),(1.,1.),(1.,1.),(1.,
1.),(1.,1.),(1.,1.),(1.,1.),(1.,1.),(1.,1.),(1.,1.),(1.,1.),(1.,1.),(1.,
1.),(1.,1.),(1.,1.),(1.,1.),(1.,1.),(1.,1.),(1.,1.),(1.,1.),(1.,1.),(1.,
1.),(1.,1.),(1.,1.),(1.,1.),(1.,1.),(1.,1.),(1.,1.),(1.,1.),(1.,1.),(1.,
1.),(1.,1.),(1.,1.),(1.,1.),(1.,1.),(1.,1.),(1.,1.),(1.,1.),(1.,1.),(1.,
1.),(1.,1.),(1.,1.),(1.,1.),(1.,1.),(1.,1.),(1.,1.),(1.,1.),(1.,1.),(1.,
1.),(1.,1.),(1.,1.),(1.,1.),(1.,1.),(1.,1.),(1.,1.),(1.,1.),(1.,1.),(1.,
1.),(1.,1.),(1.,1.),(1.,1.),(1.,1.),(1.,1.),(1.,1.),(1.,1.),(1.,1.),(1.,
1.),(1.,1.)))
REPRESENTATION_ITEM('')
SURFACE()
);
#30=(
BOUNDED_SURFACE()
B_SPLINE_SURFACE(5,1,((#29282,#29283),(#29284,#29285),(#29286,#29287),(#29288,
#29289),(#29290,#29291),(#29292,#29293),(#29294,#29295),(#29296,#29297),
(#29298,#29299),(#29300,#29301),(#29302,#29303),(#29304,#29305),(#29306,
#29307),(#29308,#29309),(#29310,#29311),(#29312,#29313),(#29314,#29315),
(#29316,#29317),(#29318,#29319),(#29320,#29321),(#29322,#29323),(#29324,
#29325),(#29326,#29327),(#29328,#29329),(#29330,#29331),(#29332,#29333),
(#29334,#29335),(#29336,#29337),(#29338,#29339),(#29340,#29341),(#29342,
#29343),(#29344,#29345),(#29346,#29347),(#29348,#29349),(#29350,#29351),
(#29352,#29353),(#29354,#29355),(#29356,#29357),(#29358,#29359),(#29360,
#29361),(#29362,#29363),(#29364,#29365),(#29366,#29367),(#29368,#29369),
(#29370,#29371),(#29372,#29373),(#29374,#29375),(#29376,#29377),(#29378,
#29379),(#29380,#29381),(#29382,#29383),(#29384,#29385),(#29386,#29387),
(#29388,#29389),(#29390,#29391),(#29392,#29393),(#29394,#29395),(#29396,
#29397),(#29398,#29399),(#29400,#29401),(#29402,#29403),(#29404,#29405),
(#29406,#29407),(#29408,#29409),(#29410,#29411),(#29412,#29413),(#29414,
#29415),(#29416,#29417),(#29418,#29419),(#29420,#29421)),.UNSPECIFIED.,
 .F.,.F.,.F.)
B_SPLINE_SURFACE_WITH_KNOTS((6,1,1,1,1,1,1,1,1,1,1,1,1,1,1,1,1,1,1,1,1,
1,1,1,1,1,1,1,1,1,1,1,1,1,1,1,1,1,1,1,1,1,1,1,1,1,1,1,1,1,1,1,1,1,1,1,1,
1,1,1,1,1,1,1,1,6),(2,2),(-1.,-0.984615384615383,-0.969230769230768,-0.953846153846152,
-0.938461538461537,-0.923076923076922,-0.907692307692306,-0.892307692307691,
-0.876923076923076,-0.86153846153846,-0.846153846153845,-0.83076923076923,
-0.815384615384614,-0.799999999999999,-0.784615384615384,-0.769230769230768,
-0.753846153846153,-0.738461538461538,-0.723076923076922,-0.707692307692307,
-0.692307692307692,-0.676923076923076,-0.661538461538461,-0.646153846153846,
-0.63076923076923,-0.615384615384615,-0.6,-0.584615384615384,-0.569230769230769,
-0.553846153846154,-0.538461538461538,-0.523076923076923,-0.507692307692308,
-0.492307692307692,-0.476923076923077,-0.461538461538462,-0.446153846153846,
-0.430769230769231,-0.415384615384615,-0.4,-0.384615384615385,-0.369230769230769,
-0.353846153846154,-0.338461538461538,-0.323076923076923,-0.307692307692308,
-0.292307692307692,-0.276923076923077,-0.261538461538462,-0.246153846153846,
-0.230769230769231,-0.215384615384615,-0.2,-0.184615384615385,-0.169230769230769,
-0.153846153846154,-0.138461538461538,-0.123076923076923,-0.107692307692308,
-0.0923076923076923,-0.0769230769230769,-0.0615384615384615,-0.0461538461538462,
-0.0307692307692308,-0.0153846153846154,0.),(-1.,1.),.UNSPECIFIED.)
GEOMETRIC_REPRESENTATION_ITEM()
RATIONAL_B_SPLINE_SURFACE(((1.,1.),(1.,1.),(1.,1.),(1.,1.),(1.,1.),(1.,
1.),(1.,1.),(1.,1.),(1.,1.),(1.,1.),(1.,1.),(1.,1.),(1.,1.),(1.,1.),(1.,
1.),(1.,1.),(1.,1.),(1.,1.),(1.,1.),(1.,1.),(1.,1.),(1.,1.),(1.,1.),(1.,
1.),(1.,1.),(1.,1.),(1.,1.),(1.,1.),(1.,1.),(1.,1.),(1.,1.),(1.,1.),(1.,
1.),(1.,1.),(1.,1.),(1.,1.),(1.,1.),(1.,1.),(1.,1.),(1.,1.),(1.,1.),(1.,
1.),(1.,1.),(1.,1.),(1.,1.),(1.,1.),(1.,1.),(1.,1.),(1.,1.),(1.,1.),(1.,
1.),(1.,1.),(1.,1.),(1.,1.),(1.,1.),(1.,1.),(1.,1.),(1.,1.),(1.,1.),(1.,
1.),(1.,1.),(1.,1.),(1.,1.),(1.,1.),(1.,1.),(1.,1.),(1.,1.),(1.,1.),(1.,
1.),(1.,1.)))
REPRESENTATION_ITEM('')
SURFACE()
);
#31=(
BOUNDED_SURFACE()
B_SPLINE_SURFACE(5,1,((#29498,#29499),(#29500,#29501),(#29502,#29503),(#29504,
#29505),(#29506,#29507),(#29508,#29509),(#29510,#29511),(#29512,#29513),
(#29514,#29515),(#29516,#29517),(#29518,#29519),(#29520,#29521),(#29522,
#29523),(#29524,#29525),(#29526,#29527),(#29528,#29529),(#29530,#29531),
(#29532,#29533),(#29534,#29535),(#29536,#29537),(#29538,#29539),(#29540,
#29541),(#29542,#29543),(#29544,#29545),(#29546,#29547),(#29548,#29549),
(#29550,#29551),(#29552,#29553),(#29554,#29555),(#29556,#29557),(#29558,
#29559),(#29560,#29561),(#29562,#29563),(#29564,#29565),(#29566,#29567),
(#29568,#29569),(#29570,#29571),(#29572,#29573),(#29574,#29575),(#29576,
#29577),(#29578,#29579),(#29580,#29581),(#29582,#29583),(#29584,#29585),
(#29586,#29587),(#29588,#29589),(#29590,#29591),(#29592,#29593),(#29594,
#29595),(#29596,#29597),(#29598,#29599),(#29600,#29601),(#29602,#29603),
(#29604,#29605),(#29606,#29607),(#29608,#29609),(#29610,#29611),(#29612,
#29613),(#29614,#29615),(#29616,#29617),(#29618,#29619),(#29620,#29621),
(#29622,#29623),(#29624,#29625),(#29626,#29627),(#29628,#29629),(#29630,
#29631),(#29632,#29633),(#29634,#29635),(#29636,#29637)),.UNSPECIFIED.,
 .F.,.F.,.F.)
B_SPLINE_SURFACE_WITH_KNOTS((6,1,1,1,1,1,1,1,1,1,1,1,1,1,1,1,1,1,1,1,1,
1,1,1,1,1,1,1,1,1,1,1,1,1,1,1,1,1,1,1,1,1,1,1,1,1,1,1,1,1,1,1,1,1,1,1,1,
1,1,1,1,1,1,1,1,6),(2,2),(-1.,-0.984615384615383,-0.969230769230768,-0.953846153846152,
-0.938461538461537,-0.923076923076922,-0.907692307692306,-0.892307692307691,
-0.876923076923076,-0.86153846153846,-0.846153846153845,-0.83076923076923,
-0.815384615384614,-0.799999999999999,-0.784615384615384,-0.769230769230768,
-0.753846153846153,-0.738461538461538,-0.723076923076922,-0.707692307692307,
-0.692307692307692,-0.676923076923076,-0.661538461538461,-0.646153846153846,
-0.63076923076923,-0.615384615384615,-0.6,-0.584615384615384,-0.569230769230769,
-0.553846153846154,-0.538461538461538,-0.523076923076923,-0.507692307692308,
-0.492307692307692,-0.476923076923077,-0.461538461538462,-0.446153846153846,
-0.430769230769231,-0.415384615384615,-0.4,-0.384615384615385,-0.369230769230769,
-0.353846153846154,-0.338461538461538,-0.323076923076923,-0.307692307692308,
-0.292307692307692,-0.276923076923077,-0.261538461538462,-0.246153846153846,
-0.230769230769231,-0.215384615384615,-0.2,-0.184615384615385,-0.169230769230769,
-0.153846153846154,-0.138461538461538,-0.123076923076923,-0.107692307692308,
-0.0923076923076923,-0.0769230769230769,-0.0615384615384615,-0.0461538461538462,
-0.0307692307692308,-0.0153846153846154,0.),(-1.,1.),.UNSPECIFIED.)
GEOMETRIC_REPRESENTATION_ITEM()
RATIONAL_B_SPLINE_SURFACE(((1.,1.),(1.,1.),(1.,1.),(1.,1.),(1.,1.),(1.,
1.),(1.,1.),(1.,1.),(1.,1.),(1.,1.),(1.,1.),(1.,1.),(1.,1.),(1.,1.),(1.,
1.),(1.,1.),(1.,1.),(1.,1.),(1.,1.),(1.,1.),(1.,1.),(1.,1.),(1.,1.),(1.,
1.),(1.,1.),(1.,1.),(1.,1.),(1.,1.),(1.,1.),(1.,1.),(1.,1.),(1.,1.),(1.,
1.),(1.,1.),(1.,1.),(1.,1.),(1.,1.),(1.,1.),(1.,1.),(1.,1.),(1.,1.),(1.,
1.),(1.,1.),(1.,1.),(1.,1.),(1.,1.),(1.,1.),(1.,1.),(1.,1.),(1.,1.),(1.,
1.),(1.,1.),(1.,1.),(1.,1.),(1.,1.),(1.,1.),(1.,1.),(1.,1.),(1.,1.),(1.,
1.),(1.,1.),(1.,1.),(1.,1.),(1.,1.),(1.,1.),(1.,1.),(1.,1.),(1.,1.),(1.,
1.),(1.,1.)))
REPRESENTATION_ITEM('')
SURFACE()
);
#32=(
BOUNDED_SURFACE()
B_SPLINE_SURFACE(5,1,((#29714,#29715),(#29716,#29717),(#29718,#29719),(#29720,
#29721),(#29722,#29723),(#29724,#29725),(#29726,#29727),(#29728,#29729),
(#29730,#29731),(#29732,#29733),(#29734,#29735),(#29736,#29737),(#29738,
#29739),(#29740,#29741),(#29742,#29743),(#29744,#29745),(#29746,#29747),
(#29748,#29749),(#29750,#29751),(#29752,#29753),(#29754,#29755),(#29756,
#29757),(#29758,#29759),(#29760,#29761),(#29762,#29763),(#29764,#29765),
(#29766,#29767),(#29768,#29769),(#29770,#29771),(#29772,#29773),(#29774,
#29775),(#29776,#29777),(#29778,#29779),(#29780,#29781),(#29782,#29783),
(#29784,#29785),(#29786,#29787),(#29788,#29789),(#29790,#29791),(#29792,
#29793),(#29794,#29795),(#29796,#29797),(#29798,#29799),(#29800,#29801),
(#29802,#29803),(#29804,#29805),(#29806,#29807),(#29808,#29809),(#29810,
#29811),(#29812,#29813),(#29814,#29815),(#29816,#29817),(#29818,#29819),
(#29820,#29821),(#29822,#29823),(#29824,#29825),(#29826,#29827),(#29828,
#29829),(#29830,#29831),(#29832,#29833),(#29834,#29835),(#29836,#29837),
(#29838,#29839),(#29840,#29841),(#29842,#29843),(#29844,#29845),(#29846,
#29847),(#29848,#29849),(#29850,#29851),(#29852,#29853)),.UNSPECIFIED.,
 .F.,.F.,.F.)
B_SPLINE_SURFACE_WITH_KNOTS((6,1,1,1,1,1,1,1,1,1,1,1,1,1,1,1,1,1,1,1,1,
1,1,1,1,1,1,1,1,1,1,1,1,1,1,1,1,1,1,1,1,1,1,1,1,1,1,1,1,1,1,1,1,1,1,1,1,
1,1,1,1,1,1,1,1,6),(2,2),(-1.,-0.984615384615383,-0.969230769230768,-0.953846153846152,
-0.938461538461537,-0.923076923076922,-0.907692307692306,-0.892307692307691,
-0.876923076923076,-0.86153846153846,-0.846153846153845,-0.83076923076923,
-0.815384615384614,-0.799999999999999,-0.784615384615384,-0.769230769230768,
-0.753846153846153,-0.738461538461538,-0.723076923076922,-0.707692307692307,
-0.692307692307692,-0.676923076923076,-0.661538461538461,-0.646153846153846,
-0.63076923076923,-0.615384615384615,-0.6,-0.584615384615384,-0.569230769230769,
-0.553846153846154,-0.538461538461538,-0.523076923076923,-0.507692307692308,
-0.492307692307692,-0.476923076923077,-0.461538461538462,-0.446153846153846,
-0.430769230769231,-0.415384615384615,-0.4,-0.384615384615385,-0.369230769230769,
-0.353846153846154,-0.338461538461538,-0.323076923076923,-0.307692307692308,
-0.292307692307692,-0.276923076923077,-0.261538461538462,-0.246153846153846,
-0.230769230769231,-0.215384615384615,-0.2,-0.184615384615385,-0.169230769230769,
-0.153846153846154,-0.138461538461538,-0.123076923076923,-0.107692307692308,
-0.0923076923076923,-0.0769230769230769,-0.0615384615384615,-0.0461538461538462,
-0.0307692307692308,-0.0153846153846154,0.),(-1.,1.),.UNSPECIFIED.)
GEOMETRIC_REPRESENTATION_ITEM()
RATIONAL_B_SPLINE_SURFACE(((1.,1.),(1.,1.),(1.,1.),(1.,1.),(1.,1.),(1.,
1.),(1.,1.),(1.,1.),(1.,1.),(1.,1.),(1.,1.),(1.,1.),(1.,1.),(1.,1.),(1.,
1.),(1.,1.),(1.,1.),(1.,1.),(1.,1.),(1.,1.),(1.,1.),(1.,1.),(1.,1.),(1.,
1.),(1.,1.),(1.,1.),(1.,1.),(1.,1.),(1.,1.),(1.,1.),(1.,1.),(1.,1.),(1.,
1.),(1.,1.),(1.,1.),(1.,1.),(1.,1.),(1.,1.),(1.,1.),(1.,1.),(1.,1.),(1.,
1.),(1.,1.),(1.,1.),(1.,1.),(1.,1.),(1.,1.),(1.,1.),(1.,1.),(1.,1.),(1.,
1.),(1.,1.),(1.,1.),(1.,1.),(1.,1.),(1.,1.),(1.,1.),(1.,1.),(1.,1.),(1.,
1.),(1.,1.),(1.,1.),(1.,1.),(1.,1.),(1.,1.),(1.,1.),(1.,1.),(1.,1.),(1.,
1.),(1.,1.)))
REPRESENTATION_ITEM('')
SURFACE()
);
#33=(
BOUNDED_SURFACE()
B_SPLINE_SURFACE(5,1,((#29930,#29931),(#29932,#29933),(#29934,#29935),(#29936,
#29937),(#29938,#29939),(#29940,#29941),(#29942,#29943),(#29944,#29945),
(#29946,#29947),(#29948,#29949),(#29950,#29951),(#29952,#29953),(#29954,
#29955),(#29956,#29957),(#29958,#29959),(#29960,#29961),(#29962,#29963),
(#29964,#29965),(#29966,#29967),(#29968,#29969),(#29970,#29971),(#29972,
#29973),(#29974,#29975),(#29976,#29977),(#29978,#29979),(#29980,#29981),
(#29982,#29983),(#29984,#29985),(#29986,#29987),(#29988,#29989),(#29990,
#29991),(#29992,#29993),(#29994,#29995),(#29996,#29997),(#29998,#29999),
(#30000,#30001),(#30002,#30003),(#30004,#30005),(#30006,#30007),(#30008,
#30009),(#30010,#30011),(#30012,#30013),(#30014,#30015),(#30016,#30017),
(#30018,#30019),(#30020,#30021),(#30022,#30023),(#30024,#30025),(#30026,
#30027),(#30028,#30029),(#30030,#30031),(#30032,#30033),(#30034,#30035),
(#30036,#30037),(#30038,#30039),(#30040,#30041),(#30042,#30043),(#30044,
#30045),(#30046,#30047),(#30048,#30049),(#30050,#30051),(#30052,#30053),
(#30054,#30055),(#30056,#30057),(#30058,#30059),(#30060,#30061),(#30062,
#30063),(#30064,#30065),(#30066,#30067),(#30068,#30069)),.UNSPECIFIED.,
 .F.,.F.,.F.)
B_SPLINE_SURFACE_WITH_KNOTS((6,1,1,1,1,1,1,1,1,1,1,1,1,1,1,1,1,1,1,1,1,
1,1,1,1,1,1,1,1,1,1,1,1,1,1,1,1,1,1,1,1,1,1,1,1,1,1,1,1,1,1,1,1,1,1,1,1,
1,1,1,1,1,1,1,1,6),(2,2),(-1.,-0.984615384615383,-0.969230769230768,-0.953846153846152,
-0.938461538461537,-0.923076923076922,-0.907692307692306,-0.892307692307691,
-0.876923076923076,-0.86153846153846,-0.846153846153845,-0.83076923076923,
-0.815384615384614,-0.799999999999999,-0.784615384615384,-0.769230769230768,
-0.753846153846153,-0.738461538461538,-0.723076923076922,-0.707692307692307,
-0.692307692307692,-0.676923076923076,-0.661538461538461,-0.646153846153846,
-0.63076923076923,-0.615384615384615,-0.6,-0.584615384615384,-0.569230769230769,
-0.553846153846154,-0.538461538461538,-0.523076923076923,-0.507692307692308,
-0.492307692307692,-0.476923076923077,-0.461538461538462,-0.446153846153846,
-0.430769230769231,-0.415384615384615,-0.4,-0.384615384615385,-0.369230769230769,
-0.353846153846154,-0.338461538461538,-0.323076923076923,-0.307692307692308,
-0.292307692307692,-0.276923076923077,-0.261538461538462,-0.246153846153846,
-0.230769230769231,-0.215384615384615,-0.2,-0.184615384615385,-0.169230769230769,
-0.153846153846154,-0.138461538461538,-0.123076923076923,-0.107692307692308,
-0.0923076923076923,-0.0769230769230769,-0.0615384615384615,-0.0461538461538462,
-0.0307692307692308,-0.0153846153846154,0.),(-1.,1.),.UNSPECIFIED.)
GEOMETRIC_REPRESENTATION_ITEM()
RATIONAL_B_SPLINE_SURFACE(((1.,1.),(1.,1.),(1.,1.),(1.,1.),(1.,1.),(1.,
1.),(1.,1.),(1.,1.),(1.,1.),(1.,1.),(1.,1.),(1.,1.),(1.,1.),(1.,1.),(1.,
1.),(1.,1.),(1.,1.),(1.,1.),(1.,1.),(1.,1.),(1.,1.),(1.,1.),(1.,1.),(1.,
1.),(1.,1.),(1.,1.),(1.,1.),(1.,1.),(1.,1.),(1.,1.),(1.,1.),(1.,1.),(1.,
1.),(1.,1.),(1.,1.),(1.,1.),(1.,1.),(1.,1.),(1.,1.),(1.,1.),(1.,1.),(1.,
1.),(1.,1.),(1.,1.),(1.,1.),(1.,1.),(1.,1.),(1.,1.),(1.,1.),(1.,1.),(1.,
1.),(1.,1.),(1.,1.),(1.,1.),(1.,1.),(1.,1.),(1.,1.),(1.,1.),(1.,1.),(1.,
1.),(1.,1.),(1.,1.),(1.,1.),(1.,1.),(1.,1.),(1.,1.),(1.,1.),(1.,1.),(1.,
1.),(1.,1.)))
REPRESENTATION_ITEM('')
SURFACE()
);
#34=(
BOUNDED_SURFACE()
B_SPLINE_SURFACE(5,1,((#30146,#30147),(#30148,#30149),(#30150,#30151),(#30152,
#30153),(#30154,#30155),(#30156,#30157),(#30158,#30159),(#30160,#30161),
(#30162,#30163),(#30164,#30165),(#30166,#30167),(#30168,#30169),(#30170,
#30171),(#30172,#30173),(#30174,#30175),(#30176,#30177),(#30178,#30179),
(#30180,#30181),(#30182,#30183),(#30184,#30185),(#30186,#30187),(#30188,
#30189),(#30190,#30191),(#30192,#30193),(#30194,#30195),(#30196,#30197),
(#30198,#30199),(#30200,#30201),(#30202,#30203),(#30204,#30205),(#30206,
#30207),(#30208,#30209),(#30210,#30211),(#30212,#30213),(#30214,#30215),
(#30216,#30217),(#30218,#30219),(#30220,#30221),(#30222,#30223),(#30224,
#30225),(#30226,#30227),(#30228,#30229),(#30230,#30231),(#30232,#30233),
(#30234,#30235),(#30236,#30237),(#30238,#30239),(#30240,#30241),(#30242,
#30243),(#30244,#30245),(#30246,#30247),(#30248,#30249),(#30250,#30251),
(#30252,#30253),(#30254,#30255),(#30256,#30257),(#30258,#30259),(#30260,
#30261),(#30262,#30263),(#30264,#30265),(#30266,#30267),(#30268,#30269),
(#30270,#30271),(#30272,#30273),(#30274,#30275),(#30276,#30277),(#30278,
#30279),(#30280,#30281),(#30282,#30283),(#30284,#30285)),.UNSPECIFIED.,
 .F.,.F.,.F.)
B_SPLINE_SURFACE_WITH_KNOTS((6,1,1,1,1,1,1,1,1,1,1,1,1,1,1,1,1,1,1,1,1,
1,1,1,1,1,1,1,1,1,1,1,1,1,1,1,1,1,1,1,1,1,1,1,1,1,1,1,1,1,1,1,1,1,1,1,1,
1,1,1,1,1,1,1,1,6),(2,2),(-1.,-0.984615384615383,-0.969230769230768,-0.953846153846152,
-0.938461538461537,-0.923076923076922,-0.907692307692306,-0.892307692307691,
-0.876923076923076,-0.86153846153846,-0.846153846153845,-0.83076923076923,
-0.815384615384614,-0.799999999999999,-0.784615384615384,-0.769230769230768,
-0.753846153846153,-0.738461538461538,-0.723076923076922,-0.707692307692307,
-0.692307692307692,-0.676923076923076,-0.661538461538461,-0.646153846153846,
-0.63076923076923,-0.615384615384615,-0.6,-0.584615384615384,-0.569230769230769,
-0.553846153846154,-0.538461538461538,-0.523076923076923,-0.507692307692308,
-0.492307692307692,-0.476923076923077,-0.461538461538462,-0.446153846153846,
-0.430769230769231,-0.415384615384615,-0.4,-0.384615384615385,-0.369230769230769,
-0.353846153846154,-0.338461538461538,-0.323076923076923,-0.307692307692308,
-0.292307692307692,-0.276923076923077,-0.261538461538462,-0.246153846153846,
-0.230769230769231,-0.215384615384615,-0.2,-0.184615384615385,-0.169230769230769,
-0.153846153846154,-0.138461538461538,-0.123076923076923,-0.107692307692308,
-0.0923076923076923,-0.0769230769230769,-0.0615384615384615,-0.0461538461538462,
-0.0307692307692308,-0.0153846153846154,0.),(-1.,1.),.UNSPECIFIED.)
GEOMETRIC_REPRESENTATION_ITEM()
RATIONAL_B_SPLINE_SURFACE(((1.,1.),(1.,1.),(1.,1.),(1.,1.),(1.,1.),(1.,
1.),(1.,1.),(1.,1.),(1.,1.),(1.,1.),(1.,1.),(1.,1.),(1.,1.),(1.,1.),(1.,
1.),(1.,1.),(1.,1.),(1.,1.),(1.,1.),(1.,1.),(1.,1.),(1.,1.),(1.,1.),(1.,
1.),(1.,1.),(1.,1.),(1.,1.),(1.,1.),(1.,1.),(1.,1.),(1.,1.),(1.,1.),(1.,
1.),(1.,1.),(1.,1.),(1.,1.),(1.,1.),(1.,1.),(1.,1.),(1.,1.),(1.,1.),(1.,
1.),(1.,1.),(1.,1.),(1.,1.),(1.,1.),(1.,1.),(1.,1.),(1.,1.),(1.,1.),(1.,
1.),(1.,1.),(1.,1.),(1.,1.),(1.,1.),(1.,1.),(1.,1.),(1.,1.),(1.,1.),(1.,
1.),(1.,1.),(1.,1.),(1.,1.),(1.,1.),(1.,1.),(1.,1.),(1.,1.),(1.,1.),(1.,
1.),(1.,1.)))
REPRESENTATION_ITEM('')
SURFACE()
);
#35=(
BOUNDED_SURFACE()
B_SPLINE_SURFACE(5,1,((#30362,#30363),(#30364,#30365),(#30366,#30367),(#30368,
#30369),(#30370,#30371),(#30372,#30373),(#30374,#30375),(#30376,#30377),
(#30378,#30379),(#30380,#30381),(#30382,#30383),(#30384,#30385),(#30386,
#30387),(#30388,#30389),(#30390,#30391),(#30392,#30393),(#30394,#30395),
(#30396,#30397),(#30398,#30399),(#30400,#30401),(#30402,#30403),(#30404,
#30405),(#30406,#30407),(#30408,#30409),(#30410,#30411),(#30412,#30413),
(#30414,#30415),(#30416,#30417),(#30418,#30419),(#30420,#30421),(#30422,
#30423),(#30424,#30425),(#30426,#30427),(#30428,#30429),(#30430,#30431),
(#30432,#30433),(#30434,#30435),(#30436,#30437),(#30438,#30439),(#30440,
#30441),(#30442,#30443),(#30444,#30445),(#30446,#30447),(#30448,#30449),
(#30450,#30451),(#30452,#30453),(#30454,#30455),(#30456,#30457),(#30458,
#30459),(#30460,#30461),(#30462,#30463),(#30464,#30465),(#30466,#30467),
(#30468,#30469),(#30470,#30471),(#30472,#30473),(#30474,#30475),(#30476,
#30477),(#30478,#30479),(#30480,#30481),(#30482,#30483),(#30484,#30485),
(#30486,#30487),(#30488,#30489),(#30490,#30491),(#30492,#30493),(#30494,
#30495),(#30496,#30497),(#30498,#30499),(#30500,#30501)),.UNSPECIFIED.,
 .F.,.F.,.F.)
B_SPLINE_SURFACE_WITH_KNOTS((6,1,1,1,1,1,1,1,1,1,1,1,1,1,1,1,1,1,1,1,1,
1,1,1,1,1,1,1,1,1,1,1,1,1,1,1,1,1,1,1,1,1,1,1,1,1,1,1,1,1,1,1,1,1,1,1,1,
1,1,1,1,1,1,1,1,6),(2,2),(-1.,-0.984615384615383,-0.969230769230768,-0.953846153846152,
-0.938461538461537,-0.923076923076922,-0.907692307692306,-0.892307692307691,
-0.876923076923076,-0.86153846153846,-0.846153846153845,-0.83076923076923,
-0.815384615384614,-0.799999999999999,-0.784615384615384,-0.769230769230768,
-0.753846153846153,-0.738461538461538,-0.723076923076922,-0.707692307692307,
-0.692307692307692,-0.676923076923076,-0.661538461538461,-0.646153846153846,
-0.63076923076923,-0.615384615384615,-0.6,-0.584615384615384,-0.569230769230769,
-0.553846153846154,-0.538461538461538,-0.523076923076923,-0.507692307692308,
-0.492307692307692,-0.476923076923077,-0.461538461538462,-0.446153846153846,
-0.430769230769231,-0.415384615384615,-0.4,-0.384615384615385,-0.369230769230769,
-0.353846153846154,-0.338461538461538,-0.323076923076923,-0.307692307692308,
-0.292307692307692,-0.276923076923077,-0.261538461538462,-0.246153846153846,
-0.230769230769231,-0.215384615384615,-0.2,-0.184615384615385,-0.169230769230769,
-0.153846153846154,-0.138461538461538,-0.123076923076923,-0.107692307692308,
-0.0923076923076923,-0.0769230769230769,-0.0615384615384615,-0.0461538461538462,
-0.0307692307692308,-0.0153846153846154,0.),(-1.,1.),.UNSPECIFIED.)
GEOMETRIC_REPRESENTATION_ITEM()
RATIONAL_B_SPLINE_SURFACE(((1.,1.),(1.,1.),(1.,1.),(1.,1.),(1.,1.),(1.,
1.),(1.,1.),(1.,1.),(1.,1.),(1.,1.),(1.,1.),(1.,1.),(1.,1.),(1.,1.),(1.,
1.),(1.,1.),(1.,1.),(1.,1.),(1.,1.),(1.,1.),(1.,1.),(1.,1.),(1.,1.),(1.,
1.),(1.,1.),(1.,1.),(1.,1.),(1.,1.),(1.,1.),(1.,1.),(1.,1.),(1.,1.),(1.,
1.),(1.,1.),(1.,1.),(1.,1.),(1.,1.),(1.,1.),(1.,1.),(1.,1.),(1.,1.),(1.,
1.),(1.,1.),(1.,1.),(1.,1.),(1.,1.),(1.,1.),(1.,1.),(1.,1.),(1.,1.),(1.,
1.),(1.,1.),(1.,1.),(1.,1.),(1.,1.),(1.,1.),(1.,1.),(1.,1.),(1.,1.),(1.,
1.),(1.,1.),(1.,1.),(1.,1.),(1.,1.),(1.,1.),(1.,1.),(1.,1.),(1.,1.),(1.,
1.),(1.,1.)))
REPRESENTATION_ITEM('')
SURFACE()
);
#36=(
BOUNDED_SURFACE()
B_SPLINE_SURFACE(5,1,((#30578,#30579),(#30580,#30581),(#30582,#30583),(#30584,
#30585),(#30586,#30587),(#30588,#30589),(#30590,#30591),(#30592,#30593),
(#30594,#30595),(#30596,#30597),(#30598,#30599),(#30600,#30601),(#30602,
#30603),(#30604,#30605),(#30606,#30607),(#30608,#30609),(#30610,#30611),
(#30612,#30613),(#30614,#30615),(#30616,#30617),(#30618,#30619),(#30620,
#30621),(#30622,#30623),(#30624,#30625),(#30626,#30627),(#30628,#30629),
(#30630,#30631),(#30632,#30633),(#30634,#30635),(#30636,#30637),(#30638,
#30639),(#30640,#30641),(#30642,#30643),(#30644,#30645),(#30646,#30647),
(#30648,#30649),(#30650,#30651),(#30652,#30653),(#30654,#30655),(#30656,
#30657),(#30658,#30659),(#30660,#30661),(#30662,#30663),(#30664,#30665),
(#30666,#30667),(#30668,#30669),(#30670,#30671),(#30672,#30673),(#30674,
#30675),(#30676,#30677),(#30678,#30679),(#30680,#30681),(#30682,#30683),
(#30684,#30685),(#30686,#30687),(#30688,#30689),(#30690,#30691),(#30692,
#30693),(#30694,#30695),(#30696,#30697),(#30698,#30699),(#30700,#30701),
(#30702,#30703),(#30704,#30705),(#30706,#30707),(#30708,#30709),(#30710,
#30711),(#30712,#30713),(#30714,#30715),(#30716,#30717)),.UNSPECIFIED.,
 .F.,.F.,.F.)
B_SPLINE_SURFACE_WITH_KNOTS((6,1,1,1,1,1,1,1,1,1,1,1,1,1,1,1,1,1,1,1,1,
1,1,1,1,1,1,1,1,1,1,1,1,1,1,1,1,1,1,1,1,1,1,1,1,1,1,1,1,1,1,1,1,1,1,1,1,
1,1,1,1,1,1,1,1,6),(2,2),(-1.,-0.984615384615383,-0.969230769230768,-0.953846153846152,
-0.938461538461537,-0.923076923076922,-0.907692307692306,-0.892307692307691,
-0.876923076923076,-0.86153846153846,-0.846153846153845,-0.83076923076923,
-0.815384615384614,-0.799999999999999,-0.784615384615384,-0.769230769230768,
-0.753846153846153,-0.738461538461538,-0.723076923076922,-0.707692307692307,
-0.692307692307692,-0.676923076923076,-0.661538461538461,-0.646153846153846,
-0.63076923076923,-0.615384615384615,-0.6,-0.584615384615384,-0.569230769230769,
-0.553846153846154,-0.538461538461538,-0.523076923076923,-0.507692307692308,
-0.492307692307692,-0.476923076923077,-0.461538461538462,-0.446153846153846,
-0.430769230769231,-0.415384615384615,-0.4,-0.384615384615385,-0.369230769230769,
-0.353846153846154,-0.338461538461538,-0.323076923076923,-0.307692307692308,
-0.292307692307692,-0.276923076923077,-0.261538461538462,-0.246153846153846,
-0.230769230769231,-0.215384615384615,-0.2,-0.184615384615385,-0.169230769230769,
-0.153846153846154,-0.138461538461538,-0.123076923076923,-0.107692307692308,
-0.0923076923076923,-0.0769230769230769,-0.0615384615384615,-0.0461538461538462,
-0.0307692307692308,-0.0153846153846154,0.),(-1.,1.),.UNSPECIFIED.)
GEOMETRIC_REPRESENTATION_ITEM()
RATIONAL_B_SPLINE_SURFACE(((1.,1.),(1.,1.),(1.,1.),(1.,1.),(1.,1.),(1.,
1.),(1.,1.),(1.,1.),(1.,1.),(1.,1.),(1.,1.),(1.,1.),(1.,1.),(1.,1.),(1.,
1.),(1.,1.),(1.,1.),(1.,1.),(1.,1.),(1.,1.),(1.,1.),(1.,1.),(1.,1.),(1.,
1.),(1.,1.),(1.,1.),(1.,1.),(1.,1.),(1.,1.),(1.,1.),(1.,1.),(1.,1.),(1.,
1.),(1.,1.),(1.,1.),(1.,1.),(1.,1.),(1.,1.),(1.,1.),(1.,1.),(1.,1.),(1.,
1.),(1.,1.),(1.,1.),(1.,1.),(1.,1.),(1.,1.),(1.,1.),(1.,1.),(1.,1.),(1.,
1.),(1.,1.),(1.,1.),(1.,1.),(1.,1.),(1.,1.),(1.,1.),(1.,1.),(1.,1.),(1.,
1.),(1.,1.),(1.,1.),(1.,1.),(1.,1.),(1.,1.),(1.,1.),(1.,1.),(1.,1.),(1.,
1.),(1.,1.)))
REPRESENTATION_ITEM('')
SURFACE()
);
#37=(
BOUNDED_SURFACE()
B_SPLINE_SURFACE(5,1,((#30794,#30795),(#30796,#30797),(#30798,#30799),(#30800,
#30801),(#30802,#30803),(#30804,#30805),(#30806,#30807),(#30808,#30809),
(#30810,#30811),(#30812,#30813),(#30814,#30815),(#30816,#30817),(#30818,
#30819),(#30820,#30821),(#30822,#30823),(#30824,#30825),(#30826,#30827),
(#30828,#30829),(#30830,#30831),(#30832,#30833),(#30834,#30835),(#30836,
#30837),(#30838,#30839),(#30840,#30841),(#30842,#30843),(#30844,#30845),
(#30846,#30847),(#30848,#30849),(#30850,#30851),(#30852,#30853),(#30854,
#30855),(#30856,#30857),(#30858,#30859),(#30860,#30861),(#30862,#30863),
(#30864,#30865),(#30866,#30867),(#30868,#30869),(#30870,#30871),(#30872,
#30873),(#30874,#30875),(#30876,#30877),(#30878,#30879),(#30880,#30881),
(#30882,#30883),(#30884,#30885),(#30886,#30887),(#30888,#30889),(#30890,
#30891),(#30892,#30893),(#30894,#30895),(#30896,#30897),(#30898,#30899),
(#30900,#30901),(#30902,#30903),(#30904,#30905),(#30906,#30907),(#30908,
#30909),(#30910,#30911),(#30912,#30913),(#30914,#30915),(#30916,#30917),
(#30918,#30919),(#30920,#30921),(#30922,#30923),(#30924,#30925),(#30926,
#30927),(#30928,#30929),(#30930,#30931),(#30932,#30933)),.UNSPECIFIED.,
 .F.,.F.,.F.)
B_SPLINE_SURFACE_WITH_KNOTS((6,1,1,1,1,1,1,1,1,1,1,1,1,1,1,1,1,1,1,1,1,
1,1,1,1,1,1,1,1,1,1,1,1,1,1,1,1,1,1,1,1,1,1,1,1,1,1,1,1,1,1,1,1,1,1,1,1,
1,1,1,1,1,1,1,1,6),(2,2),(-1.,-0.984615384615383,-0.969230769230768,-0.953846153846152,
-0.938461538461537,-0.923076923076922,-0.907692307692306,-0.892307692307691,
-0.876923076923076,-0.86153846153846,-0.846153846153845,-0.83076923076923,
-0.815384615384614,-0.799999999999999,-0.784615384615384,-0.769230769230768,
-0.753846153846153,-0.738461538461538,-0.723076923076922,-0.707692307692307,
-0.692307692307692,-0.676923076923076,-0.661538461538461,-0.646153846153846,
-0.63076923076923,-0.615384615384615,-0.6,-0.584615384615384,-0.569230769230769,
-0.553846153846154,-0.538461538461538,-0.523076923076923,-0.507692307692308,
-0.492307692307692,-0.476923076923077,-0.461538461538462,-0.446153846153846,
-0.430769230769231,-0.415384615384615,-0.4,-0.384615384615385,-0.369230769230769,
-0.353846153846154,-0.338461538461538,-0.323076923076923,-0.307692307692308,
-0.292307692307692,-0.276923076923077,-0.261538461538462,-0.246153846153846,
-0.230769230769231,-0.215384615384615,-0.2,-0.184615384615385,-0.169230769230769,
-0.153846153846154,-0.138461538461538,-0.123076923076923,-0.107692307692308,
-0.0923076923076923,-0.0769230769230769,-0.0615384615384615,-0.0461538461538462,
-0.0307692307692308,-0.0153846153846154,0.),(-1.,1.),.UNSPECIFIED.)
GEOMETRIC_REPRESENTATION_ITEM()
RATIONAL_B_SPLINE_SURFACE(((1.,1.),(1.,1.),(1.,1.),(1.,1.),(1.,1.),(1.,
1.),(1.,1.),(1.,1.),(1.,1.),(1.,1.),(1.,1.),(1.,1.),(1.,1.),(1.,1.),(1.,
1.),(1.,1.),(1.,1.),(1.,1.),(1.,1.),(1.,1.),(1.,1.),(1.,1.),(1.,1.),(1.,
1.),(1.,1.),(1.,1.),(1.,1.),(1.,1.),(1.,1.),(1.,1.),(1.,1.),(1.,1.),(1.,
1.),(1.,1.),(1.,1.),(1.,1.),(1.,1.),(1.,1.),(1.,1.),(1.,1.),(1.,1.),(1.,
1.),(1.,1.),(1.,1.),(1.,1.),(1.,1.),(1.,1.),(1.,1.),(1.,1.),(1.,1.),(1.,
1.),(1.,1.),(1.,1.),(1.,1.),(1.,1.),(1.,1.),(1.,1.),(1.,1.),(1.,1.),(1.,
1.),(1.,1.),(1.,1.),(1.,1.),(1.,1.),(1.,1.),(1.,1.),(1.,1.),(1.,1.),(1.,
1.),(1.,1.)))
REPRESENTATION_ITEM('')
SURFACE()
);
#38=(
BOUNDED_SURFACE()
B_SPLINE_SURFACE(5,1,((#31010,#31011),(#31012,#31013),(#31014,#31015),(#31016,
#31017),(#31018,#31019),(#31020,#31021),(#31022,#31023),(#31024,#31025),
(#31026,#31027),(#31028,#31029),(#31030,#31031),(#31032,#31033),(#31034,
#31035),(#31036,#31037),(#31038,#31039),(#31040,#31041),(#31042,#31043),
(#31044,#31045),(#31046,#31047),(#31048,#31049),(#31050,#31051),(#31052,
#31053),(#31054,#31055),(#31056,#31057),(#31058,#31059),(#31060,#31061),
(#31062,#31063),(#31064,#31065),(#31066,#31067),(#31068,#31069),(#31070,
#31071),(#31072,#31073),(#31074,#31075),(#31076,#31077),(#31078,#31079),
(#31080,#31081),(#31082,#31083),(#31084,#31085),(#31086,#31087),(#31088,
#31089),(#31090,#31091),(#31092,#31093),(#31094,#31095),(#31096,#31097),
(#31098,#31099),(#31100,#31101),(#31102,#31103),(#31104,#31105),(#31106,
#31107),(#31108,#31109),(#31110,#31111),(#31112,#31113),(#31114,#31115),
(#31116,#31117),(#31118,#31119),(#31120,#31121),(#31122,#31123),(#31124,
#31125),(#31126,#31127),(#31128,#31129),(#31130,#31131),(#31132,#31133),
(#31134,#31135),(#31136,#31137),(#31138,#31139),(#31140,#31141),(#31142,
#31143),(#31144,#31145),(#31146,#31147),(#31148,#31149)),.UNSPECIFIED.,
 .F.,.F.,.F.)
B_SPLINE_SURFACE_WITH_KNOTS((6,1,1,1,1,1,1,1,1,1,1,1,1,1,1,1,1,1,1,1,1,
1,1,1,1,1,1,1,1,1,1,1,1,1,1,1,1,1,1,1,1,1,1,1,1,1,1,1,1,1,1,1,1,1,1,1,1,
1,1,1,1,1,1,1,1,6),(2,2),(-1.,-0.984615384615383,-0.969230769230768,-0.953846153846152,
-0.938461538461537,-0.923076923076922,-0.907692307692306,-0.892307692307691,
-0.876923076923076,-0.86153846153846,-0.846153846153845,-0.83076923076923,
-0.815384615384614,-0.799999999999999,-0.784615384615384,-0.769230769230768,
-0.753846153846153,-0.738461538461538,-0.723076923076922,-0.707692307692307,
-0.692307692307692,-0.676923076923076,-0.661538461538461,-0.646153846153846,
-0.63076923076923,-0.615384615384615,-0.6,-0.584615384615384,-0.569230769230769,
-0.553846153846154,-0.538461538461538,-0.523076923076923,-0.507692307692308,
-0.492307692307692,-0.476923076923077,-0.461538461538462,-0.446153846153846,
-0.430769230769231,-0.415384615384615,-0.4,-0.384615384615385,-0.369230769230769,
-0.353846153846154,-0.338461538461538,-0.323076923076923,-0.307692307692308,
-0.292307692307692,-0.276923076923077,-0.261538461538462,-0.246153846153846,
-0.230769230769231,-0.215384615384615,-0.2,-0.184615384615385,-0.169230769230769,
-0.153846153846154,-0.138461538461538,-0.123076923076923,-0.107692307692308,
-0.0923076923076923,-0.0769230769230769,-0.0615384615384615,-0.0461538461538462,
-0.0307692307692308,-0.0153846153846154,0.),(-1.,1.),.UNSPECIFIED.)
GEOMETRIC_REPRESENTATION_ITEM()
RATIONAL_B_SPLINE_SURFACE(((1.,1.),(1.,1.),(1.,1.),(1.,1.),(1.,1.),(1.,
1.),(1.,1.),(1.,1.),(1.,1.),(1.,1.),(1.,1.),(1.,1.),(1.,1.),(1.,1.),(1.,
1.),(1.,1.),(1.,1.),(1.,1.),(1.,1.),(1.,1.),(1.,1.),(1.,1.),(1.,1.),(1.,
1.),(1.,1.),(1.,1.),(1.,1.),(1.,1.),(1.,1.),(1.,1.),(1.,1.),(1.,1.),(1.,
1.),(1.,1.),(1.,1.),(1.,1.),(1.,1.),(1.,1.),(1.,1.),(1.,1.),(1.,1.),(1.,
1.),(1.,1.),(1.,1.),(1.,1.),(1.,1.),(1.,1.),(1.,1.),(1.,1.),(1.,1.),(1.,
1.),(1.,1.),(1.,1.),(1.,1.),(1.,1.),(1.,1.),(1.,1.),(1.,1.),(1.,1.),(1.,
1.),(1.,1.),(1.,1.),(1.,1.),(1.,1.),(1.,1.),(1.,1.),(1.,1.),(1.,1.),(1.,
1.),(1.,1.)))
REPRESENTATION_ITEM('')
SURFACE()
);
#39=(
BOUNDED_SURFACE()
B_SPLINE_SURFACE(5,1,((#31226,#31227),(#31228,#31229),(#31230,#31231),(#31232,
#31233),(#31234,#31235),(#31236,#31237),(#31238,#31239),(#31240,#31241),
(#31242,#31243),(#31244,#31245),(#31246,#31247),(#31248,#31249),(#31250,
#31251),(#31252,#31253),(#31254,#31255),(#31256,#31257),(#31258,#31259),
(#31260,#31261),(#31262,#31263),(#31264,#31265),(#31266,#31267),(#31268,
#31269),(#31270,#31271),(#31272,#31273),(#31274,#31275),(#31276,#31277),
(#31278,#31279),(#31280,#31281),(#31282,#31283),(#31284,#31285),(#31286,
#31287),(#31288,#31289),(#31290,#31291),(#31292,#31293),(#31294,#31295),
(#31296,#31297),(#31298,#31299),(#31300,#31301),(#31302,#31303),(#31304,
#31305),(#31306,#31307),(#31308,#31309),(#31310,#31311),(#31312,#31313),
(#31314,#31315),(#31316,#31317),(#31318,#31319),(#31320,#31321),(#31322,
#31323),(#31324,#31325),(#31326,#31327),(#31328,#31329),(#31330,#31331),
(#31332,#31333),(#31334,#31335),(#31336,#31337),(#31338,#31339),(#31340,
#31341),(#31342,#31343),(#31344,#31345),(#31346,#31347),(#31348,#31349),
(#31350,#31351),(#31352,#31353),(#31354,#31355),(#31356,#31357),(#31358,
#31359),(#31360,#31361),(#31362,#31363),(#31364,#31365)),.UNSPECIFIED.,
 .F.,.F.,.F.)
B_SPLINE_SURFACE_WITH_KNOTS((6,1,1,1,1,1,1,1,1,1,1,1,1,1,1,1,1,1,1,1,1,
1,1,1,1,1,1,1,1,1,1,1,1,1,1,1,1,1,1,1,1,1,1,1,1,1,1,1,1,1,1,1,1,1,1,1,1,
1,1,1,1,1,1,1,1,6),(2,2),(-1.,-0.984615384615383,-0.969230769230768,-0.953846153846152,
-0.938461538461537,-0.923076923076922,-0.907692307692306,-0.892307692307691,
-0.876923076923076,-0.86153846153846,-0.846153846153845,-0.83076923076923,
-0.815384615384614,-0.799999999999999,-0.784615384615384,-0.769230769230768,
-0.753846153846153,-0.738461538461538,-0.723076923076922,-0.707692307692307,
-0.692307692307692,-0.676923076923076,-0.661538461538461,-0.646153846153846,
-0.63076923076923,-0.615384615384615,-0.6,-0.584615384615384,-0.569230769230769,
-0.553846153846154,-0.538461538461538,-0.523076923076923,-0.507692307692308,
-0.492307692307692,-0.476923076923077,-0.461538461538462,-0.446153846153846,
-0.430769230769231,-0.415384615384615,-0.4,-0.384615384615385,-0.369230769230769,
-0.353846153846154,-0.338461538461538,-0.323076923076923,-0.307692307692308,
-0.292307692307692,-0.276923076923077,-0.261538461538462,-0.246153846153846,
-0.230769230769231,-0.215384615384615,-0.2,-0.184615384615385,-0.169230769230769,
-0.153846153846154,-0.138461538461538,-0.123076923076923,-0.107692307692308,
-0.0923076923076923,-0.0769230769230769,-0.0615384615384615,-0.0461538461538462,
-0.0307692307692308,-0.0153846153846154,0.),(-1.,1.),.UNSPECIFIED.)
GEOMETRIC_REPRESENTATION_ITEM()
RATIONAL_B_SPLINE_SURFACE(((1.,1.),(1.,1.),(1.,1.),(1.,1.),(1.,1.),(1.,
1.),(1.,1.),(1.,1.),(1.,1.),(1.,1.),(1.,1.),(1.,1.),(1.,1.),(1.,1.),(1.,
1.),(1.,1.),(1.,1.),(1.,1.),(1.,1.),(1.,1.),(1.,1.),(1.,1.),(1.,1.),(1.,
1.),(1.,1.),(1.,1.),(1.,1.),(1.,1.),(1.,1.),(1.,1.),(1.,1.),(1.,1.),(1.,
1.),(1.,1.),(1.,1.),(1.,1.),(1.,1.),(1.,1.),(1.,1.),(1.,1.),(1.,1.),(1.,
1.),(1.,1.),(1.,1.),(1.,1.),(1.,1.),(1.,1.),(1.,1.),(1.,1.),(1.,1.),(1.,
1.),(1.,1.),(1.,1.),(1.,1.),(1.,1.),(1.,1.),(1.,1.),(1.,1.),(1.,1.),(1.,
1.),(1.,1.),(1.,1.),(1.,1.),(1.,1.),(1.,1.),(1.,1.),(1.,1.),(1.,1.),(1.,
1.),(1.,1.)))
REPRESENTATION_ITEM('')
SURFACE()
);
#40=(
BOUNDED_SURFACE()
B_SPLINE_SURFACE(5,1,((#31442,#31443),(#31444,#31445),(#31446,#31447),(#31448,
#31449),(#31450,#31451),(#31452,#31453),(#31454,#31455),(#31456,#31457),
(#31458,#31459),(#31460,#31461),(#31462,#31463),(#31464,#31465),(#31466,
#31467),(#31468,#31469),(#31470,#31471),(#31472,#31473),(#31474,#31475),
(#31476,#31477),(#31478,#31479),(#31480,#31481),(#31482,#31483),(#31484,
#31485),(#31486,#31487),(#31488,#31489),(#31490,#31491),(#31492,#31493),
(#31494,#31495),(#31496,#31497),(#31498,#31499),(#31500,#31501),(#31502,
#31503),(#31504,#31505),(#31506,#31507),(#31508,#31509),(#31510,#31511),
(#31512,#31513),(#31514,#31515),(#31516,#31517),(#31518,#31519),(#31520,
#31521),(#31522,#31523),(#31524,#31525),(#31526,#31527),(#31528,#31529),
(#31530,#31531),(#31532,#31533),(#31534,#31535),(#31536,#31537),(#31538,
#31539),(#31540,#31541),(#31542,#31543),(#31544,#31545),(#31546,#31547),
(#31548,#31549),(#31550,#31551),(#31552,#31553),(#31554,#31555),(#31556,
#31557),(#31558,#31559),(#31560,#31561),(#31562,#31563),(#31564,#31565),
(#31566,#31567),(#31568,#31569),(#31570,#31571),(#31572,#31573),(#31574,
#31575),(#31576,#31577),(#31578,#31579),(#31580,#31581)),.UNSPECIFIED.,
 .F.,.F.,.F.)
B_SPLINE_SURFACE_WITH_KNOTS((6,1,1,1,1,1,1,1,1,1,1,1,1,1,1,1,1,1,1,1,1,
1,1,1,1,1,1,1,1,1,1,1,1,1,1,1,1,1,1,1,1,1,1,1,1,1,1,1,1,1,1,1,1,1,1,1,1,
1,1,1,1,1,1,1,1,6),(2,2),(-1.,-0.984615384615383,-0.969230769230768,-0.953846153846152,
-0.938461538461537,-0.923076923076922,-0.907692307692306,-0.892307692307691,
-0.876923076923076,-0.86153846153846,-0.846153846153845,-0.83076923076923,
-0.815384615384614,-0.799999999999999,-0.784615384615384,-0.769230769230768,
-0.753846153846153,-0.738461538461538,-0.723076923076922,-0.707692307692307,
-0.692307692307692,-0.676923076923076,-0.661538461538461,-0.646153846153846,
-0.63076923076923,-0.615384615384615,-0.6,-0.584615384615384,-0.569230769230769,
-0.553846153846154,-0.538461538461538,-0.523076923076923,-0.507692307692308,
-0.492307692307692,-0.476923076923077,-0.461538461538462,-0.446153846153846,
-0.430769230769231,-0.415384615384615,-0.4,-0.384615384615385,-0.369230769230769,
-0.353846153846154,-0.338461538461538,-0.323076923076923,-0.307692307692308,
-0.292307692307692,-0.276923076923077,-0.261538461538462,-0.246153846153846,
-0.230769230769231,-0.215384615384615,-0.2,-0.184615384615385,-0.169230769230769,
-0.153846153846154,-0.138461538461538,-0.123076923076923,-0.107692307692308,
-0.0923076923076923,-0.0769230769230769,-0.0615384615384615,-0.0461538461538462,
-0.0307692307692308,-0.0153846153846154,0.),(-1.,1.),.UNSPECIFIED.)
GEOMETRIC_REPRESENTATION_ITEM()
RATIONAL_B_SPLINE_SURFACE(((1.,1.),(1.,1.),(1.,1.),(1.,1.),(1.,1.),(1.,
1.),(1.,1.),(1.,1.),(1.,1.),(1.,1.),(1.,1.),(1.,1.),(1.,1.),(1.,1.),(1.,
1.),(1.,1.),(1.,1.),(1.,1.),(1.,1.),(1.,1.),(1.,1.),(1.,1.),(1.,1.),(1.,
1.),(1.,1.),(1.,1.),(1.,1.),(1.,1.),(1.,1.),(1.,1.),(1.,1.),(1.,1.),(1.,
1.),(1.,1.),(1.,1.),(1.,1.),(1.,1.),(1.,1.),(1.,1.),(1.,1.),(1.,1.),(1.,
1.),(1.,1.),(1.,1.),(1.,1.),(1.,1.),(1.,1.),(1.,1.),(1.,1.),(1.,1.),(1.,
1.),(1.,1.),(1.,1.),(1.,1.),(1.,1.),(1.,1.),(1.,1.),(1.,1.),(1.,1.),(1.,
1.),(1.,1.),(1.,1.),(1.,1.),(1.,1.),(1.,1.),(1.,1.),(1.,1.),(1.,1.),(1.,
1.),(1.,1.)))
REPRESENTATION_ITEM('')
SURFACE()
);
#41=(
BOUNDED_SURFACE()
B_SPLINE_SURFACE(5,1,((#31658,#31659),(#31660,#31661),(#31662,#31663),(#31664,
#31665),(#31666,#31667),(#31668,#31669),(#31670,#31671),(#31672,#31673),
(#31674,#31675),(#31676,#31677),(#31678,#31679),(#31680,#31681),(#31682,
#31683),(#31684,#31685),(#31686,#31687),(#31688,#31689),(#31690,#31691),
(#31692,#31693),(#31694,#31695),(#31696,#31697),(#31698,#31699),(#31700,
#31701),(#31702,#31703),(#31704,#31705),(#31706,#31707),(#31708,#31709),
(#31710,#31711),(#31712,#31713),(#31714,#31715),(#31716,#31717),(#31718,
#31719),(#31720,#31721),(#31722,#31723),(#31724,#31725),(#31726,#31727),
(#31728,#31729),(#31730,#31731),(#31732,#31733),(#31734,#31735),(#31736,
#31737),(#31738,#31739),(#31740,#31741),(#31742,#31743),(#31744,#31745),
(#31746,#31747),(#31748,#31749),(#31750,#31751),(#31752,#31753),(#31754,
#31755),(#31756,#31757),(#31758,#31759),(#31760,#31761),(#31762,#31763),
(#31764,#31765),(#31766,#31767),(#31768,#31769),(#31770,#31771),(#31772,
#31773),(#31774,#31775),(#31776,#31777),(#31778,#31779),(#31780,#31781),
(#31782,#31783),(#31784,#31785),(#31786,#31787),(#31788,#31789),(#31790,
#31791),(#31792,#31793),(#31794,#31795),(#31796,#31797)),.UNSPECIFIED.,
 .F.,.F.,.F.)
B_SPLINE_SURFACE_WITH_KNOTS((6,1,1,1,1,1,1,1,1,1,1,1,1,1,1,1,1,1,1,1,1,
1,1,1,1,1,1,1,1,1,1,1,1,1,1,1,1,1,1,1,1,1,1,1,1,1,1,1,1,1,1,1,1,1,1,1,1,
1,1,1,1,1,1,1,1,6),(2,2),(-1.,-0.984615384615383,-0.969230769230768,-0.953846153846152,
-0.938461538461537,-0.923076923076922,-0.907692307692306,-0.892307692307691,
-0.876923076923076,-0.86153846153846,-0.846153846153845,-0.83076923076923,
-0.815384615384614,-0.799999999999999,-0.784615384615384,-0.769230769230768,
-0.753846153846153,-0.738461538461538,-0.723076923076922,-0.707692307692307,
-0.692307692307692,-0.676923076923076,-0.661538461538461,-0.646153846153846,
-0.63076923076923,-0.615384615384615,-0.6,-0.584615384615384,-0.569230769230769,
-0.553846153846154,-0.538461538461538,-0.523076923076923,-0.507692307692308,
-0.492307692307692,-0.476923076923077,-0.461538461538462,-0.446153846153846,
-0.430769230769231,-0.415384615384615,-0.4,-0.384615384615385,-0.369230769230769,
-0.353846153846154,-0.338461538461538,-0.323076923076923,-0.307692307692308,
-0.292307692307692,-0.276923076923077,-0.261538461538462,-0.246153846153846,
-0.230769230769231,-0.215384615384615,-0.2,-0.184615384615385,-0.169230769230769,
-0.153846153846154,-0.138461538461538,-0.123076923076923,-0.107692307692308,
-0.0923076923076923,-0.0769230769230769,-0.0615384615384615,-0.0461538461538462,
-0.0307692307692308,-0.0153846153846154,0.),(-1.,1.),.UNSPECIFIED.)
GEOMETRIC_REPRESENTATION_ITEM()
RATIONAL_B_SPLINE_SURFACE(((1.,1.),(1.,1.),(1.,1.),(1.,1.),(1.,1.),(1.,
1.),(1.,1.),(1.,1.),(1.,1.),(1.,1.),(1.,1.),(1.,1.),(1.,1.),(1.,1.),(1.,
1.),(1.,1.),(1.,1.),(1.,1.),(1.,1.),(1.,1.),(1.,1.),(1.,1.),(1.,1.),(1.,
1.),(1.,1.),(1.,1.),(1.,1.),(1.,1.),(1.,1.),(1.,1.),(1.,1.),(1.,1.),(1.,
1.),(1.,1.),(1.,1.),(1.,1.),(1.,1.),(1.,1.),(1.,1.),(1.,1.),(1.,1.),(1.,
1.),(1.,1.),(1.,1.),(1.,1.),(1.,1.),(1.,1.),(1.,1.),(1.,1.),(1.,1.),(1.,
1.),(1.,1.),(1.,1.),(1.,1.),(1.,1.),(1.,1.),(1.,1.),(1.,1.),(1.,1.),(1.,
1.),(1.,1.),(1.,1.),(1.,1.),(1.,1.),(1.,1.),(1.,1.),(1.,1.),(1.,1.),(1.,
1.),(1.,1.)))
REPRESENTATION_ITEM('')
SURFACE()
);
#42=(
BOUNDED_SURFACE()
B_SPLINE_SURFACE(5,1,((#31874,#31875),(#31876,#31877),(#31878,#31879),(#31880,
#31881),(#31882,#31883),(#31884,#31885),(#31886,#31887),(#31888,#31889),
(#31890,#31891),(#31892,#31893),(#31894,#31895),(#31896,#31897),(#31898,
#31899),(#31900,#31901),(#31902,#31903),(#31904,#31905),(#31906,#31907),
(#31908,#31909),(#31910,#31911),(#31912,#31913),(#31914,#31915),(#31916,
#31917),(#31918,#31919),(#31920,#31921),(#31922,#31923),(#31924,#31925),
(#31926,#31927),(#31928,#31929),(#31930,#31931),(#31932,#31933),(#31934,
#31935),(#31936,#31937),(#31938,#31939),(#31940,#31941),(#31942,#31943),
(#31944,#31945),(#31946,#31947),(#31948,#31949),(#31950,#31951),(#31952,
#31953),(#31954,#31955),(#31956,#31957),(#31958,#31959),(#31960,#31961),
(#31962,#31963),(#31964,#31965),(#31966,#31967),(#31968,#31969),(#31970,
#31971),(#31972,#31973),(#31974,#31975),(#31976,#31977),(#31978,#31979),
(#31980,#31981),(#31982,#31983),(#31984,#31985),(#31986,#31987),(#31988,
#31989),(#31990,#31991),(#31992,#31993),(#31994,#31995),(#31996,#31997),
(#31998,#31999),(#32000,#32001),(#32002,#32003),(#32004,#32005),(#32006,
#32007),(#32008,#32009),(#32010,#32011),(#32012,#32013)),.UNSPECIFIED.,
 .F.,.F.,.F.)
B_SPLINE_SURFACE_WITH_KNOTS((6,1,1,1,1,1,1,1,1,1,1,1,1,1,1,1,1,1,1,1,1,
1,1,1,1,1,1,1,1,1,1,1,1,1,1,1,1,1,1,1,1,1,1,1,1,1,1,1,1,1,1,1,1,1,1,1,1,
1,1,1,1,1,1,1,1,6),(2,2),(-1.,-0.984615384615383,-0.969230769230768,-0.953846153846152,
-0.938461538461537,-0.923076923076922,-0.907692307692306,-0.892307692307691,
-0.876923076923076,-0.86153846153846,-0.846153846153845,-0.83076923076923,
-0.815384615384614,-0.799999999999999,-0.784615384615384,-0.769230769230768,
-0.753846153846153,-0.738461538461538,-0.723076923076922,-0.707692307692307,
-0.692307692307692,-0.676923076923076,-0.661538461538461,-0.646153846153846,
-0.63076923076923,-0.615384615384615,-0.6,-0.584615384615384,-0.569230769230769,
-0.553846153846154,-0.538461538461538,-0.523076923076923,-0.507692307692308,
-0.492307692307692,-0.476923076923077,-0.461538461538462,-0.446153846153846,
-0.430769230769231,-0.415384615384615,-0.4,-0.384615384615385,-0.369230769230769,
-0.353846153846154,-0.338461538461538,-0.323076923076923,-0.307692307692308,
-0.292307692307692,-0.276923076923077,-0.261538461538462,-0.246153846153846,
-0.230769230769231,-0.215384615384615,-0.2,-0.184615384615385,-0.169230769230769,
-0.153846153846154,-0.138461538461538,-0.123076923076923,-0.107692307692308,
-0.0923076923076923,-0.0769230769230769,-0.0615384615384615,-0.0461538461538462,
-0.0307692307692308,-0.0153846153846154,0.),(-1.,1.),.UNSPECIFIED.)
GEOMETRIC_REPRESENTATION_ITEM()
RATIONAL_B_SPLINE_SURFACE(((1.,1.),(1.,1.),(1.,1.),(1.,1.),(1.,1.),(1.,
1.),(1.,1.),(1.,1.),(1.,1.),(1.,1.),(1.,1.),(1.,1.),(1.,1.),(1.,1.),(1.,
1.),(1.,1.),(1.,1.),(1.,1.),(1.,1.),(1.,1.),(1.,1.),(1.,1.),(1.,1.),(1.,
1.),(1.,1.),(1.,1.),(1.,1.),(1.,1.),(1.,1.),(1.,1.),(1.,1.),(1.,1.),(1.,
1.),(1.,1.),(1.,1.),(1.,1.),(1.,1.),(1.,1.),(1.,1.),(1.,1.),(1.,1.),(1.,
1.),(1.,1.),(1.,1.),(1.,1.),(1.,1.),(1.,1.),(1.,1.),(1.,1.),(1.,1.),(1.,
1.),(1.,1.),(1.,1.),(1.,1.),(1.,1.),(1.,1.),(1.,1.),(1.,1.),(1.,1.),(1.,
1.),(1.,1.),(1.,1.),(1.,1.),(1.,1.),(1.,1.),(1.,1.),(1.,1.),(1.,1.),(1.,
1.),(1.,1.)))
REPRESENTATION_ITEM('')
SURFACE()
);
#43=(
BOUNDED_SURFACE()
B_SPLINE_SURFACE(5,1,((#32090,#32091),(#32092,#32093),(#32094,#32095),(#32096,
#32097),(#32098,#32099),(#32100,#32101),(#32102,#32103),(#32104,#32105),
(#32106,#32107),(#32108,#32109),(#32110,#32111),(#32112,#32113),(#32114,
#32115),(#32116,#32117),(#32118,#32119),(#32120,#32121),(#32122,#32123),
(#32124,#32125),(#32126,#32127),(#32128,#32129),(#32130,#32131),(#32132,
#32133),(#32134,#32135),(#32136,#32137),(#32138,#32139),(#32140,#32141),
(#32142,#32143),(#32144,#32145),(#32146,#32147),(#32148,#32149),(#32150,
#32151),(#32152,#32153),(#32154,#32155),(#32156,#32157),(#32158,#32159),
(#32160,#32161),(#32162,#32163),(#32164,#32165),(#32166,#32167),(#32168,
#32169),(#32170,#32171),(#32172,#32173),(#32174,#32175),(#32176,#32177),
(#32178,#32179),(#32180,#32181),(#32182,#32183),(#32184,#32185),(#32186,
#32187),(#32188,#32189),(#32190,#32191),(#32192,#32193),(#32194,#32195),
(#32196,#32197),(#32198,#32199),(#32200,#32201),(#32202,#32203),(#32204,
#32205),(#32206,#32207),(#32208,#32209),(#32210,#32211),(#32212,#32213),
(#32214,#32215),(#32216,#32217),(#32218,#32219),(#32220,#32221),(#32222,
#32223),(#32224,#32225),(#32226,#32227),(#32228,#32229)),.UNSPECIFIED.,
 .F.,.F.,.F.)
B_SPLINE_SURFACE_WITH_KNOTS((6,1,1,1,1,1,1,1,1,1,1,1,1,1,1,1,1,1,1,1,1,
1,1,1,1,1,1,1,1,1,1,1,1,1,1,1,1,1,1,1,1,1,1,1,1,1,1,1,1,1,1,1,1,1,1,1,1,
1,1,1,1,1,1,1,1,6),(2,2),(-1.,-0.984615384615383,-0.969230769230768,-0.953846153846152,
-0.938461538461537,-0.923076923076922,-0.907692307692306,-0.892307692307691,
-0.876923076923076,-0.86153846153846,-0.846153846153845,-0.83076923076923,
-0.815384615384614,-0.799999999999999,-0.784615384615384,-0.769230769230768,
-0.753846153846153,-0.738461538461538,-0.723076923076922,-0.707692307692307,
-0.692307692307692,-0.676923076923076,-0.661538461538461,-0.646153846153846,
-0.63076923076923,-0.615384615384615,-0.6,-0.584615384615384,-0.569230769230769,
-0.553846153846154,-0.538461538461538,-0.523076923076923,-0.507692307692308,
-0.492307692307692,-0.476923076923077,-0.461538461538462,-0.446153846153846,
-0.430769230769231,-0.415384615384615,-0.4,-0.384615384615385,-0.369230769230769,
-0.353846153846154,-0.338461538461538,-0.323076923076923,-0.307692307692308,
-0.292307692307692,-0.276923076923077,-0.261538461538462,-0.246153846153846,
-0.230769230769231,-0.215384615384615,-0.2,-0.184615384615385,-0.169230769230769,
-0.153846153846154,-0.138461538461538,-0.123076923076923,-0.107692307692308,
-0.0923076923076923,-0.0769230769230769,-0.0615384615384615,-0.0461538461538462,
-0.0307692307692308,-0.0153846153846154,0.),(-1.,1.),.UNSPECIFIED.)
GEOMETRIC_REPRESENTATION_ITEM()
RATIONAL_B_SPLINE_SURFACE(((1.,1.),(1.,1.),(1.,1.),(1.,1.),(1.,1.),(1.,
1.),(1.,1.),(1.,1.),(1.,1.),(1.,1.),(1.,1.),(1.,1.),(1.,1.),(1.,1.),(1.,
1.),(1.,1.),(1.,1.),(1.,1.),(1.,1.),(1.,1.),(1.,1.),(1.,1.),(1.,1.),(1.,
1.),(1.,1.),(1.,1.),(1.,1.),(1.,1.),(1.,1.),(1.,1.),(1.,1.),(1.,1.),(1.,
1.),(1.,1.),(1.,1.),(1.,1.),(1.,1.),(1.,1.),(1.,1.),(1.,1.),(1.,1.),(1.,
1.),(1.,1.),(1.,1.),(1.,1.),(1.,1.),(1.,1.),(1.,1.),(1.,1.),(1.,1.),(1.,
1.),(1.,1.),(1.,1.),(1.,1.),(1.,1.),(1.,1.),(1.,1.),(1.,1.),(1.,1.),(1.,
1.),(1.,1.),(1.,1.),(1.,1.),(1.,1.),(1.,1.),(1.,1.),(1.,1.),(1.,1.),(1.,
1.),(1.,1.)))
REPRESENTATION_ITEM('')
SURFACE()
);
#44=(
BOUNDED_SURFACE()
B_SPLINE_SURFACE(5,1,((#32306,#32307),(#32308,#32309),(#32310,#32311),(#32312,
#32313),(#32314,#32315),(#32316,#32317),(#32318,#32319),(#32320,#32321),
(#32322,#32323),(#32324,#32325),(#32326,#32327),(#32328,#32329),(#32330,
#32331),(#32332,#32333),(#32334,#32335),(#32336,#32337),(#32338,#32339),
(#32340,#32341),(#32342,#32343),(#32344,#32345),(#32346,#32347),(#32348,
#32349),(#32350,#32351),(#32352,#32353),(#32354,#32355),(#32356,#32357),
(#32358,#32359),(#32360,#32361),(#32362,#32363),(#32364,#32365),(#32366,
#32367),(#32368,#32369),(#32370,#32371),(#32372,#32373),(#32374,#32375),
(#32376,#32377),(#32378,#32379),(#32380,#32381),(#32382,#32383),(#32384,
#32385),(#32386,#32387),(#32388,#32389),(#32390,#32391),(#32392,#32393),
(#32394,#32395),(#32396,#32397),(#32398,#32399),(#32400,#32401),(#32402,
#32403),(#32404,#32405),(#32406,#32407),(#32408,#32409),(#32410,#32411),
(#32412,#32413),(#32414,#32415),(#32416,#32417),(#32418,#32419),(#32420,
#32421),(#32422,#32423),(#32424,#32425),(#32426,#32427),(#32428,#32429),
(#32430,#32431),(#32432,#32433),(#32434,#32435),(#32436,#32437),(#32438,
#32439),(#32440,#32441),(#32442,#32443),(#32444,#32445)),.UNSPECIFIED.,
 .F.,.F.,.F.)
B_SPLINE_SURFACE_WITH_KNOTS((6,1,1,1,1,1,1,1,1,1,1,1,1,1,1,1,1,1,1,1,1,
1,1,1,1,1,1,1,1,1,1,1,1,1,1,1,1,1,1,1,1,1,1,1,1,1,1,1,1,1,1,1,1,1,1,1,1,
1,1,1,1,1,1,1,1,6),(2,2),(-1.,-0.984615384615383,-0.969230769230768,-0.953846153846152,
-0.938461538461537,-0.923076923076922,-0.907692307692306,-0.892307692307691,
-0.876923076923076,-0.86153846153846,-0.846153846153845,-0.83076923076923,
-0.815384615384614,-0.799999999999999,-0.784615384615384,-0.769230769230768,
-0.753846153846153,-0.738461538461538,-0.723076923076922,-0.707692307692307,
-0.692307692307692,-0.676923076923076,-0.661538461538461,-0.646153846153846,
-0.63076923076923,-0.615384615384615,-0.6,-0.584615384615384,-0.569230769230769,
-0.553846153846154,-0.538461538461538,-0.523076923076923,-0.507692307692308,
-0.492307692307692,-0.476923076923077,-0.461538461538462,-0.446153846153846,
-0.430769230769231,-0.415384615384615,-0.4,-0.384615384615385,-0.369230769230769,
-0.353846153846154,-0.338461538461538,-0.323076923076923,-0.307692307692308,
-0.292307692307692,-0.276923076923077,-0.261538461538462,-0.246153846153846,
-0.230769230769231,-0.215384615384615,-0.2,-0.184615384615385,-0.169230769230769,
-0.153846153846154,-0.138461538461538,-0.123076923076923,-0.107692307692308,
-0.0923076923076923,-0.0769230769230769,-0.0615384615384615,-0.0461538461538462,
-0.0307692307692308,-0.0153846153846154,0.),(-1.,1.),.UNSPECIFIED.)
GEOMETRIC_REPRESENTATION_ITEM()
RATIONAL_B_SPLINE_SURFACE(((1.,1.),(1.,1.),(1.,1.),(1.,1.),(1.,1.),(1.,
1.),(1.,1.),(1.,1.),(1.,1.),(1.,1.),(1.,1.),(1.,1.),(1.,1.),(1.,1.),(1.,
1.),(1.,1.),(1.,1.),(1.,1.),(1.,1.),(1.,1.),(1.,1.),(1.,1.),(1.,1.),(1.,
1.),(1.,1.),(1.,1.),(1.,1.),(1.,1.),(1.,1.),(1.,1.),(1.,1.),(1.,1.),(1.,
1.),(1.,1.),(1.,1.),(1.,1.),(1.,1.),(1.,1.),(1.,1.),(1.,1.),(1.,1.),(1.,
1.),(1.,1.),(1.,1.),(1.,1.),(1.,1.),(1.,1.),(1.,1.),(1.,1.),(1.,1.),(1.,
1.),(1.,1.),(1.,1.),(1.,1.),(1.,1.),(1.,1.),(1.,1.),(1.,1.),(1.,1.),(1.,
1.),(1.,1.),(1.,1.),(1.,1.),(1.,1.),(1.,1.),(1.,1.),(1.,1.),(1.,1.),(1.,
1.),(1.,1.)))
REPRESENTATION_ITEM('')
SURFACE()
);
#45=(
BOUNDED_SURFACE()
B_SPLINE_SURFACE(5,1,((#32522,#32523),(#32524,#32525),(#32526,#32527),(#32528,
#32529),(#32530,#32531),(#32532,#32533),(#32534,#32535),(#32536,#32537),
(#32538,#32539),(#32540,#32541),(#32542,#32543),(#32544,#32545),(#32546,
#32547),(#32548,#32549),(#32550,#32551),(#32552,#32553),(#32554,#32555),
(#32556,#32557),(#32558,#32559),(#32560,#32561),(#32562,#32563),(#32564,
#32565),(#32566,#32567),(#32568,#32569),(#32570,#32571),(#32572,#32573),
(#32574,#32575),(#32576,#32577),(#32578,#32579),(#32580,#32581),(#32582,
#32583),(#32584,#32585),(#32586,#32587),(#32588,#32589),(#32590,#32591),
(#32592,#32593),(#32594,#32595),(#32596,#32597),(#32598,#32599),(#32600,
#32601),(#32602,#32603),(#32604,#32605),(#32606,#32607),(#32608,#32609),
(#32610,#32611),(#32612,#32613),(#32614,#32615),(#32616,#32617),(#32618,
#32619),(#32620,#32621),(#32622,#32623),(#32624,#32625),(#32626,#32627),
(#32628,#32629),(#32630,#32631),(#32632,#32633),(#32634,#32635),(#32636,
#32637),(#32638,#32639),(#32640,#32641),(#32642,#32643),(#32644,#32645),
(#32646,#32647),(#32648,#32649),(#32650,#32651),(#32652,#32653),(#32654,
#32655),(#32656,#32657),(#32658,#32659),(#32660,#32661)),.UNSPECIFIED.,
 .F.,.F.,.F.)
B_SPLINE_SURFACE_WITH_KNOTS((6,1,1,1,1,1,1,1,1,1,1,1,1,1,1,1,1,1,1,1,1,
1,1,1,1,1,1,1,1,1,1,1,1,1,1,1,1,1,1,1,1,1,1,1,1,1,1,1,1,1,1,1,1,1,1,1,1,
1,1,1,1,1,1,1,1,6),(2,2),(-1.,-0.984615384615383,-0.969230769230768,-0.953846153846152,
-0.938461538461537,-0.923076923076922,-0.907692307692306,-0.892307692307691,
-0.876923076923076,-0.86153846153846,-0.846153846153845,-0.83076923076923,
-0.815384615384614,-0.799999999999999,-0.784615384615384,-0.769230769230768,
-0.753846153846153,-0.738461538461538,-0.723076923076922,-0.707692307692307,
-0.692307692307692,-0.676923076923076,-0.661538461538461,-0.646153846153846,
-0.63076923076923,-0.615384615384615,-0.6,-0.584615384615384,-0.569230769230769,
-0.553846153846154,-0.538461538461538,-0.523076923076923,-0.507692307692308,
-0.492307692307692,-0.476923076923077,-0.461538461538462,-0.446153846153846,
-0.430769230769231,-0.415384615384615,-0.4,-0.384615384615385,-0.369230769230769,
-0.353846153846154,-0.338461538461538,-0.323076923076923,-0.307692307692308,
-0.292307692307692,-0.276923076923077,-0.261538461538462,-0.246153846153846,
-0.230769230769231,-0.215384615384615,-0.2,-0.184615384615385,-0.169230769230769,
-0.153846153846154,-0.138461538461538,-0.123076923076923,-0.107692307692308,
-0.0923076923076923,-0.0769230769230769,-0.0615384615384615,-0.0461538461538462,
-0.0307692307692308,-0.0153846153846154,0.),(-1.,1.),.UNSPECIFIED.)
GEOMETRIC_REPRESENTATION_ITEM()
RATIONAL_B_SPLINE_SURFACE(((1.,1.),(1.,1.),(1.,1.),(1.,1.),(1.,1.),(1.,
1.),(1.,1.),(1.,1.),(1.,1.),(1.,1.),(1.,1.),(1.,1.),(1.,1.),(1.,1.),(1.,
1.),(1.,1.),(1.,1.),(1.,1.),(1.,1.),(1.,1.),(1.,1.),(1.,1.),(1.,1.),(1.,
1.),(1.,1.),(1.,1.),(1.,1.),(1.,1.),(1.,1.),(1.,1.),(1.,1.),(1.,1.),(1.,
1.),(1.,1.),(1.,1.),(1.,1.),(1.,1.),(1.,1.),(1.,1.),(1.,1.),(1.,1.),(1.,
1.),(1.,1.),(1.,1.),(1.,1.),(1.,1.),(1.,1.),(1.,1.),(1.,1.),(1.,1.),(1.,
1.),(1.,1.),(1.,1.),(1.,1.),(1.,1.),(1.,1.),(1.,1.),(1.,1.),(1.,1.),(1.,
1.),(1.,1.),(1.,1.),(1.,1.),(1.,1.),(1.,1.),(1.,1.),(1.,1.),(1.,1.),(1.,
1.),(1.,1.)))
REPRESENTATION_ITEM('')
SURFACE()
);
#46=(
BOUNDED_SURFACE()
B_SPLINE_SURFACE(5,1,((#32738,#32739),(#32740,#32741),(#32742,#32743),(#32744,
#32745),(#32746,#32747),(#32748,#32749),(#32750,#32751),(#32752,#32753),
(#32754,#32755),(#32756,#32757),(#32758,#32759),(#32760,#32761),(#32762,
#32763),(#32764,#32765),(#32766,#32767),(#32768,#32769),(#32770,#32771),
(#32772,#32773),(#32774,#32775),(#32776,#32777),(#32778,#32779),(#32780,
#32781),(#32782,#32783),(#32784,#32785),(#32786,#32787),(#32788,#32789),
(#32790,#32791),(#32792,#32793),(#32794,#32795),(#32796,#32797),(#32798,
#32799),(#32800,#32801),(#32802,#32803),(#32804,#32805),(#32806,#32807),
(#32808,#32809),(#32810,#32811),(#32812,#32813),(#32814,#32815),(#32816,
#32817),(#32818,#32819),(#32820,#32821),(#32822,#32823),(#32824,#32825),
(#32826,#32827),(#32828,#32829),(#32830,#32831),(#32832,#32833),(#32834,
#32835),(#32836,#32837),(#32838,#32839),(#32840,#32841),(#32842,#32843),
(#32844,#32845),(#32846,#32847),(#32848,#32849),(#32850,#32851),(#32852,
#32853),(#32854,#32855),(#32856,#32857),(#32858,#32859),(#32860,#32861),
(#32862,#32863),(#32864,#32865),(#32866,#32867),(#32868,#32869),(#32870,
#32871),(#32872,#32873),(#32874,#32875),(#32876,#32877)),.UNSPECIFIED.,
 .F.,.F.,.F.)
B_SPLINE_SURFACE_WITH_KNOTS((6,1,1,1,1,1,1,1,1,1,1,1,1,1,1,1,1,1,1,1,1,
1,1,1,1,1,1,1,1,1,1,1,1,1,1,1,1,1,1,1,1,1,1,1,1,1,1,1,1,1,1,1,1,1,1,1,1,
1,1,1,1,1,1,1,1,6),(2,2),(-1.,-0.984615384615383,-0.969230769230768,-0.953846153846152,
-0.938461538461537,-0.923076923076922,-0.907692307692306,-0.892307692307691,
-0.876923076923076,-0.86153846153846,-0.846153846153845,-0.83076923076923,
-0.815384615384614,-0.799999999999999,-0.784615384615384,-0.769230769230768,
-0.753846153846153,-0.738461538461538,-0.723076923076922,-0.707692307692307,
-0.692307692307692,-0.676923076923076,-0.661538461538461,-0.646153846153846,
-0.63076923076923,-0.615384615384615,-0.6,-0.584615384615384,-0.569230769230769,
-0.553846153846154,-0.538461538461538,-0.523076923076923,-0.507692307692308,
-0.492307692307692,-0.476923076923077,-0.461538461538462,-0.446153846153846,
-0.430769230769231,-0.415384615384615,-0.4,-0.384615384615385,-0.369230769230769,
-0.353846153846154,-0.338461538461538,-0.323076923076923,-0.307692307692308,
-0.292307692307692,-0.276923076923077,-0.261538461538462,-0.246153846153846,
-0.230769230769231,-0.215384615384615,-0.2,-0.184615384615385,-0.169230769230769,
-0.153846153846154,-0.138461538461538,-0.123076923076923,-0.107692307692308,
-0.0923076923076923,-0.0769230769230769,-0.0615384615384615,-0.0461538461538462,
-0.0307692307692308,-0.0153846153846154,0.),(-1.,1.),.UNSPECIFIED.)
GEOMETRIC_REPRESENTATION_ITEM()
RATIONAL_B_SPLINE_SURFACE(((1.,1.),(1.,1.),(1.,1.),(1.,1.),(1.,1.),(1.,
1.),(1.,1.),(1.,1.),(1.,1.),(1.,1.),(1.,1.),(1.,1.),(1.,1.),(1.,1.),(1.,
1.),(1.,1.),(1.,1.),(1.,1.),(1.,1.),(1.,1.),(1.,1.),(1.,1.),(1.,1.),(1.,
1.),(1.,1.),(1.,1.),(1.,1.),(1.,1.),(1.,1.),(1.,1.),(1.,1.),(1.,1.),(1.,
1.),(1.,1.),(1.,1.),(1.,1.),(1.,1.),(1.,1.),(1.,1.),(1.,1.),(1.,1.),(1.,
1.),(1.,1.),(1.,1.),(1.,1.),(1.,1.),(1.,1.),(1.,1.),(1.,1.),(1.,1.),(1.,
1.),(1.,1.),(1.,1.),(1.,1.),(1.,1.),(1.,1.),(1.,1.),(1.,1.),(1.,1.),(1.,
1.),(1.,1.),(1.,1.),(1.,1.),(1.,1.),(1.,1.),(1.,1.),(1.,1.),(1.,1.),(1.,
1.),(1.,1.)))
REPRESENTATION_ITEM('')
SURFACE()
);
#47=(
BOUNDED_SURFACE()
B_SPLINE_SURFACE(5,1,((#32954,#32955),(#32956,#32957),(#32958,#32959),(#32960,
#32961),(#32962,#32963),(#32964,#32965),(#32966,#32967),(#32968,#32969),
(#32970,#32971),(#32972,#32973),(#32974,#32975),(#32976,#32977),(#32978,
#32979),(#32980,#32981),(#32982,#32983),(#32984,#32985),(#32986,#32987),
(#32988,#32989),(#32990,#32991),(#32992,#32993),(#32994,#32995),(#32996,
#32997),(#32998,#32999),(#33000,#33001),(#33002,#33003),(#33004,#33005),
(#33006,#33007),(#33008,#33009),(#33010,#33011),(#33012,#33013),(#33014,
#33015),(#33016,#33017),(#33018,#33019),(#33020,#33021),(#33022,#33023),
(#33024,#33025),(#33026,#33027),(#33028,#33029),(#33030,#33031),(#33032,
#33033),(#33034,#33035),(#33036,#33037),(#33038,#33039),(#33040,#33041),
(#33042,#33043),(#33044,#33045),(#33046,#33047),(#33048,#33049),(#33050,
#33051),(#33052,#33053),(#33054,#33055),(#33056,#33057),(#33058,#33059),
(#33060,#33061),(#33062,#33063),(#33064,#33065),(#33066,#33067),(#33068,
#33069),(#33070,#33071),(#33072,#33073),(#33074,#33075),(#33076,#33077),
(#33078,#33079),(#33080,#33081),(#33082,#33083),(#33084,#33085),(#33086,
#33087),(#33088,#33089),(#33090,#33091),(#33092,#33093)),.UNSPECIFIED.,
 .F.,.F.,.F.)
B_SPLINE_SURFACE_WITH_KNOTS((6,1,1,1,1,1,1,1,1,1,1,1,1,1,1,1,1,1,1,1,1,
1,1,1,1,1,1,1,1,1,1,1,1,1,1,1,1,1,1,1,1,1,1,1,1,1,1,1,1,1,1,1,1,1,1,1,1,
1,1,1,1,1,1,1,1,6),(2,2),(-1.,-0.984615384615383,-0.969230769230768,-0.953846153846152,
-0.938461538461537,-0.923076923076922,-0.907692307692306,-0.892307692307691,
-0.876923076923076,-0.86153846153846,-0.846153846153845,-0.83076923076923,
-0.815384615384614,-0.799999999999999,-0.784615384615384,-0.769230769230768,
-0.753846153846153,-0.738461538461538,-0.723076923076922,-0.707692307692307,
-0.692307692307692,-0.676923076923076,-0.661538461538461,-0.646153846153846,
-0.63076923076923,-0.615384615384615,-0.6,-0.584615384615384,-0.569230769230769,
-0.553846153846154,-0.538461538461538,-0.523076923076923,-0.507692307692308,
-0.492307692307692,-0.476923076923077,-0.461538461538462,-0.446153846153846,
-0.430769230769231,-0.415384615384615,-0.4,-0.384615384615385,-0.369230769230769,
-0.353846153846154,-0.338461538461538,-0.323076923076923,-0.307692307692308,
-0.292307692307692,-0.276923076923077,-0.261538461538462,-0.246153846153846,
-0.230769230769231,-0.215384615384615,-0.2,-0.184615384615385,-0.169230769230769,
-0.153846153846154,-0.138461538461538,-0.123076923076923,-0.107692307692308,
-0.0923076923076923,-0.0769230769230769,-0.0615384615384615,-0.0461538461538462,
-0.0307692307692308,-0.0153846153846154,0.),(-1.,1.),.UNSPECIFIED.)
GEOMETRIC_REPRESENTATION_ITEM()
RATIONAL_B_SPLINE_SURFACE(((1.,1.),(1.,1.),(1.,1.),(1.,1.),(1.,1.),(1.,
1.),(1.,1.),(1.,1.),(1.,1.),(1.,1.),(1.,1.),(1.,1.),(1.,1.),(1.,1.),(1.,
1.),(1.,1.),(1.,1.),(1.,1.),(1.,1.),(1.,1.),(1.,1.),(1.,1.),(1.,1.),(1.,
1.),(1.,1.),(1.,1.),(1.,1.),(1.,1.),(1.,1.),(1.,1.),(1.,1.),(1.,1.),(1.,
1.),(1.,1.),(1.,1.),(1.,1.),(1.,1.),(1.,1.),(1.,1.),(1.,1.),(1.,1.),(1.,
1.),(1.,1.),(1.,1.),(1.,1.),(1.,1.),(1.,1.),(1.,1.),(1.,1.),(1.,1.),(1.,
1.),(1.,1.),(1.,1.),(1.,1.),(1.,1.),(1.,1.),(1.,1.),(1.,1.),(1.,1.),(1.,
1.),(1.,1.),(1.,1.),(1.,1.),(1.,1.),(1.,1.),(1.,1.),(1.,1.),(1.,1.),(1.,
1.),(1.,1.)))
REPRESENTATION_ITEM('')
SURFACE()
);
#48=(
BOUNDED_SURFACE()
B_SPLINE_SURFACE(5,1,((#33170,#33171),(#33172,#33173),(#33174,#33175),(#33176,
#33177),(#33178,#33179),(#33180,#33181),(#33182,#33183),(#33184,#33185),
(#33186,#33187),(#33188,#33189),(#33190,#33191),(#33192,#33193),(#33194,
#33195),(#33196,#33197),(#33198,#33199),(#33200,#33201),(#33202,#33203),
(#33204,#33205),(#33206,#33207),(#33208,#33209),(#33210,#33211),(#33212,
#33213),(#33214,#33215),(#33216,#33217),(#33218,#33219),(#33220,#33221),
(#33222,#33223),(#33224,#33225),(#33226,#33227),(#33228,#33229),(#33230,
#33231),(#33232,#33233),(#33234,#33235),(#33236,#33237),(#33238,#33239),
(#33240,#33241),(#33242,#33243),(#33244,#33245),(#33246,#33247),(#33248,
#33249),(#33250,#33251),(#33252,#33253),(#33254,#33255),(#33256,#33257),
(#33258,#33259),(#33260,#33261),(#33262,#33263),(#33264,#33265),(#33266,
#33267),(#33268,#33269),(#33270,#33271),(#33272,#33273),(#33274,#33275),
(#33276,#33277),(#33278,#33279),(#33280,#33281),(#33282,#33283),(#33284,
#33285),(#33286,#33287),(#33288,#33289),(#33290,#33291),(#33292,#33293),
(#33294,#33295),(#33296,#33297),(#33298,#33299),(#33300,#33301),(#33302,
#33303),(#33304,#33305),(#33306,#33307),(#33308,#33309)),.UNSPECIFIED.,
 .F.,.F.,.F.)
B_SPLINE_SURFACE_WITH_KNOTS((6,1,1,1,1,1,1,1,1,1,1,1,1,1,1,1,1,1,1,1,1,
1,1,1,1,1,1,1,1,1,1,1,1,1,1,1,1,1,1,1,1,1,1,1,1,1,1,1,1,1,1,1,1,1,1,1,1,
1,1,1,1,1,1,1,1,6),(2,2),(-1.,-0.984615384615383,-0.969230769230768,-0.953846153846152,
-0.938461538461537,-0.923076923076922,-0.907692307692306,-0.892307692307691,
-0.876923076923076,-0.86153846153846,-0.846153846153845,-0.83076923076923,
-0.815384615384614,-0.799999999999999,-0.784615384615384,-0.769230769230768,
-0.753846153846153,-0.738461538461538,-0.723076923076922,-0.707692307692307,
-0.692307692307692,-0.676923076923076,-0.661538461538461,-0.646153846153846,
-0.63076923076923,-0.615384615384615,-0.6,-0.584615384615384,-0.569230769230769,
-0.553846153846154,-0.538461538461538,-0.523076923076923,-0.507692307692308,
-0.492307692307692,-0.476923076923077,-0.461538461538462,-0.446153846153846,
-0.430769230769231,-0.415384615384615,-0.4,-0.384615384615385,-0.369230769230769,
-0.353846153846154,-0.338461538461538,-0.323076923076923,-0.307692307692308,
-0.292307692307692,-0.276923076923077,-0.261538461538462,-0.246153846153846,
-0.230769230769231,-0.215384615384615,-0.2,-0.184615384615385,-0.169230769230769,
-0.153846153846154,-0.138461538461538,-0.123076923076923,-0.107692307692308,
-0.0923076923076923,-0.0769230769230769,-0.0615384615384615,-0.0461538461538462,
-0.0307692307692308,-0.0153846153846154,0.),(-1.,1.),.UNSPECIFIED.)
GEOMETRIC_REPRESENTATION_ITEM()
RATIONAL_B_SPLINE_SURFACE(((1.,1.),(1.,1.),(1.,1.),(1.,1.),(1.,1.),(1.,
1.),(1.,1.),(1.,1.),(1.,1.),(1.,1.),(1.,1.),(1.,1.),(1.,1.),(1.,1.),(1.,
1.),(1.,1.),(1.,1.),(1.,1.),(1.,1.),(1.,1.),(1.,1.),(1.,1.),(1.,1.),(1.,
1.),(1.,1.),(1.,1.),(1.,1.),(1.,1.),(1.,1.),(1.,1.),(1.,1.),(1.,1.),(1.,
1.),(1.,1.),(1.,1.),(1.,1.),(1.,1.),(1.,1.),(1.,1.),(1.,1.),(1.,1.),(1.,
1.),(1.,1.),(1.,1.),(1.,1.),(1.,1.),(1.,1.),(1.,1.),(1.,1.),(1.,1.),(1.,
1.),(1.,1.),(1.,1.),(1.,1.),(1.,1.),(1.,1.),(1.,1.),(1.,1.),(1.,1.),(1.,
1.),(1.,1.),(1.,1.),(1.,1.),(1.,1.),(1.,1.),(1.,1.),(1.,1.),(1.,1.),(1.,
1.),(1.,1.)))
REPRESENTATION_ITEM('')
SURFACE()
);
#49=(
BOUNDED_SURFACE()
B_SPLINE_SURFACE(5,1,((#33386,#33387),(#33388,#33389),(#33390,#33391),(#33392,
#33393),(#33394,#33395),(#33396,#33397),(#33398,#33399),(#33400,#33401),
(#33402,#33403),(#33404,#33405),(#33406,#33407),(#33408,#33409),(#33410,
#33411),(#33412,#33413),(#33414,#33415),(#33416,#33417),(#33418,#33419),
(#33420,#33421),(#33422,#33423),(#33424,#33425),(#33426,#33427),(#33428,
#33429),(#33430,#33431),(#33432,#33433),(#33434,#33435),(#33436,#33437),
(#33438,#33439),(#33440,#33441),(#33442,#33443),(#33444,#33445),(#33446,
#33447),(#33448,#33449),(#33450,#33451),(#33452,#33453),(#33454,#33455),
(#33456,#33457),(#33458,#33459),(#33460,#33461),(#33462,#33463),(#33464,
#33465),(#33466,#33467),(#33468,#33469),(#33470,#33471),(#33472,#33473),
(#33474,#33475),(#33476,#33477),(#33478,#33479),(#33480,#33481),(#33482,
#33483),(#33484,#33485),(#33486,#33487),(#33488,#33489),(#33490,#33491),
(#33492,#33493),(#33494,#33495),(#33496,#33497),(#33498,#33499),(#33500,
#33501),(#33502,#33503),(#33504,#33505),(#33506,#33507),(#33508,#33509),
(#33510,#33511),(#33512,#33513),(#33514,#33515),(#33516,#33517),(#33518,
#33519),(#33520,#33521),(#33522,#33523),(#33524,#33525)),.UNSPECIFIED.,
 .F.,.F.,.F.)
B_SPLINE_SURFACE_WITH_KNOTS((6,1,1,1,1,1,1,1,1,1,1,1,1,1,1,1,1,1,1,1,1,
1,1,1,1,1,1,1,1,1,1,1,1,1,1,1,1,1,1,1,1,1,1,1,1,1,1,1,1,1,1,1,1,1,1,1,1,
1,1,1,1,1,1,1,1,6),(2,2),(-1.,-0.984615384615383,-0.969230769230768,-0.953846153846152,
-0.938461538461537,-0.923076923076922,-0.907692307692306,-0.892307692307691,
-0.876923076923076,-0.86153846153846,-0.846153846153845,-0.83076923076923,
-0.815384615384614,-0.799999999999999,-0.784615384615384,-0.769230769230768,
-0.753846153846153,-0.738461538461538,-0.723076923076922,-0.707692307692307,
-0.692307692307692,-0.676923076923076,-0.661538461538461,-0.646153846153846,
-0.63076923076923,-0.615384615384615,-0.6,-0.584615384615384,-0.569230769230769,
-0.553846153846154,-0.538461538461538,-0.523076923076923,-0.507692307692308,
-0.492307692307692,-0.476923076923077,-0.461538461538462,-0.446153846153846,
-0.430769230769231,-0.415384615384615,-0.4,-0.384615384615385,-0.369230769230769,
-0.353846153846154,-0.338461538461538,-0.323076923076923,-0.307692307692308,
-0.292307692307692,-0.276923076923077,-0.261538461538462,-0.246153846153846,
-0.230769230769231,-0.215384615384615,-0.2,-0.184615384615385,-0.169230769230769,
-0.153846153846154,-0.138461538461538,-0.123076923076923,-0.107692307692308,
-0.0923076923076923,-0.0769230769230769,-0.0615384615384615,-0.0461538461538462,
-0.0307692307692308,-0.0153846153846154,0.),(-1.,1.),.UNSPECIFIED.)
GEOMETRIC_REPRESENTATION_ITEM()
RATIONAL_B_SPLINE_SURFACE(((1.,1.),(1.,1.),(1.,1.),(1.,1.),(1.,1.),(1.,
1.),(1.,1.),(1.,1.),(1.,1.),(1.,1.),(1.,1.),(1.,1.),(1.,1.),(1.,1.),(1.,
1.),(1.,1.),(1.,1.),(1.,1.),(1.,1.),(1.,1.),(1.,1.),(1.,1.),(1.,1.),(1.,
1.),(1.,1.),(1.,1.),(1.,1.),(1.,1.),(1.,1.),(1.,1.),(1.,1.),(1.,1.),(1.,
1.),(1.,1.),(1.,1.),(1.,1.),(1.,1.),(1.,1.),(1.,1.),(1.,1.),(1.,1.),(1.,
1.),(1.,1.),(1.,1.),(1.,1.),(1.,1.),(1.,1.),(1.,1.),(1.,1.),(1.,1.),(1.,
1.),(1.,1.),(1.,1.),(1.,1.),(1.,1.),(1.,1.),(1.,1.),(1.,1.),(1.,1.),(1.,
1.),(1.,1.),(1.,1.),(1.,1.),(1.,1.),(1.,1.),(1.,1.),(1.,1.),(1.,1.),(1.,
1.),(1.,1.)))
REPRESENTATION_ITEM('')
SURFACE()
);
#50=(
BOUNDED_SURFACE()
B_SPLINE_SURFACE(5,1,((#33602,#33603),(#33604,#33605),(#33606,#33607),(#33608,
#33609),(#33610,#33611),(#33612,#33613),(#33614,#33615),(#33616,#33617),
(#33618,#33619),(#33620,#33621),(#33622,#33623),(#33624,#33625),(#33626,
#33627),(#33628,#33629),(#33630,#33631),(#33632,#33633),(#33634,#33635),
(#33636,#33637),(#33638,#33639),(#33640,#33641),(#33642,#33643),(#33644,
#33645),(#33646,#33647),(#33648,#33649),(#33650,#33651),(#33652,#33653),
(#33654,#33655),(#33656,#33657),(#33658,#33659),(#33660,#33661),(#33662,
#33663),(#33664,#33665),(#33666,#33667),(#33668,#33669),(#33670,#33671),
(#33672,#33673),(#33674,#33675),(#33676,#33677),(#33678,#33679),(#33680,
#33681),(#33682,#33683),(#33684,#33685),(#33686,#33687),(#33688,#33689),
(#33690,#33691),(#33692,#33693),(#33694,#33695),(#33696,#33697),(#33698,
#33699),(#33700,#33701),(#33702,#33703),(#33704,#33705),(#33706,#33707),
(#33708,#33709),(#33710,#33711),(#33712,#33713),(#33714,#33715),(#33716,
#33717),(#33718,#33719),(#33720,#33721),(#33722,#33723),(#33724,#33725),
(#33726,#33727),(#33728,#33729),(#33730,#33731),(#33732,#33733),(#33734,
#33735),(#33736,#33737),(#33738,#33739),(#33740,#33741)),.UNSPECIFIED.,
 .F.,.F.,.F.)
B_SPLINE_SURFACE_WITH_KNOTS((6,1,1,1,1,1,1,1,1,1,1,1,1,1,1,1,1,1,1,1,1,
1,1,1,1,1,1,1,1,1,1,1,1,1,1,1,1,1,1,1,1,1,1,1,1,1,1,1,1,1,1,1,1,1,1,1,1,
1,1,1,1,1,1,1,1,6),(2,2),(-1.,-0.984615384615383,-0.969230769230768,-0.953846153846152,
-0.938461538461537,-0.923076923076922,-0.907692307692306,-0.892307692307691,
-0.876923076923076,-0.86153846153846,-0.846153846153845,-0.83076923076923,
-0.815384615384614,-0.799999999999999,-0.784615384615384,-0.769230769230768,
-0.753846153846153,-0.738461538461538,-0.723076923076922,-0.707692307692307,
-0.692307692307692,-0.676923076923076,-0.661538461538461,-0.646153846153846,
-0.63076923076923,-0.615384615384615,-0.6,-0.584615384615384,-0.569230769230769,
-0.553846153846154,-0.538461538461538,-0.523076923076923,-0.507692307692308,
-0.492307692307692,-0.476923076923077,-0.461538461538462,-0.446153846153846,
-0.430769230769231,-0.415384615384615,-0.4,-0.384615384615385,-0.369230769230769,
-0.353846153846154,-0.338461538461538,-0.323076923076923,-0.307692307692308,
-0.292307692307692,-0.276923076923077,-0.261538461538462,-0.246153846153846,
-0.230769230769231,-0.215384615384615,-0.2,-0.184615384615385,-0.169230769230769,
-0.153846153846154,-0.138461538461538,-0.123076923076923,-0.107692307692308,
-0.0923076923076923,-0.0769230769230769,-0.0615384615384615,-0.0461538461538462,
-0.0307692307692308,-0.0153846153846154,0.),(-1.,1.),.UNSPECIFIED.)
GEOMETRIC_REPRESENTATION_ITEM()
RATIONAL_B_SPLINE_SURFACE(((1.,1.),(1.,1.),(1.,1.),(1.,1.),(1.,1.),(1.,
1.),(1.,1.),(1.,1.),(1.,1.),(1.,1.),(1.,1.),(1.,1.),(1.,1.),(1.,1.),(1.,
1.),(1.,1.),(1.,1.),(1.,1.),(1.,1.),(1.,1.),(1.,1.),(1.,1.),(1.,1.),(1.,
1.),(1.,1.),(1.,1.),(1.,1.),(1.,1.),(1.,1.),(1.,1.),(1.,1.),(1.,1.),(1.,
1.),(1.,1.),(1.,1.),(1.,1.),(1.,1.),(1.,1.),(1.,1.),(1.,1.),(1.,1.),(1.,
1.),(1.,1.),(1.,1.),(1.,1.),(1.,1.),(1.,1.),(1.,1.),(1.,1.),(1.,1.),(1.,
1.),(1.,1.),(1.,1.),(1.,1.),(1.,1.),(1.,1.),(1.,1.),(1.,1.),(1.,1.),(1.,
1.),(1.,1.),(1.,1.),(1.,1.),(1.,1.),(1.,1.),(1.,1.),(1.,1.),(1.,1.),(1.,
1.),(1.,1.)))
REPRESENTATION_ITEM('')
SURFACE()
);
#51=(
BOUNDED_SURFACE()
B_SPLINE_SURFACE(5,1,((#39961,#39962),(#39963,#39964),(#39965,#39966),(#39967,
#39968),(#39969,#39970),(#39971,#39972),(#39973,#39974),(#39975,#39976),
(#39977,#39978),(#39979,#39980),(#39981,#39982),(#39983,#39984),(#39985,
#39986),(#39987,#39988),(#39989,#39990),(#39991,#39992),(#39993,#39994),
(#39995,#39996),(#39997,#39998),(#39999,#40000),(#40001,#40002),(#40003,
#40004),(#40005,#40006),(#40007,#40008),(#40009,#40010),(#40011,#40012),
(#40013,#40014),(#40015,#40016),(#40017,#40018),(#40019,#40020),(#40021,
#40022),(#40023,#40024),(#40025,#40026),(#40027,#40028),(#40029,#40030),
(#40031,#40032),(#40033,#40034),(#40035,#40036),(#40037,#40038),(#40039,
#40040),(#40041,#40042),(#40043,#40044),(#40045,#40046),(#40047,#40048),
(#40049,#40050),(#40051,#40052),(#40053,#40054),(#40055,#40056),(#40057,
#40058),(#40059,#40060),(#40061,#40062),(#40063,#40064),(#40065,#40066),
(#40067,#40068),(#40069,#40070),(#40071,#40072),(#40073,#40074),(#40075,
#40076),(#40077,#40078),(#40079,#40080),(#40081,#40082),(#40083,#40084),
(#40085,#40086),(#40087,#40088),(#40089,#40090),(#40091,#40092),(#40093,
#40094),(#40095,#40096),(#40097,#40098),(#40099,#40100)),.UNSPECIFIED.,
 .F.,.F.,.F.)
B_SPLINE_SURFACE_WITH_KNOTS((6,1,1,1,1,1,1,1,1,1,1,1,1,1,1,1,1,1,1,1,1,
1,1,1,1,1,1,1,1,1,1,1,1,1,1,1,1,1,1,1,1,1,1,1,1,1,1,1,1,1,1,1,1,1,1,1,1,
1,1,1,1,1,1,1,1,6),(2,2),(-1.,-0.984615384615383,-0.969230769230768,-0.953846153846152,
-0.938461538461537,-0.923076923076922,-0.907692307692306,-0.892307692307691,
-0.876923076923076,-0.86153846153846,-0.846153846153845,-0.83076923076923,
-0.815384615384614,-0.799999999999999,-0.784615384615384,-0.769230769230768,
-0.753846153846153,-0.738461538461538,-0.723076923076922,-0.707692307692307,
-0.692307692307692,-0.676923076923076,-0.661538461538461,-0.646153846153846,
-0.63076923076923,-0.615384615384615,-0.6,-0.584615384615384,-0.569230769230769,
-0.553846153846154,-0.538461538461538,-0.523076923076923,-0.507692307692308,
-0.492307692307692,-0.476923076923077,-0.461538461538462,-0.446153846153846,
-0.430769230769231,-0.415384615384615,-0.4,-0.384615384615385,-0.369230769230769,
-0.353846153846154,-0.338461538461538,-0.323076923076923,-0.307692307692308,
-0.292307692307692,-0.276923076923077,-0.261538461538462,-0.246153846153846,
-0.230769230769231,-0.215384615384615,-0.2,-0.184615384615385,-0.169230769230769,
-0.153846153846154,-0.138461538461538,-0.123076923076923,-0.107692307692308,
-0.0923076923076923,-0.0769230769230769,-0.0615384615384615,-0.0461538461538462,
-0.0307692307692308,-0.0153846153846154,0.),(-1.,1.),.UNSPECIFIED.)
GEOMETRIC_REPRESENTATION_ITEM()
RATIONAL_B_SPLINE_SURFACE(((1.,1.),(1.,1.),(1.,1.),(1.,1.),(1.,1.),(1.,
1.),(1.,1.),(1.,1.),(1.,1.),(1.,1.),(1.,1.),(1.,1.),(1.,1.),(1.,1.),(1.,
1.),(1.,1.),(1.,1.),(1.,1.),(1.,1.),(1.,1.),(1.,1.),(1.,1.),(1.,1.),(1.,
1.),(1.,1.),(1.,1.),(1.,1.),(1.,1.),(1.,1.),(1.,1.),(1.,1.),(1.,1.),(1.,
1.),(1.,1.),(1.,1.),(1.,1.),(1.,1.),(1.,1.),(1.,1.),(1.,1.),(1.,1.),(1.,
1.),(1.,1.),(1.,1.),(1.,1.),(1.,1.),(1.,1.),(1.,1.),(1.,1.),(1.,1.),(1.,
1.),(1.,1.),(1.,1.),(1.,1.),(1.,1.),(1.,1.),(1.,1.),(1.,1.),(1.,1.),(1.,
1.),(1.,1.),(1.,1.),(1.,1.),(1.,1.),(1.,1.),(1.,1.),(1.,1.),(1.,1.),(1.,
1.),(1.,1.)))
REPRESENTATION_ITEM('')
SURFACE()
);
#52=(
BOUNDED_SURFACE()
B_SPLINE_SURFACE(5,1,((#40180,#40181),(#40182,#40183),(#40184,#40185),(#40186,
#40187),(#40188,#40189),(#40190,#40191),(#40192,#40193),(#40194,#40195),
(#40196,#40197),(#40198,#40199),(#40200,#40201),(#40202,#40203),(#40204,
#40205),(#40206,#40207),(#40208,#40209),(#40210,#40211),(#40212,#40213),
(#40214,#40215),(#40216,#40217),(#40218,#40219),(#40220,#40221),(#40222,
#40223),(#40224,#40225),(#40226,#40227),(#40228,#40229),(#40230,#40231),
(#40232,#40233),(#40234,#40235),(#40236,#40237),(#40238,#40239),(#40240,
#40241),(#40242,#40243),(#40244,#40245),(#40246,#40247),(#40248,#40249),
(#40250,#40251),(#40252,#40253),(#40254,#40255),(#40256,#40257),(#40258,
#40259),(#40260,#40261),(#40262,#40263),(#40264,#40265),(#40266,#40267),
(#40268,#40269),(#40270,#40271),(#40272,#40273),(#40274,#40275),(#40276,
#40277),(#40278,#40279),(#40280,#40281),(#40282,#40283),(#40284,#40285),
(#40286,#40287),(#40288,#40289),(#40290,#40291),(#40292,#40293),(#40294,
#40295),(#40296,#40297),(#40298,#40299),(#40300,#40301),(#40302,#40303),
(#40304,#40305),(#40306,#40307),(#40308,#40309),(#40310,#40311),(#40312,
#40313),(#40314,#40315),(#40316,#40317),(#40318,#40319)),.UNSPECIFIED.,
 .F.,.F.,.F.)
B_SPLINE_SURFACE_WITH_KNOTS((6,1,1,1,1,1,1,1,1,1,1,1,1,1,1,1,1,1,1,1,1,
1,1,1,1,1,1,1,1,1,1,1,1,1,1,1,1,1,1,1,1,1,1,1,1,1,1,1,1,1,1,1,1,1,1,1,1,
1,1,1,1,1,1,1,1,6),(2,2),(-1.,-0.984615384615383,-0.969230769230768,-0.953846153846152,
-0.938461538461537,-0.923076923076922,-0.907692307692306,-0.892307692307691,
-0.876923076923076,-0.86153846153846,-0.846153846153845,-0.83076923076923,
-0.815384615384614,-0.799999999999999,-0.784615384615384,-0.769230769230768,
-0.753846153846153,-0.738461538461538,-0.723076923076922,-0.707692307692307,
-0.692307692307692,-0.676923076923076,-0.661538461538461,-0.646153846153846,
-0.63076923076923,-0.615384615384615,-0.6,-0.584615384615384,-0.569230769230769,
-0.553846153846154,-0.538461538461538,-0.523076923076923,-0.507692307692308,
-0.492307692307692,-0.476923076923077,-0.461538461538462,-0.446153846153846,
-0.430769230769231,-0.415384615384615,-0.4,-0.384615384615385,-0.369230769230769,
-0.353846153846154,-0.338461538461538,-0.323076923076923,-0.307692307692308,
-0.292307692307692,-0.276923076923077,-0.261538461538462,-0.246153846153846,
-0.230769230769231,-0.215384615384615,-0.2,-0.184615384615385,-0.169230769230769,
-0.153846153846154,-0.138461538461538,-0.123076923076923,-0.107692307692308,
-0.0923076923076923,-0.0769230769230769,-0.0615384615384615,-0.0461538461538462,
-0.0307692307692308,-0.0153846153846154,0.),(-1.,1.),.UNSPECIFIED.)
GEOMETRIC_REPRESENTATION_ITEM()
RATIONAL_B_SPLINE_SURFACE(((1.,1.),(1.,1.),(1.,1.),(1.,1.),(1.,1.),(1.,
1.),(1.,1.),(1.,1.),(1.,1.),(1.,1.),(1.,1.),(1.,1.),(1.,1.),(1.,1.),(1.,
1.),(1.,1.),(1.,1.),(1.,1.),(1.,1.),(1.,1.),(1.,1.),(1.,1.),(1.,1.),(1.,
1.),(1.,1.),(1.,1.),(1.,1.),(1.,1.),(1.,1.),(1.,1.),(1.,1.),(1.,1.),(1.,
1.),(1.,1.),(1.,1.),(1.,1.),(1.,1.),(1.,1.),(1.,1.),(1.,1.),(1.,1.),(1.,
1.),(1.,1.),(1.,1.),(1.,1.),(1.,1.),(1.,1.),(1.,1.),(1.,1.),(1.,1.),(1.,
1.),(1.,1.),(1.,1.),(1.,1.),(1.,1.),(1.,1.),(1.,1.),(1.,1.),(1.,1.),(1.,
1.),(1.,1.),(1.,1.),(1.,1.),(1.,1.),(1.,1.),(1.,1.),(1.,1.),(1.,1.),(1.,
1.),(1.,1.)))
REPRESENTATION_ITEM('')
SURFACE()
);
#53=(
BOUNDED_SURFACE()
B_SPLINE_SURFACE(5,1,((#40410,#40411),(#40412,#40413),(#40414,#40415),(#40416,
#40417),(#40418,#40419),(#40420,#40421),(#40422,#40423),(#40424,#40425),
(#40426,#40427),(#40428,#40429),(#40430,#40431),(#40432,#40433),(#40434,
#40435),(#40436,#40437),(#40438,#40439),(#40440,#40441),(#40442,#40443),
(#40444,#40445),(#40446,#40447),(#40448,#40449),(#40450,#40451),(#40452,
#40453),(#40454,#40455),(#40456,#40457),(#40458,#40459),(#40460,#40461),
(#40462,#40463),(#40464,#40465),(#40466,#40467),(#40468,#40469),(#40470,
#40471),(#40472,#40473),(#40474,#40475),(#40476,#40477),(#40478,#40479),
(#40480,#40481),(#40482,#40483),(#40484,#40485),(#40486,#40487),(#40488,
#40489),(#40490,#40491),(#40492,#40493),(#40494,#40495),(#40496,#40497),
(#40498,#40499),(#40500,#40501),(#40502,#40503),(#40504,#40505),(#40506,
#40507),(#40508,#40509),(#40510,#40511),(#40512,#40513),(#40514,#40515),
(#40516,#40517),(#40518,#40519),(#40520,#40521),(#40522,#40523),(#40524,
#40525),(#40526,#40527),(#40528,#40529),(#40530,#40531),(#40532,#40533),
(#40534,#40535),(#40536,#40537),(#40538,#40539),(#40540,#40541),(#40542,
#40543),(#40544,#40545),(#40546,#40547),(#40548,#40549)),.UNSPECIFIED.,
 .F.,.F.,.F.)
B_SPLINE_SURFACE_WITH_KNOTS((6,1,1,1,1,1,1,1,1,1,1,1,1,1,1,1,1,1,1,1,1,
1,1,1,1,1,1,1,1,1,1,1,1,1,1,1,1,1,1,1,1,1,1,1,1,1,1,1,1,1,1,1,1,1,1,1,1,
1,1,1,1,1,1,1,1,6),(2,2),(-1.,-0.984615384615383,-0.969230769230768,-0.953846153846152,
-0.938461538461537,-0.923076923076922,-0.907692307692306,-0.892307692307691,
-0.876923076923076,-0.86153846153846,-0.846153846153845,-0.83076923076923,
-0.815384615384614,-0.799999999999999,-0.784615384615384,-0.769230769230768,
-0.753846153846153,-0.738461538461538,-0.723076923076922,-0.707692307692307,
-0.692307692307692,-0.676923076923076,-0.661538461538461,-0.646153846153846,
-0.63076923076923,-0.615384615384615,-0.6,-0.584615384615384,-0.569230769230769,
-0.553846153846154,-0.538461538461538,-0.523076923076923,-0.507692307692308,
-0.492307692307692,-0.476923076923077,-0.461538461538462,-0.446153846153846,
-0.430769230769231,-0.415384615384615,-0.4,-0.384615384615385,-0.369230769230769,
-0.353846153846154,-0.338461538461538,-0.323076923076923,-0.307692307692308,
-0.292307692307692,-0.276923076923077,-0.261538461538462,-0.246153846153846,
-0.230769230769231,-0.215384615384615,-0.2,-0.184615384615385,-0.169230769230769,
-0.153846153846154,-0.138461538461538,-0.123076923076923,-0.107692307692308,
-0.0923076923076923,-0.0769230769230769,-0.0615384615384615,-0.0461538461538462,
-0.0307692307692308,-0.0153846153846154,0.),(-1.,1.),.UNSPECIFIED.)
GEOMETRIC_REPRESENTATION_ITEM()
RATIONAL_B_SPLINE_SURFACE(((1.,1.),(1.,1.),(1.,1.),(1.,1.),(1.,1.),(1.,
1.),(1.,1.),(1.,1.),(1.,1.),(1.,1.),(1.,1.),(1.,1.),(1.,1.),(1.,1.),(1.,
1.),(1.,1.),(1.,1.),(1.,1.),(1.,1.),(1.,1.),(1.,1.),(1.,1.),(1.,1.),(1.,
1.),(1.,1.),(1.,1.),(1.,1.),(1.,1.),(1.,1.),(1.,1.),(1.,1.),(1.,1.),(1.,
1.),(1.,1.),(1.,1.),(1.,1.),(1.,1.),(1.,1.),(1.,1.),(1.,1.),(1.,1.),(1.,
1.),(1.,1.),(1.,1.),(1.,1.),(1.,1.),(1.,1.),(1.,1.),(1.,1.),(1.,1.),(1.,
1.),(1.,1.),(1.,1.),(1.,1.),(1.,1.),(1.,1.),(1.,1.),(1.,1.),(1.,1.),(1.,
1.),(1.,1.),(1.,1.),(1.,1.),(1.,1.),(1.,1.),(1.,1.),(1.,1.),(1.,1.),(1.,
1.),(1.,1.)))
REPRESENTATION_ITEM('')
SURFACE()
);
#54=(
BOUNDED_SURFACE()
B_SPLINE_SURFACE(5,1,((#40622,#40623),(#40624,#40625),(#40626,#40627),(#40628,
#40629),(#40630,#40631),(#40632,#40633),(#40634,#40635),(#40636,#40637),
(#40638,#40639),(#40640,#40641),(#40642,#40643),(#40644,#40645),(#40646,
#40647),(#40648,#40649),(#40650,#40651),(#40652,#40653),(#40654,#40655),
(#40656,#40657),(#40658,#40659),(#40660,#40661),(#40662,#40663),(#40664,
#40665),(#40666,#40667),(#40668,#40669),(#40670,#40671),(#40672,#40673),
(#40674,#40675),(#40676,#40677),(#40678,#40679),(#40680,#40681),(#40682,
#40683),(#40684,#40685),(#40686,#40687),(#40688,#40689),(#40690,#40691),
(#40692,#40693),(#40694,#40695),(#40696,#40697),(#40698,#40699),(#40700,
#40701),(#40702,#40703),(#40704,#40705),(#40706,#40707),(#40708,#40709),
(#40710,#40711),(#40712,#40713),(#40714,#40715),(#40716,#40717),(#40718,
#40719),(#40720,#40721),(#40722,#40723),(#40724,#40725),(#40726,#40727),
(#40728,#40729),(#40730,#40731),(#40732,#40733),(#40734,#40735),(#40736,
#40737),(#40738,#40739),(#40740,#40741),(#40742,#40743),(#40744,#40745),
(#40746,#40747),(#40748,#40749),(#40750,#40751),(#40752,#40753),(#40754,
#40755),(#40756,#40757),(#40758,#40759),(#40760,#40761)),.UNSPECIFIED.,
 .F.,.F.,.F.)
B_SPLINE_SURFACE_WITH_KNOTS((6,1,1,1,1,1,1,1,1,1,1,1,1,1,1,1,1,1,1,1,1,
1,1,1,1,1,1,1,1,1,1,1,1,1,1,1,1,1,1,1,1,1,1,1,1,1,1,1,1,1,1,1,1,1,1,1,1,
1,1,1,1,1,1,1,1,6),(2,2),(-1.,-0.984615384615383,-0.969230769230768,-0.953846153846152,
-0.938461538461537,-0.923076923076922,-0.907692307692306,-0.892307692307691,
-0.876923076923076,-0.86153846153846,-0.846153846153845,-0.83076923076923,
-0.815384615384614,-0.799999999999999,-0.784615384615384,-0.769230769230768,
-0.753846153846153,-0.738461538461538,-0.723076923076922,-0.707692307692307,
-0.692307692307692,-0.676923076923076,-0.661538461538461,-0.646153846153846,
-0.63076923076923,-0.615384615384615,-0.6,-0.584615384615384,-0.569230769230769,
-0.553846153846154,-0.538461538461538,-0.523076923076923,-0.507692307692308,
-0.492307692307692,-0.476923076923077,-0.461538461538462,-0.446153846153846,
-0.430769230769231,-0.415384615384615,-0.4,-0.384615384615385,-0.369230769230769,
-0.353846153846154,-0.338461538461538,-0.323076923076923,-0.307692307692308,
-0.292307692307692,-0.276923076923077,-0.261538461538462,-0.246153846153846,
-0.230769230769231,-0.215384615384615,-0.2,-0.184615384615385,-0.169230769230769,
-0.153846153846154,-0.138461538461538,-0.123076923076923,-0.107692307692308,
-0.0923076923076923,-0.0769230769230769,-0.0615384615384615,-0.0461538461538462,
-0.0307692307692308,-0.0153846153846154,0.),(-1.,1.),.UNSPECIFIED.)
GEOMETRIC_REPRESENTATION_ITEM()
RATIONAL_B_SPLINE_SURFACE(((1.,1.),(1.,1.),(1.,1.),(1.,1.),(1.,1.),(1.,
1.),(1.,1.),(1.,1.),(1.,1.),(1.,1.),(1.,1.),(1.,1.),(1.,1.),(1.,1.),(1.,
1.),(1.,1.),(1.,1.),(1.,1.),(1.,1.),(1.,1.),(1.,1.),(1.,1.),(1.,1.),(1.,
1.),(1.,1.),(1.,1.),(1.,1.),(1.,1.),(1.,1.),(1.,1.),(1.,1.),(1.,1.),(1.,
1.),(1.,1.),(1.,1.),(1.,1.),(1.,1.),(1.,1.),(1.,1.),(1.,1.),(1.,1.),(1.,
1.),(1.,1.),(1.,1.),(1.,1.),(1.,1.),(1.,1.),(1.,1.),(1.,1.),(1.,1.),(1.,
1.),(1.,1.),(1.,1.),(1.,1.),(1.,1.),(1.,1.),(1.,1.),(1.,1.),(1.,1.),(1.,
1.),(1.,1.),(1.,1.),(1.,1.),(1.,1.),(1.,1.),(1.,1.),(1.,1.),(1.,1.),(1.,
1.),(1.,1.)))
REPRESENTATION_ITEM('')
SURFACE()
);
#55=(
BOUNDED_SURFACE()
B_SPLINE_SURFACE(5,1,((#40852,#40853),(#40854,#40855),(#40856,#40857),(#40858,
#40859),(#40860,#40861),(#40862,#40863),(#40864,#40865),(#40866,#40867),
(#40868,#40869),(#40870,#40871),(#40872,#40873),(#40874,#40875),(#40876,
#40877),(#40878,#40879),(#40880,#40881),(#40882,#40883),(#40884,#40885),
(#40886,#40887),(#40888,#40889),(#40890,#40891),(#40892,#40893),(#40894,
#40895),(#40896,#40897),(#40898,#40899),(#40900,#40901),(#40902,#40903),
(#40904,#40905),(#40906,#40907),(#40908,#40909),(#40910,#40911),(#40912,
#40913),(#40914,#40915),(#40916,#40917),(#40918,#40919),(#40920,#40921),
(#40922,#40923),(#40924,#40925),(#40926,#40927),(#40928,#40929),(#40930,
#40931),(#40932,#40933),(#40934,#40935),(#40936,#40937),(#40938,#40939),
(#40940,#40941),(#40942,#40943),(#40944,#40945),(#40946,#40947),(#40948,
#40949),(#40950,#40951),(#40952,#40953),(#40954,#40955),(#40956,#40957),
(#40958,#40959),(#40960,#40961),(#40962,#40963),(#40964,#40965),(#40966,
#40967),(#40968,#40969),(#40970,#40971),(#40972,#40973),(#40974,#40975),
(#40976,#40977),(#40978,#40979),(#40980,#40981),(#40982,#40983),(#40984,
#40985),(#40986,#40987),(#40988,#40989),(#40990,#40991)),.UNSPECIFIED.,
 .F.,.F.,.F.)
B_SPLINE_SURFACE_WITH_KNOTS((6,1,1,1,1,1,1,1,1,1,1,1,1,1,1,1,1,1,1,1,1,
1,1,1,1,1,1,1,1,1,1,1,1,1,1,1,1,1,1,1,1,1,1,1,1,1,1,1,1,1,1,1,1,1,1,1,1,
1,1,1,1,1,1,1,1,6),(2,2),(-1.,-0.984615384615383,-0.969230769230768,-0.953846153846152,
-0.938461538461537,-0.923076923076922,-0.907692307692306,-0.892307692307691,
-0.876923076923076,-0.86153846153846,-0.846153846153845,-0.83076923076923,
-0.815384615384614,-0.799999999999999,-0.784615384615384,-0.769230769230768,
-0.753846153846153,-0.738461538461538,-0.723076923076922,-0.707692307692307,
-0.692307692307692,-0.676923076923076,-0.661538461538461,-0.646153846153846,
-0.63076923076923,-0.615384615384615,-0.6,-0.584615384615384,-0.569230769230769,
-0.553846153846154,-0.538461538461538,-0.523076923076923,-0.507692307692308,
-0.492307692307692,-0.476923076923077,-0.461538461538462,-0.446153846153846,
-0.430769230769231,-0.415384615384615,-0.4,-0.384615384615385,-0.369230769230769,
-0.353846153846154,-0.338461538461538,-0.323076923076923,-0.307692307692308,
-0.292307692307692,-0.276923076923077,-0.261538461538462,-0.246153846153846,
-0.230769230769231,-0.215384615384615,-0.2,-0.184615384615385,-0.169230769230769,
-0.153846153846154,-0.138461538461538,-0.123076923076923,-0.107692307692308,
-0.0923076923076923,-0.0769230769230769,-0.0615384615384615,-0.0461538461538462,
-0.0307692307692308,-0.0153846153846154,0.),(-1.,1.),.UNSPECIFIED.)
GEOMETRIC_REPRESENTATION_ITEM()
RATIONAL_B_SPLINE_SURFACE(((1.,1.),(1.,1.),(1.,1.),(1.,1.),(1.,1.),(1.,
1.),(1.,1.),(1.,1.),(1.,1.),(1.,1.),(1.,1.),(1.,1.),(1.,1.),(1.,1.),(1.,
1.),(1.,1.),(1.,1.),(1.,1.),(1.,1.),(1.,1.),(1.,1.),(1.,1.),(1.,1.),(1.,
1.),(1.,1.),(1.,1.),(1.,1.),(1.,1.),(1.,1.),(1.,1.),(1.,1.),(1.,1.),(1.,
1.),(1.,1.),(1.,1.),(1.,1.),(1.,1.),(1.,1.),(1.,1.),(1.,1.),(1.,1.),(1.,
1.),(1.,1.),(1.,1.),(1.,1.),(1.,1.),(1.,1.),(1.,1.),(1.,1.),(1.,1.),(1.,
1.),(1.,1.),(1.,1.),(1.,1.),(1.,1.),(1.,1.),(1.,1.),(1.,1.),(1.,1.),(1.,
1.),(1.,1.),(1.,1.),(1.,1.),(1.,1.),(1.,1.),(1.,1.),(1.,1.),(1.,1.),(1.,
1.),(1.,1.)))
REPRESENTATION_ITEM('')
SURFACE()
);
#56=(
BOUNDED_SURFACE()
B_SPLINE_SURFACE(5,1,((#41064,#41065),(#41066,#41067),(#41068,#41069),(#41070,
#41071),(#41072,#41073),(#41074,#41075),(#41076,#41077),(#41078,#41079),
(#41080,#41081),(#41082,#41083),(#41084,#41085),(#41086,#41087),(#41088,
#41089),(#41090,#41091),(#41092,#41093),(#41094,#41095),(#41096,#41097),
(#41098,#41099),(#41100,#41101),(#41102,#41103),(#41104,#41105),(#41106,
#41107),(#41108,#41109),(#41110,#41111),(#41112,#41113),(#41114,#41115),
(#41116,#41117),(#41118,#41119),(#41120,#41121),(#41122,#41123),(#41124,
#41125),(#41126,#41127),(#41128,#41129),(#41130,#41131),(#41132,#41133),
(#41134,#41135),(#41136,#41137),(#41138,#41139),(#41140,#41141),(#41142,
#41143),(#41144,#41145),(#41146,#41147),(#41148,#41149),(#41150,#41151),
(#41152,#41153),(#41154,#41155),(#41156,#41157),(#41158,#41159),(#41160,
#41161),(#41162,#41163),(#41164,#41165),(#41166,#41167),(#41168,#41169),
(#41170,#41171),(#41172,#41173),(#41174,#41175),(#41176,#41177),(#41178,
#41179),(#41180,#41181),(#41182,#41183),(#41184,#41185),(#41186,#41187),
(#41188,#41189),(#41190,#41191),(#41192,#41193),(#41194,#41195),(#41196,
#41197),(#41198,#41199),(#41200,#41201),(#41202,#41203)),.UNSPECIFIED.,
 .F.,.F.,.F.)
B_SPLINE_SURFACE_WITH_KNOTS((6,1,1,1,1,1,1,1,1,1,1,1,1,1,1,1,1,1,1,1,1,
1,1,1,1,1,1,1,1,1,1,1,1,1,1,1,1,1,1,1,1,1,1,1,1,1,1,1,1,1,1,1,1,1,1,1,1,
1,1,1,1,1,1,1,1,6),(2,2),(-1.,-0.984615384615383,-0.969230769230768,-0.953846153846152,
-0.938461538461537,-0.923076923076922,-0.907692307692306,-0.892307692307691,
-0.876923076923076,-0.86153846153846,-0.846153846153845,-0.83076923076923,
-0.815384615384614,-0.799999999999999,-0.784615384615384,-0.769230769230768,
-0.753846153846153,-0.738461538461538,-0.723076923076922,-0.707692307692307,
-0.692307692307692,-0.676923076923076,-0.661538461538461,-0.646153846153846,
-0.63076923076923,-0.615384615384615,-0.6,-0.584615384615384,-0.569230769230769,
-0.553846153846154,-0.538461538461538,-0.523076923076923,-0.507692307692308,
-0.492307692307692,-0.476923076923077,-0.461538461538462,-0.446153846153846,
-0.430769230769231,-0.415384615384615,-0.4,-0.384615384615385,-0.369230769230769,
-0.353846153846154,-0.338461538461538,-0.323076923076923,-0.307692307692308,
-0.292307692307692,-0.276923076923077,-0.261538461538462,-0.246153846153846,
-0.230769230769231,-0.215384615384615,-0.2,-0.184615384615385,-0.169230769230769,
-0.153846153846154,-0.138461538461538,-0.123076923076923,-0.107692307692308,
-0.0923076923076923,-0.0769230769230769,-0.0615384615384615,-0.0461538461538462,
-0.0307692307692308,-0.0153846153846154,0.),(-1.,1.),.UNSPECIFIED.)
GEOMETRIC_REPRESENTATION_ITEM()
RATIONAL_B_SPLINE_SURFACE(((1.,1.),(1.,1.),(1.,1.),(1.,1.),(1.,1.),(1.,
1.),(1.,1.),(1.,1.),(1.,1.),(1.,1.),(1.,1.),(1.,1.),(1.,1.),(1.,1.),(1.,
1.),(1.,1.),(1.,1.),(1.,1.),(1.,1.),(1.,1.),(1.,1.),(1.,1.),(1.,1.),(1.,
1.),(1.,1.),(1.,1.),(1.,1.),(1.,1.),(1.,1.),(1.,1.),(1.,1.),(1.,1.),(1.,
1.),(1.,1.),(1.,1.),(1.,1.),(1.,1.),(1.,1.),(1.,1.),(1.,1.),(1.,1.),(1.,
1.),(1.,1.),(1.,1.),(1.,1.),(1.,1.),(1.,1.),(1.,1.),(1.,1.),(1.,1.),(1.,
1.),(1.,1.),(1.,1.),(1.,1.),(1.,1.),(1.,1.),(1.,1.),(1.,1.),(1.,1.),(1.,
1.),(1.,1.),(1.,1.),(1.,1.),(1.,1.),(1.,1.),(1.,1.),(1.,1.),(1.,1.),(1.,
1.),(1.,1.)))
REPRESENTATION_ITEM('')
SURFACE()
);
#57=(
BOUNDED_SURFACE()
B_SPLINE_SURFACE(5,1,((#41294,#41295),(#41296,#41297),(#41298,#41299),(#41300,
#41301),(#41302,#41303),(#41304,#41305),(#41306,#41307),(#41308,#41309),
(#41310,#41311),(#41312,#41313),(#41314,#41315),(#41316,#41317),(#41318,
#41319),(#41320,#41321),(#41322,#41323),(#41324,#41325),(#41326,#41327),
(#41328,#41329),(#41330,#41331),(#41332,#41333),(#41334,#41335),(#41336,
#41337),(#41338,#41339),(#41340,#41341),(#41342,#41343),(#41344,#41345),
(#41346,#41347),(#41348,#41349),(#41350,#41351),(#41352,#41353),(#41354,
#41355),(#41356,#41357),(#41358,#41359),(#41360,#41361),(#41362,#41363),
(#41364,#41365),(#41366,#41367),(#41368,#41369),(#41370,#41371),(#41372,
#41373),(#41374,#41375),(#41376,#41377),(#41378,#41379),(#41380,#41381),
(#41382,#41383),(#41384,#41385),(#41386,#41387),(#41388,#41389),(#41390,
#41391),(#41392,#41393),(#41394,#41395),(#41396,#41397),(#41398,#41399),
(#41400,#41401),(#41402,#41403),(#41404,#41405),(#41406,#41407),(#41408,
#41409),(#41410,#41411),(#41412,#41413),(#41414,#41415),(#41416,#41417),
(#41418,#41419),(#41420,#41421),(#41422,#41423),(#41424,#41425),(#41426,
#41427),(#41428,#41429),(#41430,#41431),(#41432,#41433)),.UNSPECIFIED.,
 .F.,.F.,.F.)
B_SPLINE_SURFACE_WITH_KNOTS((6,1,1,1,1,1,1,1,1,1,1,1,1,1,1,1,1,1,1,1,1,
1,1,1,1,1,1,1,1,1,1,1,1,1,1,1,1,1,1,1,1,1,1,1,1,1,1,1,1,1,1,1,1,1,1,1,1,
1,1,1,1,1,1,1,1,6),(2,2),(-1.,-0.984615384615383,-0.969230769230768,-0.953846153846152,
-0.938461538461537,-0.923076923076922,-0.907692307692306,-0.892307692307691,
-0.876923076923076,-0.86153846153846,-0.846153846153845,-0.83076923076923,
-0.815384615384614,-0.799999999999999,-0.784615384615384,-0.769230769230768,
-0.753846153846153,-0.738461538461538,-0.723076923076922,-0.707692307692307,
-0.692307692307692,-0.676923076923076,-0.661538461538461,-0.646153846153846,
-0.63076923076923,-0.615384615384615,-0.6,-0.584615384615384,-0.569230769230769,
-0.553846153846154,-0.538461538461538,-0.523076923076923,-0.507692307692308,
-0.492307692307692,-0.476923076923077,-0.461538461538462,-0.446153846153846,
-0.430769230769231,-0.415384615384615,-0.4,-0.384615384615385,-0.369230769230769,
-0.353846153846154,-0.338461538461538,-0.323076923076923,-0.307692307692308,
-0.292307692307692,-0.276923076923077,-0.261538461538462,-0.246153846153846,
-0.230769230769231,-0.215384615384615,-0.2,-0.184615384615385,-0.169230769230769,
-0.153846153846154,-0.138461538461538,-0.123076923076923,-0.107692307692308,
-0.0923076923076923,-0.0769230769230769,-0.0615384615384615,-0.0461538461538462,
-0.0307692307692308,-0.0153846153846154,0.),(-1.,1.),.UNSPECIFIED.)
GEOMETRIC_REPRESENTATION_ITEM()
RATIONAL_B_SPLINE_SURFACE(((1.,1.),(1.,1.),(1.,1.),(1.,1.),(1.,1.),(1.,
1.),(1.,1.),(1.,1.),(1.,1.),(1.,1.),(1.,1.),(1.,1.),(1.,1.),(1.,1.),(1.,
1.),(1.,1.),(1.,1.),(1.,1.),(1.,1.),(1.,1.),(1.,1.),(1.,1.),(1.,1.),(1.,
1.),(1.,1.),(1.,1.),(1.,1.),(1.,1.),(1.,1.),(1.,1.),(1.,1.),(1.,1.),(1.,
1.),(1.,1.),(1.,1.),(1.,1.),(1.,1.),(1.,1.),(1.,1.),(1.,1.),(1.,1.),(1.,
1.),(1.,1.),(1.,1.),(1.,1.),(1.,1.),(1.,1.),(1.,1.),(1.,1.),(1.,1.),(1.,
1.),(1.,1.),(1.,1.),(1.,1.),(1.,1.),(1.,1.),(1.,1.),(1.,1.),(1.,1.),(1.,
1.),(1.,1.),(1.,1.),(1.,1.),(1.,1.),(1.,1.),(1.,1.),(1.,1.),(1.,1.),(1.,
1.),(1.,1.)))
REPRESENTATION_ITEM('')
SURFACE()
);
#58=(
BOUNDED_SURFACE()
B_SPLINE_SURFACE(5,1,((#41506,#41507),(#41508,#41509),(#41510,#41511),(#41512,
#41513),(#41514,#41515),(#41516,#41517),(#41518,#41519),(#41520,#41521),
(#41522,#41523),(#41524,#41525),(#41526,#41527),(#41528,#41529),(#41530,
#41531),(#41532,#41533),(#41534,#41535),(#41536,#41537),(#41538,#41539),
(#41540,#41541),(#41542,#41543),(#41544,#41545),(#41546,#41547),(#41548,
#41549),(#41550,#41551),(#41552,#41553),(#41554,#41555),(#41556,#41557),
(#41558,#41559),(#41560,#41561),(#41562,#41563),(#41564,#41565),(#41566,
#41567),(#41568,#41569),(#41570,#41571),(#41572,#41573),(#41574,#41575),
(#41576,#41577),(#41578,#41579),(#41580,#41581),(#41582,#41583),(#41584,
#41585),(#41586,#41587),(#41588,#41589),(#41590,#41591),(#41592,#41593),
(#41594,#41595),(#41596,#41597),(#41598,#41599),(#41600,#41601),(#41602,
#41603),(#41604,#41605),(#41606,#41607),(#41608,#41609),(#41610,#41611),
(#41612,#41613),(#41614,#41615),(#41616,#41617),(#41618,#41619),(#41620,
#41621),(#41622,#41623),(#41624,#41625),(#41626,#41627),(#41628,#41629),
(#41630,#41631),(#41632,#41633),(#41634,#41635),(#41636,#41637),(#41638,
#41639),(#41640,#41641),(#41642,#41643),(#41644,#41645)),.UNSPECIFIED.,
 .F.,.F.,.F.)
B_SPLINE_SURFACE_WITH_KNOTS((6,1,1,1,1,1,1,1,1,1,1,1,1,1,1,1,1,1,1,1,1,
1,1,1,1,1,1,1,1,1,1,1,1,1,1,1,1,1,1,1,1,1,1,1,1,1,1,1,1,1,1,1,1,1,1,1,1,
1,1,1,1,1,1,1,1,6),(2,2),(-1.,-0.984615384615383,-0.969230769230768,-0.953846153846152,
-0.938461538461537,-0.923076923076922,-0.907692307692306,-0.892307692307691,
-0.876923076923076,-0.86153846153846,-0.846153846153845,-0.83076923076923,
-0.815384615384614,-0.799999999999999,-0.784615384615384,-0.769230769230768,
-0.753846153846153,-0.738461538461538,-0.723076923076922,-0.707692307692307,
-0.692307692307692,-0.676923076923076,-0.661538461538461,-0.646153846153846,
-0.63076923076923,-0.615384615384615,-0.6,-0.584615384615384,-0.569230769230769,
-0.553846153846154,-0.538461538461538,-0.523076923076923,-0.507692307692308,
-0.492307692307692,-0.476923076923077,-0.461538461538462,-0.446153846153846,
-0.430769230769231,-0.415384615384615,-0.4,-0.384615384615385,-0.369230769230769,
-0.353846153846154,-0.338461538461538,-0.323076923076923,-0.307692307692308,
-0.292307692307692,-0.276923076923077,-0.261538461538462,-0.246153846153846,
-0.230769230769231,-0.215384615384615,-0.2,-0.184615384615385,-0.169230769230769,
-0.153846153846154,-0.138461538461538,-0.123076923076923,-0.107692307692308,
-0.0923076923076923,-0.0769230769230769,-0.0615384615384615,-0.0461538461538462,
-0.0307692307692308,-0.0153846153846154,0.),(-1.,1.),.UNSPECIFIED.)
GEOMETRIC_REPRESENTATION_ITEM()
RATIONAL_B_SPLINE_SURFACE(((1.,1.),(1.,1.),(1.,1.),(1.,1.),(1.,1.),(1.,
1.),(1.,1.),(1.,1.),(1.,1.),(1.,1.),(1.,1.),(1.,1.),(1.,1.),(1.,1.),(1.,
1.),(1.,1.),(1.,1.),(1.,1.),(1.,1.),(1.,1.),(1.,1.),(1.,1.),(1.,1.),(1.,
1.),(1.,1.),(1.,1.),(1.,1.),(1.,1.),(1.,1.),(1.,1.),(1.,1.),(1.,1.),(1.,
1.),(1.,1.),(1.,1.),(1.,1.),(1.,1.),(1.,1.),(1.,1.),(1.,1.),(1.,1.),(1.,
1.),(1.,1.),(1.,1.),(1.,1.),(1.,1.),(1.,1.),(1.,1.),(1.,1.),(1.,1.),(1.,
1.),(1.,1.),(1.,1.),(1.,1.),(1.,1.),(1.,1.),(1.,1.),(1.,1.),(1.,1.),(1.,
1.),(1.,1.),(1.,1.),(1.,1.),(1.,1.),(1.,1.),(1.,1.),(1.,1.),(1.,1.),(1.,
1.),(1.,1.)))
REPRESENTATION_ITEM('')
SURFACE()
);
#59=(
BOUNDED_SURFACE()
B_SPLINE_SURFACE(5,1,((#41736,#41737),(#41738,#41739),(#41740,#41741),(#41742,
#41743),(#41744,#41745),(#41746,#41747),(#41748,#41749),(#41750,#41751),
(#41752,#41753),(#41754,#41755),(#41756,#41757),(#41758,#41759),(#41760,
#41761),(#41762,#41763),(#41764,#41765),(#41766,#41767),(#41768,#41769),
(#41770,#41771),(#41772,#41773),(#41774,#41775),(#41776,#41777),(#41778,
#41779),(#41780,#41781),(#41782,#41783),(#41784,#41785),(#41786,#41787),
(#41788,#41789),(#41790,#41791),(#41792,#41793),(#41794,#41795),(#41796,
#41797),(#41798,#41799),(#41800,#41801),(#41802,#41803),(#41804,#41805),
(#41806,#41807),(#41808,#41809),(#41810,#41811),(#41812,#41813),(#41814,
#41815),(#41816,#41817),(#41818,#41819),(#41820,#41821),(#41822,#41823),
(#41824,#41825),(#41826,#41827),(#41828,#41829),(#41830,#41831),(#41832,
#41833),(#41834,#41835),(#41836,#41837),(#41838,#41839),(#41840,#41841),
(#41842,#41843),(#41844,#41845),(#41846,#41847),(#41848,#41849),(#41850,
#41851),(#41852,#41853),(#41854,#41855),(#41856,#41857),(#41858,#41859),
(#41860,#41861),(#41862,#41863),(#41864,#41865),(#41866,#41867),(#41868,
#41869),(#41870,#41871),(#41872,#41873),(#41874,#41875)),.UNSPECIFIED.,
 .F.,.F.,.F.)
B_SPLINE_SURFACE_WITH_KNOTS((6,1,1,1,1,1,1,1,1,1,1,1,1,1,1,1,1,1,1,1,1,
1,1,1,1,1,1,1,1,1,1,1,1,1,1,1,1,1,1,1,1,1,1,1,1,1,1,1,1,1,1,1,1,1,1,1,1,
1,1,1,1,1,1,1,1,6),(2,2),(-1.,-0.984615384615383,-0.969230769230768,-0.953846153846152,
-0.938461538461537,-0.923076923076922,-0.907692307692306,-0.892307692307691,
-0.876923076923076,-0.86153846153846,-0.846153846153845,-0.83076923076923,
-0.815384615384614,-0.799999999999999,-0.784615384615384,-0.769230769230768,
-0.753846153846153,-0.738461538461538,-0.723076923076922,-0.707692307692307,
-0.692307692307692,-0.676923076923076,-0.661538461538461,-0.646153846153846,
-0.63076923076923,-0.615384615384615,-0.6,-0.584615384615384,-0.569230769230769,
-0.553846153846154,-0.538461538461538,-0.523076923076923,-0.507692307692308,
-0.492307692307692,-0.476923076923077,-0.461538461538462,-0.446153846153846,
-0.430769230769231,-0.415384615384615,-0.4,-0.384615384615385,-0.369230769230769,
-0.353846153846154,-0.338461538461538,-0.323076923076923,-0.307692307692308,
-0.292307692307692,-0.276923076923077,-0.261538461538462,-0.246153846153846,
-0.230769230769231,-0.215384615384615,-0.2,-0.184615384615385,-0.169230769230769,
-0.153846153846154,-0.138461538461538,-0.123076923076923,-0.107692307692308,
-0.0923076923076923,-0.0769230769230769,-0.0615384615384615,-0.0461538461538462,
-0.0307692307692308,-0.0153846153846154,0.),(-1.,1.),.UNSPECIFIED.)
GEOMETRIC_REPRESENTATION_ITEM()
RATIONAL_B_SPLINE_SURFACE(((1.,1.),(1.,1.),(1.,1.),(1.,1.),(1.,1.),(1.,
1.),(1.,1.),(1.,1.),(1.,1.),(1.,1.),(1.,1.),(1.,1.),(1.,1.),(1.,1.),(1.,
1.),(1.,1.),(1.,1.),(1.,1.),(1.,1.),(1.,1.),(1.,1.),(1.,1.),(1.,1.),(1.,
1.),(1.,1.),(1.,1.),(1.,1.),(1.,1.),(1.,1.),(1.,1.),(1.,1.),(1.,1.),(1.,
1.),(1.,1.),(1.,1.),(1.,1.),(1.,1.),(1.,1.),(1.,1.),(1.,1.),(1.,1.),(1.,
1.),(1.,1.),(1.,1.),(1.,1.),(1.,1.),(1.,1.),(1.,1.),(1.,1.),(1.,1.),(1.,
1.),(1.,1.),(1.,1.),(1.,1.),(1.,1.),(1.,1.),(1.,1.),(1.,1.),(1.,1.),(1.,
1.),(1.,1.),(1.,1.),(1.,1.),(1.,1.),(1.,1.),(1.,1.),(1.,1.),(1.,1.),(1.,
1.),(1.,1.)))
REPRESENTATION_ITEM('')
SURFACE()
);
#60=(
BOUNDED_SURFACE()
B_SPLINE_SURFACE(5,1,((#41948,#41949),(#41950,#41951),(#41952,#41953),(#41954,
#41955),(#41956,#41957),(#41958,#41959),(#41960,#41961),(#41962,#41963),
(#41964,#41965),(#41966,#41967),(#41968,#41969),(#41970,#41971),(#41972,
#41973),(#41974,#41975),(#41976,#41977),(#41978,#41979),(#41980,#41981),
(#41982,#41983),(#41984,#41985),(#41986,#41987),(#41988,#41989),(#41990,
#41991),(#41992,#41993),(#41994,#41995),(#41996,#41997),(#41998,#41999),
(#42000,#42001),(#42002,#42003),(#42004,#42005),(#42006,#42007),(#42008,
#42009),(#42010,#42011),(#42012,#42013),(#42014,#42015),(#42016,#42017),
(#42018,#42019),(#42020,#42021),(#42022,#42023),(#42024,#42025),(#42026,
#42027),(#42028,#42029),(#42030,#42031),(#42032,#42033),(#42034,#42035),
(#42036,#42037),(#42038,#42039),(#42040,#42041),(#42042,#42043),(#42044,
#42045),(#42046,#42047),(#42048,#42049),(#42050,#42051),(#42052,#42053),
(#42054,#42055),(#42056,#42057),(#42058,#42059),(#42060,#42061),(#42062,
#42063),(#42064,#42065),(#42066,#42067),(#42068,#42069),(#42070,#42071),
(#42072,#42073),(#42074,#42075),(#42076,#42077),(#42078,#42079),(#42080,
#42081),(#42082,#42083),(#42084,#42085),(#42086,#42087)),.UNSPECIFIED.,
 .F.,.F.,.F.)
B_SPLINE_SURFACE_WITH_KNOTS((6,1,1,1,1,1,1,1,1,1,1,1,1,1,1,1,1,1,1,1,1,
1,1,1,1,1,1,1,1,1,1,1,1,1,1,1,1,1,1,1,1,1,1,1,1,1,1,1,1,1,1,1,1,1,1,1,1,
1,1,1,1,1,1,1,1,6),(2,2),(-1.,-0.984615384615383,-0.969230769230768,-0.953846153846152,
-0.938461538461537,-0.923076923076922,-0.907692307692306,-0.892307692307691,
-0.876923076923076,-0.86153846153846,-0.846153846153845,-0.83076923076923,
-0.815384615384614,-0.799999999999999,-0.784615384615384,-0.769230769230768,
-0.753846153846153,-0.738461538461538,-0.723076923076922,-0.707692307692307,
-0.692307692307692,-0.676923076923076,-0.661538461538461,-0.646153846153846,
-0.63076923076923,-0.615384615384615,-0.6,-0.584615384615384,-0.569230769230769,
-0.553846153846154,-0.538461538461538,-0.523076923076923,-0.507692307692308,
-0.492307692307692,-0.476923076923077,-0.461538461538462,-0.446153846153846,
-0.430769230769231,-0.415384615384615,-0.4,-0.384615384615385,-0.369230769230769,
-0.353846153846154,-0.338461538461538,-0.323076923076923,-0.307692307692308,
-0.292307692307692,-0.276923076923077,-0.261538461538462,-0.246153846153846,
-0.230769230769231,-0.215384615384615,-0.2,-0.184615384615385,-0.169230769230769,
-0.153846153846154,-0.138461538461538,-0.123076923076923,-0.107692307692308,
-0.0923076923076923,-0.0769230769230769,-0.0615384615384615,-0.0461538461538462,
-0.0307692307692308,-0.0153846153846154,0.),(-1.,1.),.UNSPECIFIED.)
GEOMETRIC_REPRESENTATION_ITEM()
RATIONAL_B_SPLINE_SURFACE(((1.,1.),(1.,1.),(1.,1.),(1.,1.),(1.,1.),(1.,
1.),(1.,1.),(1.,1.),(1.,1.),(1.,1.),(1.,1.),(1.,1.),(1.,1.),(1.,1.),(1.,
1.),(1.,1.),(1.,1.),(1.,1.),(1.,1.),(1.,1.),(1.,1.),(1.,1.),(1.,1.),(1.,
1.),(1.,1.),(1.,1.),(1.,1.),(1.,1.),(1.,1.),(1.,1.),(1.,1.),(1.,1.),(1.,
1.),(1.,1.),(1.,1.),(1.,1.),(1.,1.),(1.,1.),(1.,1.),(1.,1.),(1.,1.),(1.,
1.),(1.,1.),(1.,1.),(1.,1.),(1.,1.),(1.,1.),(1.,1.),(1.,1.),(1.,1.),(1.,
1.),(1.,1.),(1.,1.),(1.,1.),(1.,1.),(1.,1.),(1.,1.),(1.,1.),(1.,1.),(1.,
1.),(1.,1.),(1.,1.),(1.,1.),(1.,1.),(1.,1.),(1.,1.),(1.,1.),(1.,1.),(1.,
1.),(1.,1.)))
REPRESENTATION_ITEM('')
SURFACE()
);
#61=(
BOUNDED_SURFACE()
B_SPLINE_SURFACE(5,1,((#42178,#42179),(#42180,#42181),(#42182,#42183),(#42184,
#42185),(#42186,#42187),(#42188,#42189),(#42190,#42191),(#42192,#42193),
(#42194,#42195),(#42196,#42197),(#42198,#42199),(#42200,#42201),(#42202,
#42203),(#42204,#42205),(#42206,#42207),(#42208,#42209),(#42210,#42211),
(#42212,#42213),(#42214,#42215),(#42216,#42217),(#42218,#42219),(#42220,
#42221),(#42222,#42223),(#42224,#42225),(#42226,#42227),(#42228,#42229),
(#42230,#42231),(#42232,#42233),(#42234,#42235),(#42236,#42237),(#42238,
#42239),(#42240,#42241),(#42242,#42243),(#42244,#42245),(#42246,#42247),
(#42248,#42249),(#42250,#42251),(#42252,#42253),(#42254,#42255),(#42256,
#42257),(#42258,#42259),(#42260,#42261),(#42262,#42263),(#42264,#42265),
(#42266,#42267),(#42268,#42269),(#42270,#42271),(#42272,#42273),(#42274,
#42275),(#42276,#42277),(#42278,#42279),(#42280,#42281),(#42282,#42283),
(#42284,#42285),(#42286,#42287),(#42288,#42289),(#42290,#42291),(#42292,
#42293),(#42294,#42295),(#42296,#42297),(#42298,#42299),(#42300,#42301),
(#42302,#42303),(#42304,#42305),(#42306,#42307),(#42308,#42309),(#42310,
#42311),(#42312,#42313),(#42314,#42315),(#42316,#42317)),.UNSPECIFIED.,
 .F.,.F.,.F.)
B_SPLINE_SURFACE_WITH_KNOTS((6,1,1,1,1,1,1,1,1,1,1,1,1,1,1,1,1,1,1,1,1,
1,1,1,1,1,1,1,1,1,1,1,1,1,1,1,1,1,1,1,1,1,1,1,1,1,1,1,1,1,1,1,1,1,1,1,1,
1,1,1,1,1,1,1,1,6),(2,2),(-1.,-0.984615384615383,-0.969230769230768,-0.953846153846152,
-0.938461538461537,-0.923076923076922,-0.907692307692306,-0.892307692307691,
-0.876923076923076,-0.86153846153846,-0.846153846153845,-0.83076923076923,
-0.815384615384614,-0.799999999999999,-0.784615384615384,-0.769230769230768,
-0.753846153846153,-0.738461538461538,-0.723076923076922,-0.707692307692307,
-0.692307692307692,-0.676923076923076,-0.661538461538461,-0.646153846153846,
-0.63076923076923,-0.615384615384615,-0.6,-0.584615384615384,-0.569230769230769,
-0.553846153846154,-0.538461538461538,-0.523076923076923,-0.507692307692308,
-0.492307692307692,-0.476923076923077,-0.461538461538462,-0.446153846153846,
-0.430769230769231,-0.415384615384615,-0.4,-0.384615384615385,-0.369230769230769,
-0.353846153846154,-0.338461538461538,-0.323076923076923,-0.307692307692308,
-0.292307692307692,-0.276923076923077,-0.261538461538462,-0.246153846153846,
-0.230769230769231,-0.215384615384615,-0.2,-0.184615384615385,-0.169230769230769,
-0.153846153846154,-0.138461538461538,-0.123076923076923,-0.107692307692308,
-0.0923076923076923,-0.0769230769230769,-0.0615384615384615,-0.0461538461538462,
-0.0307692307692308,-0.0153846153846154,0.),(-1.,1.),.UNSPECIFIED.)
GEOMETRIC_REPRESENTATION_ITEM()
RATIONAL_B_SPLINE_SURFACE(((1.,1.),(1.,1.),(1.,1.),(1.,1.),(1.,1.),(1.,
1.),(1.,1.),(1.,1.),(1.,1.),(1.,1.),(1.,1.),(1.,1.),(1.,1.),(1.,1.),(1.,
1.),(1.,1.),(1.,1.),(1.,1.),(1.,1.),(1.,1.),(1.,1.),(1.,1.),(1.,1.),(1.,
1.),(1.,1.),(1.,1.),(1.,1.),(1.,1.),(1.,1.),(1.,1.),(1.,1.),(1.,1.),(1.,
1.),(1.,1.),(1.,1.),(1.,1.),(1.,1.),(1.,1.),(1.,1.),(1.,1.),(1.,1.),(1.,
1.),(1.,1.),(1.,1.),(1.,1.),(1.,1.),(1.,1.),(1.,1.),(1.,1.),(1.,1.),(1.,
1.),(1.,1.),(1.,1.),(1.,1.),(1.,1.),(1.,1.),(1.,1.),(1.,1.),(1.,1.),(1.,
1.),(1.,1.),(1.,1.),(1.,1.),(1.,1.),(1.,1.),(1.,1.),(1.,1.),(1.,1.),(1.,
1.),(1.,1.)))
REPRESENTATION_ITEM('')
SURFACE()
);
#62=(
BOUNDED_SURFACE()
B_SPLINE_SURFACE(5,1,((#42390,#42391),(#42392,#42393),(#42394,#42395),(#42396,
#42397),(#42398,#42399),(#42400,#42401),(#42402,#42403),(#42404,#42405),
(#42406,#42407),(#42408,#42409),(#42410,#42411),(#42412,#42413),(#42414,
#42415),(#42416,#42417),(#42418,#42419),(#42420,#42421),(#42422,#42423),
(#42424,#42425),(#42426,#42427),(#42428,#42429),(#42430,#42431),(#42432,
#42433),(#42434,#42435),(#42436,#42437),(#42438,#42439),(#42440,#42441),
(#42442,#42443),(#42444,#42445),(#42446,#42447),(#42448,#42449),(#42450,
#42451),(#42452,#42453),(#42454,#42455),(#42456,#42457),(#42458,#42459),
(#42460,#42461),(#42462,#42463),(#42464,#42465),(#42466,#42467),(#42468,
#42469),(#42470,#42471),(#42472,#42473),(#42474,#42475),(#42476,#42477),
(#42478,#42479),(#42480,#42481),(#42482,#42483),(#42484,#42485),(#42486,
#42487),(#42488,#42489),(#42490,#42491),(#42492,#42493),(#42494,#42495),
(#42496,#42497),(#42498,#42499),(#42500,#42501),(#42502,#42503),(#42504,
#42505),(#42506,#42507),(#42508,#42509),(#42510,#42511),(#42512,#42513),
(#42514,#42515),(#42516,#42517),(#42518,#42519),(#42520,#42521),(#42522,
#42523),(#42524,#42525),(#42526,#42527),(#42528,#42529)),.UNSPECIFIED.,
 .F.,.F.,.F.)
B_SPLINE_SURFACE_WITH_KNOTS((6,1,1,1,1,1,1,1,1,1,1,1,1,1,1,1,1,1,1,1,1,
1,1,1,1,1,1,1,1,1,1,1,1,1,1,1,1,1,1,1,1,1,1,1,1,1,1,1,1,1,1,1,1,1,1,1,1,
1,1,1,1,1,1,1,1,6),(2,2),(-1.,-0.984615384615383,-0.969230769230768,-0.953846153846152,
-0.938461538461537,-0.923076923076922,-0.907692307692306,-0.892307692307691,
-0.876923076923076,-0.86153846153846,-0.846153846153845,-0.83076923076923,
-0.815384615384614,-0.799999999999999,-0.784615384615384,-0.769230769230768,
-0.753846153846153,-0.738461538461538,-0.723076923076922,-0.707692307692307,
-0.692307692307692,-0.676923076923076,-0.661538461538461,-0.646153846153846,
-0.63076923076923,-0.615384615384615,-0.6,-0.584615384615384,-0.569230769230769,
-0.553846153846154,-0.538461538461538,-0.523076923076923,-0.507692307692308,
-0.492307692307692,-0.476923076923077,-0.461538461538462,-0.446153846153846,
-0.430769230769231,-0.415384615384615,-0.4,-0.384615384615385,-0.369230769230769,
-0.353846153846154,-0.338461538461538,-0.323076923076923,-0.307692307692308,
-0.292307692307692,-0.276923076923077,-0.261538461538462,-0.246153846153846,
-0.230769230769231,-0.215384615384615,-0.2,-0.184615384615385,-0.169230769230769,
-0.153846153846154,-0.138461538461538,-0.123076923076923,-0.107692307692308,
-0.0923076923076923,-0.0769230769230769,-0.0615384615384615,-0.0461538461538462,
-0.0307692307692308,-0.0153846153846154,0.),(-1.,1.),.UNSPECIFIED.)
GEOMETRIC_REPRESENTATION_ITEM()
RATIONAL_B_SPLINE_SURFACE(((1.,1.),(1.,1.),(1.,1.),(1.,1.),(1.,1.),(1.,
1.),(1.,1.),(1.,1.),(1.,1.),(1.,1.),(1.,1.),(1.,1.),(1.,1.),(1.,1.),(1.,
1.),(1.,1.),(1.,1.),(1.,1.),(1.,1.),(1.,1.),(1.,1.),(1.,1.),(1.,1.),(1.,
1.),(1.,1.),(1.,1.),(1.,1.),(1.,1.),(1.,1.),(1.,1.),(1.,1.),(1.,1.),(1.,
1.),(1.,1.),(1.,1.),(1.,1.),(1.,1.),(1.,1.),(1.,1.),(1.,1.),(1.,1.),(1.,
1.),(1.,1.),(1.,1.),(1.,1.),(1.,1.),(1.,1.),(1.,1.),(1.,1.),(1.,1.),(1.,
1.),(1.,1.),(1.,1.),(1.,1.),(1.,1.),(1.,1.),(1.,1.),(1.,1.),(1.,1.),(1.,
1.),(1.,1.),(1.,1.),(1.,1.),(1.,1.),(1.,1.),(1.,1.),(1.,1.),(1.,1.),(1.,
1.),(1.,1.)))
REPRESENTATION_ITEM('')
SURFACE()
);
#63=(
BOUNDED_SURFACE()
B_SPLINE_SURFACE(5,1,((#42620,#42621),(#42622,#42623),(#42624,#42625),(#42626,
#42627),(#42628,#42629),(#42630,#42631),(#42632,#42633),(#42634,#42635),
(#42636,#42637),(#42638,#42639),(#42640,#42641),(#42642,#42643),(#42644,
#42645),(#42646,#42647),(#42648,#42649),(#42650,#42651),(#42652,#42653),
(#42654,#42655),(#42656,#42657),(#42658,#42659),(#42660,#42661),(#42662,
#42663),(#42664,#42665),(#42666,#42667),(#42668,#42669),(#42670,#42671),
(#42672,#42673),(#42674,#42675),(#42676,#42677),(#42678,#42679),(#42680,
#42681),(#42682,#42683),(#42684,#42685),(#42686,#42687),(#42688,#42689),
(#42690,#42691),(#42692,#42693),(#42694,#42695),(#42696,#42697),(#42698,
#42699),(#42700,#42701),(#42702,#42703),(#42704,#42705),(#42706,#42707),
(#42708,#42709),(#42710,#42711),(#42712,#42713),(#42714,#42715),(#42716,
#42717),(#42718,#42719),(#42720,#42721),(#42722,#42723),(#42724,#42725),
(#42726,#42727),(#42728,#42729),(#42730,#42731),(#42732,#42733),(#42734,
#42735),(#42736,#42737),(#42738,#42739),(#42740,#42741),(#42742,#42743),
(#42744,#42745),(#42746,#42747),(#42748,#42749),(#42750,#42751),(#42752,
#42753),(#42754,#42755),(#42756,#42757),(#42758,#42759)),.UNSPECIFIED.,
 .F.,.F.,.F.)
B_SPLINE_SURFACE_WITH_KNOTS((6,1,1,1,1,1,1,1,1,1,1,1,1,1,1,1,1,1,1,1,1,
1,1,1,1,1,1,1,1,1,1,1,1,1,1,1,1,1,1,1,1,1,1,1,1,1,1,1,1,1,1,1,1,1,1,1,1,
1,1,1,1,1,1,1,1,6),(2,2),(-1.,-0.984615384615383,-0.969230769230768,-0.953846153846152,
-0.938461538461537,-0.923076923076922,-0.907692307692306,-0.892307692307691,
-0.876923076923076,-0.86153846153846,-0.846153846153845,-0.83076923076923,
-0.815384615384614,-0.799999999999999,-0.784615384615384,-0.769230769230768,
-0.753846153846153,-0.738461538461538,-0.723076923076922,-0.707692307692307,
-0.692307692307692,-0.676923076923076,-0.661538461538461,-0.646153846153846,
-0.63076923076923,-0.615384615384615,-0.6,-0.584615384615384,-0.569230769230769,
-0.553846153846154,-0.538461538461538,-0.523076923076923,-0.507692307692308,
-0.492307692307692,-0.476923076923077,-0.461538461538462,-0.446153846153846,
-0.430769230769231,-0.415384615384615,-0.4,-0.384615384615385,-0.369230769230769,
-0.353846153846154,-0.338461538461538,-0.323076923076923,-0.307692307692308,
-0.292307692307692,-0.276923076923077,-0.261538461538462,-0.246153846153846,
-0.230769230769231,-0.215384615384615,-0.2,-0.184615384615385,-0.169230769230769,
-0.153846153846154,-0.138461538461538,-0.123076923076923,-0.107692307692308,
-0.0923076923076923,-0.0769230769230769,-0.0615384615384615,-0.0461538461538462,
-0.0307692307692308,-0.0153846153846154,0.),(-1.,1.),.UNSPECIFIED.)
GEOMETRIC_REPRESENTATION_ITEM()
RATIONAL_B_SPLINE_SURFACE(((1.,1.),(1.,1.),(1.,1.),(1.,1.),(1.,1.),(1.,
1.),(1.,1.),(1.,1.),(1.,1.),(1.,1.),(1.,1.),(1.,1.),(1.,1.),(1.,1.),(1.,
1.),(1.,1.),(1.,1.),(1.,1.),(1.,1.),(1.,1.),(1.,1.),(1.,1.),(1.,1.),(1.,
1.),(1.,1.),(1.,1.),(1.,1.),(1.,1.),(1.,1.),(1.,1.),(1.,1.),(1.,1.),(1.,
1.),(1.,1.),(1.,1.),(1.,1.),(1.,1.),(1.,1.),(1.,1.),(1.,1.),(1.,1.),(1.,
1.),(1.,1.),(1.,1.),(1.,1.),(1.,1.),(1.,1.),(1.,1.),(1.,1.),(1.,1.),(1.,
1.),(1.,1.),(1.,1.),(1.,1.),(1.,1.),(1.,1.),(1.,1.),(1.,1.),(1.,1.),(1.,
1.),(1.,1.),(1.,1.),(1.,1.),(1.,1.),(1.,1.),(1.,1.),(1.,1.),(1.,1.),(1.,
1.),(1.,1.)))
REPRESENTATION_ITEM('')
SURFACE()
);
#64=(
BOUNDED_SURFACE()
B_SPLINE_SURFACE(5,1,((#42832,#42833),(#42834,#42835),(#42836,#42837),(#42838,
#42839),(#42840,#42841),(#42842,#42843),(#42844,#42845),(#42846,#42847),
(#42848,#42849),(#42850,#42851),(#42852,#42853),(#42854,#42855),(#42856,
#42857),(#42858,#42859),(#42860,#42861),(#42862,#42863),(#42864,#42865),
(#42866,#42867),(#42868,#42869),(#42870,#42871),(#42872,#42873),(#42874,
#42875),(#42876,#42877),(#42878,#42879),(#42880,#42881),(#42882,#42883),
(#42884,#42885),(#42886,#42887),(#42888,#42889),(#42890,#42891),(#42892,
#42893),(#42894,#42895),(#42896,#42897),(#42898,#42899),(#42900,#42901),
(#42902,#42903),(#42904,#42905),(#42906,#42907),(#42908,#42909),(#42910,
#42911),(#42912,#42913),(#42914,#42915),(#42916,#42917),(#42918,#42919),
(#42920,#42921),(#42922,#42923),(#42924,#42925),(#42926,#42927),(#42928,
#42929),(#42930,#42931),(#42932,#42933),(#42934,#42935),(#42936,#42937),
(#42938,#42939),(#42940,#42941),(#42942,#42943),(#42944,#42945),(#42946,
#42947),(#42948,#42949),(#42950,#42951),(#42952,#42953),(#42954,#42955),
(#42956,#42957),(#42958,#42959),(#42960,#42961),(#42962,#42963),(#42964,
#42965),(#42966,#42967),(#42968,#42969),(#42970,#42971)),.UNSPECIFIED.,
 .F.,.F.,.F.)
B_SPLINE_SURFACE_WITH_KNOTS((6,1,1,1,1,1,1,1,1,1,1,1,1,1,1,1,1,1,1,1,1,
1,1,1,1,1,1,1,1,1,1,1,1,1,1,1,1,1,1,1,1,1,1,1,1,1,1,1,1,1,1,1,1,1,1,1,1,
1,1,1,1,1,1,1,1,6),(2,2),(-1.,-0.984615384615383,-0.969230769230768,-0.953846153846152,
-0.938461538461537,-0.923076923076922,-0.907692307692306,-0.892307692307691,
-0.876923076923076,-0.86153846153846,-0.846153846153845,-0.83076923076923,
-0.815384615384614,-0.799999999999999,-0.784615384615384,-0.769230769230768,
-0.753846153846153,-0.738461538461538,-0.723076923076922,-0.707692307692307,
-0.692307692307692,-0.676923076923076,-0.661538461538461,-0.646153846153846,
-0.63076923076923,-0.615384615384615,-0.6,-0.584615384615384,-0.569230769230769,
-0.553846153846154,-0.538461538461538,-0.523076923076923,-0.507692307692308,
-0.492307692307692,-0.476923076923077,-0.461538461538462,-0.446153846153846,
-0.430769230769231,-0.415384615384615,-0.4,-0.384615384615385,-0.369230769230769,
-0.353846153846154,-0.338461538461538,-0.323076923076923,-0.307692307692308,
-0.292307692307692,-0.276923076923077,-0.261538461538462,-0.246153846153846,
-0.230769230769231,-0.215384615384615,-0.2,-0.184615384615385,-0.169230769230769,
-0.153846153846154,-0.138461538461538,-0.123076923076923,-0.107692307692308,
-0.0923076923076923,-0.0769230769230769,-0.0615384615384615,-0.0461538461538462,
-0.0307692307692308,-0.0153846153846154,0.),(-1.,1.),.UNSPECIFIED.)
GEOMETRIC_REPRESENTATION_ITEM()
RATIONAL_B_SPLINE_SURFACE(((1.,1.),(1.,1.),(1.,1.),(1.,1.),(1.,1.),(1.,
1.),(1.,1.),(1.,1.),(1.,1.),(1.,1.),(1.,1.),(1.,1.),(1.,1.),(1.,1.),(1.,
1.),(1.,1.),(1.,1.),(1.,1.),(1.,1.),(1.,1.),(1.,1.),(1.,1.),(1.,1.),(1.,
1.),(1.,1.),(1.,1.),(1.,1.),(1.,1.),(1.,1.),(1.,1.),(1.,1.),(1.,1.),(1.,
1.),(1.,1.),(1.,1.),(1.,1.),(1.,1.),(1.,1.),(1.,1.),(1.,1.),(1.,1.),(1.,
1.),(1.,1.),(1.,1.),(1.,1.),(1.,1.),(1.,1.),(1.,1.),(1.,1.),(1.,1.),(1.,
1.),(1.,1.),(1.,1.),(1.,1.),(1.,1.),(1.,1.),(1.,1.),(1.,1.),(1.,1.),(1.,
1.),(1.,1.),(1.,1.),(1.,1.),(1.,1.),(1.,1.),(1.,1.),(1.,1.),(1.,1.),(1.,
1.),(1.,1.)))
REPRESENTATION_ITEM('')
SURFACE()
);
#65=(
BOUNDED_SURFACE()
B_SPLINE_SURFACE(5,1,((#43062,#43063),(#43064,#43065),(#43066,#43067),(#43068,
#43069),(#43070,#43071),(#43072,#43073),(#43074,#43075),(#43076,#43077),
(#43078,#43079),(#43080,#43081),(#43082,#43083),(#43084,#43085),(#43086,
#43087),(#43088,#43089),(#43090,#43091),(#43092,#43093),(#43094,#43095),
(#43096,#43097),(#43098,#43099),(#43100,#43101),(#43102,#43103),(#43104,
#43105),(#43106,#43107),(#43108,#43109),(#43110,#43111),(#43112,#43113),
(#43114,#43115),(#43116,#43117),(#43118,#43119),(#43120,#43121),(#43122,
#43123),(#43124,#43125),(#43126,#43127),(#43128,#43129),(#43130,#43131),
(#43132,#43133),(#43134,#43135),(#43136,#43137),(#43138,#43139),(#43140,
#43141),(#43142,#43143),(#43144,#43145),(#43146,#43147),(#43148,#43149),
(#43150,#43151),(#43152,#43153),(#43154,#43155),(#43156,#43157),(#43158,
#43159),(#43160,#43161),(#43162,#43163),(#43164,#43165),(#43166,#43167),
(#43168,#43169),(#43170,#43171),(#43172,#43173),(#43174,#43175),(#43176,
#43177),(#43178,#43179),(#43180,#43181),(#43182,#43183),(#43184,#43185),
(#43186,#43187),(#43188,#43189),(#43190,#43191),(#43192,#43193),(#43194,
#43195),(#43196,#43197),(#43198,#43199),(#43200,#43201)),.UNSPECIFIED.,
 .F.,.F.,.F.)
B_SPLINE_SURFACE_WITH_KNOTS((6,1,1,1,1,1,1,1,1,1,1,1,1,1,1,1,1,1,1,1,1,
1,1,1,1,1,1,1,1,1,1,1,1,1,1,1,1,1,1,1,1,1,1,1,1,1,1,1,1,1,1,1,1,1,1,1,1,
1,1,1,1,1,1,1,1,6),(2,2),(-1.,-0.984615384615383,-0.969230769230768,-0.953846153846152,
-0.938461538461537,-0.923076923076922,-0.907692307692306,-0.892307692307691,
-0.876923076923076,-0.86153846153846,-0.846153846153845,-0.83076923076923,
-0.815384615384614,-0.799999999999999,-0.784615384615384,-0.769230769230768,
-0.753846153846153,-0.738461538461538,-0.723076923076922,-0.707692307692307,
-0.692307692307692,-0.676923076923076,-0.661538461538461,-0.646153846153846,
-0.63076923076923,-0.615384615384615,-0.6,-0.584615384615384,-0.569230769230769,
-0.553846153846154,-0.538461538461538,-0.523076923076923,-0.507692307692308,
-0.492307692307692,-0.476923076923077,-0.461538461538462,-0.446153846153846,
-0.430769230769231,-0.415384615384615,-0.4,-0.384615384615385,-0.369230769230769,
-0.353846153846154,-0.338461538461538,-0.323076923076923,-0.307692307692308,
-0.292307692307692,-0.276923076923077,-0.261538461538462,-0.246153846153846,
-0.230769230769231,-0.215384615384615,-0.2,-0.184615384615385,-0.169230769230769,
-0.153846153846154,-0.138461538461538,-0.123076923076923,-0.107692307692308,
-0.0923076923076923,-0.0769230769230769,-0.0615384615384615,-0.0461538461538462,
-0.0307692307692308,-0.0153846153846154,0.),(-1.,1.),.UNSPECIFIED.)
GEOMETRIC_REPRESENTATION_ITEM()
RATIONAL_B_SPLINE_SURFACE(((1.,1.),(1.,1.),(1.,1.),(1.,1.),(1.,1.),(1.,
1.),(1.,1.),(1.,1.),(1.,1.),(1.,1.),(1.,1.),(1.,1.),(1.,1.),(1.,1.),(1.,
1.),(1.,1.),(1.,1.),(1.,1.),(1.,1.),(1.,1.),(1.,1.),(1.,1.),(1.,1.),(1.,
1.),(1.,1.),(1.,1.),(1.,1.),(1.,1.),(1.,1.),(1.,1.),(1.,1.),(1.,1.),(1.,
1.),(1.,1.),(1.,1.),(1.,1.),(1.,1.),(1.,1.),(1.,1.),(1.,1.),(1.,1.),(1.,
1.),(1.,1.),(1.,1.),(1.,1.),(1.,1.),(1.,1.),(1.,1.),(1.,1.),(1.,1.),(1.,
1.),(1.,1.),(1.,1.),(1.,1.),(1.,1.),(1.,1.),(1.,1.),(1.,1.),(1.,1.),(1.,
1.),(1.,1.),(1.,1.),(1.,1.),(1.,1.),(1.,1.),(1.,1.),(1.,1.),(1.,1.),(1.,
1.),(1.,1.)))
REPRESENTATION_ITEM('')
SURFACE()
);
#66=(
BOUNDED_SURFACE()
B_SPLINE_SURFACE(5,1,((#43274,#43275),(#43276,#43277),(#43278,#43279),(#43280,
#43281),(#43282,#43283),(#43284,#43285),(#43286,#43287),(#43288,#43289),
(#43290,#43291),(#43292,#43293),(#43294,#43295),(#43296,#43297),(#43298,
#43299),(#43300,#43301),(#43302,#43303),(#43304,#43305),(#43306,#43307),
(#43308,#43309),(#43310,#43311),(#43312,#43313),(#43314,#43315),(#43316,
#43317),(#43318,#43319),(#43320,#43321),(#43322,#43323),(#43324,#43325),
(#43326,#43327),(#43328,#43329),(#43330,#43331),(#43332,#43333),(#43334,
#43335),(#43336,#43337),(#43338,#43339),(#43340,#43341),(#43342,#43343),
(#43344,#43345),(#43346,#43347),(#43348,#43349),(#43350,#43351),(#43352,
#43353),(#43354,#43355),(#43356,#43357),(#43358,#43359),(#43360,#43361),
(#43362,#43363),(#43364,#43365),(#43366,#43367),(#43368,#43369),(#43370,
#43371),(#43372,#43373),(#43374,#43375),(#43376,#43377),(#43378,#43379),
(#43380,#43381),(#43382,#43383),(#43384,#43385),(#43386,#43387),(#43388,
#43389),(#43390,#43391),(#43392,#43393),(#43394,#43395),(#43396,#43397),
(#43398,#43399),(#43400,#43401),(#43402,#43403),(#43404,#43405),(#43406,
#43407),(#43408,#43409),(#43410,#43411),(#43412,#43413)),.UNSPECIFIED.,
 .F.,.F.,.F.)
B_SPLINE_SURFACE_WITH_KNOTS((6,1,1,1,1,1,1,1,1,1,1,1,1,1,1,1,1,1,1,1,1,
1,1,1,1,1,1,1,1,1,1,1,1,1,1,1,1,1,1,1,1,1,1,1,1,1,1,1,1,1,1,1,1,1,1,1,1,
1,1,1,1,1,1,1,1,6),(2,2),(-1.,-0.984615384615383,-0.969230769230768,-0.953846153846152,
-0.938461538461537,-0.923076923076922,-0.907692307692306,-0.892307692307691,
-0.876923076923076,-0.86153846153846,-0.846153846153845,-0.83076923076923,
-0.815384615384614,-0.799999999999999,-0.784615384615384,-0.769230769230768,
-0.753846153846153,-0.738461538461538,-0.723076923076922,-0.707692307692307,
-0.692307692307692,-0.676923076923076,-0.661538461538461,-0.646153846153846,
-0.63076923076923,-0.615384615384615,-0.6,-0.584615384615384,-0.569230769230769,
-0.553846153846154,-0.538461538461538,-0.523076923076923,-0.507692307692308,
-0.492307692307692,-0.476923076923077,-0.461538461538462,-0.446153846153846,
-0.430769230769231,-0.415384615384615,-0.4,-0.384615384615385,-0.369230769230769,
-0.353846153846154,-0.338461538461538,-0.323076923076923,-0.307692307692308,
-0.292307692307692,-0.276923076923077,-0.261538461538462,-0.246153846153846,
-0.230769230769231,-0.215384615384615,-0.2,-0.184615384615385,-0.169230769230769,
-0.153846153846154,-0.138461538461538,-0.123076923076923,-0.107692307692308,
-0.0923076923076923,-0.0769230769230769,-0.0615384615384615,-0.0461538461538462,
-0.0307692307692308,-0.0153846153846154,0.),(-1.,1.),.UNSPECIFIED.)
GEOMETRIC_REPRESENTATION_ITEM()
RATIONAL_B_SPLINE_SURFACE(((1.,1.),(1.,1.),(1.,1.),(1.,1.),(1.,1.),(1.,
1.),(1.,1.),(1.,1.),(1.,1.),(1.,1.),(1.,1.),(1.,1.),(1.,1.),(1.,1.),(1.,
1.),(1.,1.),(1.,1.),(1.,1.),(1.,1.),(1.,1.),(1.,1.),(1.,1.),(1.,1.),(1.,
1.),(1.,1.),(1.,1.),(1.,1.),(1.,1.),(1.,1.),(1.,1.),(1.,1.),(1.,1.),(1.,
1.),(1.,1.),(1.,1.),(1.,1.),(1.,1.),(1.,1.),(1.,1.),(1.,1.),(1.,1.),(1.,
1.),(1.,1.),(1.,1.),(1.,1.),(1.,1.),(1.,1.),(1.,1.),(1.,1.),(1.,1.),(1.,
1.),(1.,1.),(1.,1.),(1.,1.),(1.,1.),(1.,1.),(1.,1.),(1.,1.),(1.,1.),(1.,
1.),(1.,1.),(1.,1.),(1.,1.),(1.,1.),(1.,1.),(1.,1.),(1.,1.),(1.,1.),(1.,
1.),(1.,1.)))
REPRESENTATION_ITEM('')
SURFACE()
);
#67=(
BOUNDED_SURFACE()
B_SPLINE_SURFACE(5,1,((#43504,#43505),(#43506,#43507),(#43508,#43509),(#43510,
#43511),(#43512,#43513),(#43514,#43515),(#43516,#43517),(#43518,#43519),
(#43520,#43521),(#43522,#43523),(#43524,#43525),(#43526,#43527),(#43528,
#43529),(#43530,#43531),(#43532,#43533),(#43534,#43535),(#43536,#43537),
(#43538,#43539),(#43540,#43541),(#43542,#43543),(#43544,#43545),(#43546,
#43547),(#43548,#43549),(#43550,#43551),(#43552,#43553),(#43554,#43555),
(#43556,#43557),(#43558,#43559),(#43560,#43561),(#43562,#43563),(#43564,
#43565),(#43566,#43567),(#43568,#43569),(#43570,#43571),(#43572,#43573),
(#43574,#43575),(#43576,#43577),(#43578,#43579),(#43580,#43581),(#43582,
#43583),(#43584,#43585),(#43586,#43587),(#43588,#43589),(#43590,#43591),
(#43592,#43593),(#43594,#43595),(#43596,#43597),(#43598,#43599),(#43600,
#43601),(#43602,#43603),(#43604,#43605),(#43606,#43607),(#43608,#43609),
(#43610,#43611),(#43612,#43613),(#43614,#43615),(#43616,#43617),(#43618,
#43619),(#43620,#43621),(#43622,#43623),(#43624,#43625),(#43626,#43627),
(#43628,#43629),(#43630,#43631),(#43632,#43633),(#43634,#43635),(#43636,
#43637),(#43638,#43639),(#43640,#43641),(#43642,#43643)),.UNSPECIFIED.,
 .F.,.F.,.F.)
B_SPLINE_SURFACE_WITH_KNOTS((6,1,1,1,1,1,1,1,1,1,1,1,1,1,1,1,1,1,1,1,1,
1,1,1,1,1,1,1,1,1,1,1,1,1,1,1,1,1,1,1,1,1,1,1,1,1,1,1,1,1,1,1,1,1,1,1,1,
1,1,1,1,1,1,1,1,6),(2,2),(-1.,-0.984615384615383,-0.969230769230768,-0.953846153846152,
-0.938461538461537,-0.923076923076922,-0.907692307692306,-0.892307692307691,
-0.876923076923076,-0.86153846153846,-0.846153846153845,-0.83076923076923,
-0.815384615384614,-0.799999999999999,-0.784615384615384,-0.769230769230768,
-0.753846153846153,-0.738461538461538,-0.723076923076922,-0.707692307692307,
-0.692307692307692,-0.676923076923076,-0.661538461538461,-0.646153846153846,
-0.63076923076923,-0.615384615384615,-0.6,-0.584615384615384,-0.569230769230769,
-0.553846153846154,-0.538461538461538,-0.523076923076923,-0.507692307692308,
-0.492307692307692,-0.476923076923077,-0.461538461538462,-0.446153846153846,
-0.430769230769231,-0.415384615384615,-0.4,-0.384615384615385,-0.369230769230769,
-0.353846153846154,-0.338461538461538,-0.323076923076923,-0.307692307692308,
-0.292307692307692,-0.276923076923077,-0.261538461538462,-0.246153846153846,
-0.230769230769231,-0.215384615384615,-0.2,-0.184615384615385,-0.169230769230769,
-0.153846153846154,-0.138461538461538,-0.123076923076923,-0.107692307692308,
-0.0923076923076923,-0.0769230769230769,-0.0615384615384615,-0.0461538461538462,
-0.0307692307692308,-0.0153846153846154,0.),(-1.,1.),.UNSPECIFIED.)
GEOMETRIC_REPRESENTATION_ITEM()
RATIONAL_B_SPLINE_SURFACE(((1.,1.),(1.,1.),(1.,1.),(1.,1.),(1.,1.),(1.,
1.),(1.,1.),(1.,1.),(1.,1.),(1.,1.),(1.,1.),(1.,1.),(1.,1.),(1.,1.),(1.,
1.),(1.,1.),(1.,1.),(1.,1.),(1.,1.),(1.,1.),(1.,1.),(1.,1.),(1.,1.),(1.,
1.),(1.,1.),(1.,1.),(1.,1.),(1.,1.),(1.,1.),(1.,1.),(1.,1.),(1.,1.),(1.,
1.),(1.,1.),(1.,1.),(1.,1.),(1.,1.),(1.,1.),(1.,1.),(1.,1.),(1.,1.),(1.,
1.),(1.,1.),(1.,1.),(1.,1.),(1.,1.),(1.,1.),(1.,1.),(1.,1.),(1.,1.),(1.,
1.),(1.,1.),(1.,1.),(1.,1.),(1.,1.),(1.,1.),(1.,1.),(1.,1.),(1.,1.),(1.,
1.),(1.,1.),(1.,1.),(1.,1.),(1.,1.),(1.,1.),(1.,1.),(1.,1.),(1.,1.),(1.,
1.),(1.,1.)))
REPRESENTATION_ITEM('')
SURFACE()
);
#68=(
BOUNDED_SURFACE()
B_SPLINE_SURFACE(5,1,((#43716,#43717),(#43718,#43719),(#43720,#43721),(#43722,
#43723),(#43724,#43725),(#43726,#43727),(#43728,#43729),(#43730,#43731),
(#43732,#43733),(#43734,#43735),(#43736,#43737),(#43738,#43739),(#43740,
#43741),(#43742,#43743),(#43744,#43745),(#43746,#43747),(#43748,#43749),
(#43750,#43751),(#43752,#43753),(#43754,#43755),(#43756,#43757),(#43758,
#43759),(#43760,#43761),(#43762,#43763),(#43764,#43765),(#43766,#43767),
(#43768,#43769),(#43770,#43771),(#43772,#43773),(#43774,#43775),(#43776,
#43777),(#43778,#43779),(#43780,#43781),(#43782,#43783),(#43784,#43785),
(#43786,#43787),(#43788,#43789),(#43790,#43791),(#43792,#43793),(#43794,
#43795),(#43796,#43797),(#43798,#43799),(#43800,#43801),(#43802,#43803),
(#43804,#43805),(#43806,#43807),(#43808,#43809),(#43810,#43811),(#43812,
#43813),(#43814,#43815),(#43816,#43817),(#43818,#43819),(#43820,#43821),
(#43822,#43823),(#43824,#43825),(#43826,#43827),(#43828,#43829),(#43830,
#43831),(#43832,#43833),(#43834,#43835),(#43836,#43837),(#43838,#43839),
(#43840,#43841),(#43842,#43843),(#43844,#43845),(#43846,#43847),(#43848,
#43849),(#43850,#43851),(#43852,#43853),(#43854,#43855)),.UNSPECIFIED.,
 .F.,.F.,.F.)
B_SPLINE_SURFACE_WITH_KNOTS((6,1,1,1,1,1,1,1,1,1,1,1,1,1,1,1,1,1,1,1,1,
1,1,1,1,1,1,1,1,1,1,1,1,1,1,1,1,1,1,1,1,1,1,1,1,1,1,1,1,1,1,1,1,1,1,1,1,
1,1,1,1,1,1,1,1,6),(2,2),(-1.,-0.984615384615383,-0.969230769230768,-0.953846153846152,
-0.938461538461537,-0.923076923076922,-0.907692307692306,-0.892307692307691,
-0.876923076923076,-0.86153846153846,-0.846153846153845,-0.83076923076923,
-0.815384615384614,-0.799999999999999,-0.784615384615384,-0.769230769230768,
-0.753846153846153,-0.738461538461538,-0.723076923076922,-0.707692307692307,
-0.692307692307692,-0.676923076923076,-0.661538461538461,-0.646153846153846,
-0.63076923076923,-0.615384615384615,-0.6,-0.584615384615384,-0.569230769230769,
-0.553846153846154,-0.538461538461538,-0.523076923076923,-0.507692307692308,
-0.492307692307692,-0.476923076923077,-0.461538461538462,-0.446153846153846,
-0.430769230769231,-0.415384615384615,-0.4,-0.384615384615385,-0.369230769230769,
-0.353846153846154,-0.338461538461538,-0.323076923076923,-0.307692307692308,
-0.292307692307692,-0.276923076923077,-0.261538461538462,-0.246153846153846,
-0.230769230769231,-0.215384615384615,-0.2,-0.184615384615385,-0.169230769230769,
-0.153846153846154,-0.138461538461538,-0.123076923076923,-0.107692307692308,
-0.0923076923076923,-0.0769230769230769,-0.0615384615384615,-0.0461538461538462,
-0.0307692307692308,-0.0153846153846154,0.),(-1.,1.),.UNSPECIFIED.)
GEOMETRIC_REPRESENTATION_ITEM()
RATIONAL_B_SPLINE_SURFACE(((1.,1.),(1.,1.),(1.,1.),(1.,1.),(1.,1.),(1.,
1.),(1.,1.),(1.,1.),(1.,1.),(1.,1.),(1.,1.),(1.,1.),(1.,1.),(1.,1.),(1.,
1.),(1.,1.),(1.,1.),(1.,1.),(1.,1.),(1.,1.),(1.,1.),(1.,1.),(1.,1.),(1.,
1.),(1.,1.),(1.,1.),(1.,1.),(1.,1.),(1.,1.),(1.,1.),(1.,1.),(1.,1.),(1.,
1.),(1.,1.),(1.,1.),(1.,1.),(1.,1.),(1.,1.),(1.,1.),(1.,1.),(1.,1.),(1.,
1.),(1.,1.),(1.,1.),(1.,1.),(1.,1.),(1.,1.),(1.,1.),(1.,1.),(1.,1.),(1.,
1.),(1.,1.),(1.,1.),(1.,1.),(1.,1.),(1.,1.),(1.,1.),(1.,1.),(1.,1.),(1.,
1.),(1.,1.),(1.,1.),(1.,1.),(1.,1.),(1.,1.),(1.,1.),(1.,1.),(1.,1.),(1.,
1.),(1.,1.)))
REPRESENTATION_ITEM('')
SURFACE()
);
#69=(
BOUNDED_SURFACE()
B_SPLINE_SURFACE(5,1,((#43946,#43947),(#43948,#43949),(#43950,#43951),(#43952,
#43953),(#43954,#43955),(#43956,#43957),(#43958,#43959),(#43960,#43961),
(#43962,#43963),(#43964,#43965),(#43966,#43967),(#43968,#43969),(#43970,
#43971),(#43972,#43973),(#43974,#43975),(#43976,#43977),(#43978,#43979),
(#43980,#43981),(#43982,#43983),(#43984,#43985),(#43986,#43987),(#43988,
#43989),(#43990,#43991),(#43992,#43993),(#43994,#43995),(#43996,#43997),
(#43998,#43999),(#44000,#44001),(#44002,#44003),(#44004,#44005),(#44006,
#44007),(#44008,#44009),(#44010,#44011),(#44012,#44013),(#44014,#44015),
(#44016,#44017),(#44018,#44019),(#44020,#44021),(#44022,#44023),(#44024,
#44025),(#44026,#44027),(#44028,#44029),(#44030,#44031),(#44032,#44033),
(#44034,#44035),(#44036,#44037),(#44038,#44039),(#44040,#44041),(#44042,
#44043),(#44044,#44045),(#44046,#44047),(#44048,#44049),(#44050,#44051),
(#44052,#44053),(#44054,#44055),(#44056,#44057),(#44058,#44059),(#44060,
#44061),(#44062,#44063),(#44064,#44065),(#44066,#44067),(#44068,#44069),
(#44070,#44071),(#44072,#44073),(#44074,#44075),(#44076,#44077),(#44078,
#44079),(#44080,#44081),(#44082,#44083),(#44084,#44085)),.UNSPECIFIED.,
 .F.,.F.,.F.)
B_SPLINE_SURFACE_WITH_KNOTS((6,1,1,1,1,1,1,1,1,1,1,1,1,1,1,1,1,1,1,1,1,
1,1,1,1,1,1,1,1,1,1,1,1,1,1,1,1,1,1,1,1,1,1,1,1,1,1,1,1,1,1,1,1,1,1,1,1,
1,1,1,1,1,1,1,1,6),(2,2),(-1.,-0.984615384615383,-0.969230769230768,-0.953846153846152,
-0.938461538461537,-0.923076923076922,-0.907692307692306,-0.892307692307691,
-0.876923076923076,-0.86153846153846,-0.846153846153845,-0.83076923076923,
-0.815384615384614,-0.799999999999999,-0.784615384615384,-0.769230769230768,
-0.753846153846153,-0.738461538461538,-0.723076923076922,-0.707692307692307,
-0.692307692307692,-0.676923076923076,-0.661538461538461,-0.646153846153846,
-0.63076923076923,-0.615384615384615,-0.6,-0.584615384615384,-0.569230769230769,
-0.553846153846154,-0.538461538461538,-0.523076923076923,-0.507692307692308,
-0.492307692307692,-0.476923076923077,-0.461538461538462,-0.446153846153846,
-0.430769230769231,-0.415384615384615,-0.4,-0.384615384615385,-0.369230769230769,
-0.353846153846154,-0.338461538461538,-0.323076923076923,-0.307692307692308,
-0.292307692307692,-0.276923076923077,-0.261538461538462,-0.246153846153846,
-0.230769230769231,-0.215384615384615,-0.2,-0.184615384615385,-0.169230769230769,
-0.153846153846154,-0.138461538461538,-0.123076923076923,-0.107692307692308,
-0.0923076923076923,-0.0769230769230769,-0.0615384615384615,-0.0461538461538462,
-0.0307692307692308,-0.0153846153846154,0.),(-1.,1.),.UNSPECIFIED.)
GEOMETRIC_REPRESENTATION_ITEM()
RATIONAL_B_SPLINE_SURFACE(((1.,1.),(1.,1.),(1.,1.),(1.,1.),(1.,1.),(1.,
1.),(1.,1.),(1.,1.),(1.,1.),(1.,1.),(1.,1.),(1.,1.),(1.,1.),(1.,1.),(1.,
1.),(1.,1.),(1.,1.),(1.,1.),(1.,1.),(1.,1.),(1.,1.),(1.,1.),(1.,1.),(1.,
1.),(1.,1.),(1.,1.),(1.,1.),(1.,1.),(1.,1.),(1.,1.),(1.,1.),(1.,1.),(1.,
1.),(1.,1.),(1.,1.),(1.,1.),(1.,1.),(1.,1.),(1.,1.),(1.,1.),(1.,1.),(1.,
1.),(1.,1.),(1.,1.),(1.,1.),(1.,1.),(1.,1.),(1.,1.),(1.,1.),(1.,1.),(1.,
1.),(1.,1.),(1.,1.),(1.,1.),(1.,1.),(1.,1.),(1.,1.),(1.,1.),(1.,1.),(1.,
1.),(1.,1.),(1.,1.),(1.,1.),(1.,1.),(1.,1.),(1.,1.),(1.,1.),(1.,1.),(1.,
1.),(1.,1.)))
REPRESENTATION_ITEM('')
SURFACE()
);
#70=(
BOUNDED_SURFACE()
B_SPLINE_SURFACE(5,1,((#44158,#44159),(#44160,#44161),(#44162,#44163),(#44164,
#44165),(#44166,#44167),(#44168,#44169),(#44170,#44171),(#44172,#44173),
(#44174,#44175),(#44176,#44177),(#44178,#44179),(#44180,#44181),(#44182,
#44183),(#44184,#44185),(#44186,#44187),(#44188,#44189),(#44190,#44191),
(#44192,#44193),(#44194,#44195),(#44196,#44197),(#44198,#44199),(#44200,
#44201),(#44202,#44203),(#44204,#44205),(#44206,#44207),(#44208,#44209),
(#44210,#44211),(#44212,#44213),(#44214,#44215),(#44216,#44217),(#44218,
#44219),(#44220,#44221),(#44222,#44223),(#44224,#44225),(#44226,#44227),
(#44228,#44229),(#44230,#44231),(#44232,#44233),(#44234,#44235),(#44236,
#44237),(#44238,#44239),(#44240,#44241),(#44242,#44243),(#44244,#44245),
(#44246,#44247),(#44248,#44249),(#44250,#44251),(#44252,#44253),(#44254,
#44255),(#44256,#44257),(#44258,#44259),(#44260,#44261),(#44262,#44263),
(#44264,#44265),(#44266,#44267),(#44268,#44269),(#44270,#44271),(#44272,
#44273),(#44274,#44275),(#44276,#44277),(#44278,#44279),(#44280,#44281),
(#44282,#44283),(#44284,#44285),(#44286,#44287),(#44288,#44289),(#44290,
#44291),(#44292,#44293),(#44294,#44295),(#44296,#44297)),.UNSPECIFIED.,
 .F.,.F.,.F.)
B_SPLINE_SURFACE_WITH_KNOTS((6,1,1,1,1,1,1,1,1,1,1,1,1,1,1,1,1,1,1,1,1,
1,1,1,1,1,1,1,1,1,1,1,1,1,1,1,1,1,1,1,1,1,1,1,1,1,1,1,1,1,1,1,1,1,1,1,1,
1,1,1,1,1,1,1,1,6),(2,2),(-1.,-0.984615384615383,-0.969230769230768,-0.953846153846152,
-0.938461538461537,-0.923076923076922,-0.907692307692306,-0.892307692307691,
-0.876923076923076,-0.86153846153846,-0.846153846153845,-0.83076923076923,
-0.815384615384614,-0.799999999999999,-0.784615384615384,-0.769230769230768,
-0.753846153846153,-0.738461538461538,-0.723076923076922,-0.707692307692307,
-0.692307692307692,-0.676923076923076,-0.661538461538461,-0.646153846153846,
-0.63076923076923,-0.615384615384615,-0.6,-0.584615384615384,-0.569230769230769,
-0.553846153846154,-0.538461538461538,-0.523076923076923,-0.507692307692308,
-0.492307692307692,-0.476923076923077,-0.461538461538462,-0.446153846153846,
-0.430769230769231,-0.415384615384615,-0.4,-0.384615384615385,-0.369230769230769,
-0.353846153846154,-0.338461538461538,-0.323076923076923,-0.307692307692308,
-0.292307692307692,-0.276923076923077,-0.261538461538462,-0.246153846153846,
-0.230769230769231,-0.215384615384615,-0.2,-0.184615384615385,-0.169230769230769,
-0.153846153846154,-0.138461538461538,-0.123076923076923,-0.107692307692308,
-0.0923076923076923,-0.0769230769230769,-0.0615384615384615,-0.0461538461538462,
-0.0307692307692308,-0.0153846153846154,0.),(-1.,1.),.UNSPECIFIED.)
GEOMETRIC_REPRESENTATION_ITEM()
RATIONAL_B_SPLINE_SURFACE(((1.,1.),(1.,1.),(1.,1.),(1.,1.),(1.,1.),(1.,
1.),(1.,1.),(1.,1.),(1.,1.),(1.,1.),(1.,1.),(1.,1.),(1.,1.),(1.,1.),(1.,
1.),(1.,1.),(1.,1.),(1.,1.),(1.,1.),(1.,1.),(1.,1.),(1.,1.),(1.,1.),(1.,
1.),(1.,1.),(1.,1.),(1.,1.),(1.,1.),(1.,1.),(1.,1.),(1.,1.),(1.,1.),(1.,
1.),(1.,1.),(1.,1.),(1.,1.),(1.,1.),(1.,1.),(1.,1.),(1.,1.),(1.,1.),(1.,
1.),(1.,1.),(1.,1.),(1.,1.),(1.,1.),(1.,1.),(1.,1.),(1.,1.),(1.,1.),(1.,
1.),(1.,1.),(1.,1.),(1.,1.),(1.,1.),(1.,1.),(1.,1.),(1.,1.),(1.,1.),(1.,
1.),(1.,1.),(1.,1.),(1.,1.),(1.,1.),(1.,1.),(1.,1.),(1.,1.),(1.,1.),(1.,
1.),(1.,1.)))
REPRESENTATION_ITEM('')
SURFACE()
);
#71=(
BOUNDED_SURFACE()
B_SPLINE_SURFACE(5,1,((#44388,#44389),(#44390,#44391),(#44392,#44393),(#44394,
#44395),(#44396,#44397),(#44398,#44399),(#44400,#44401),(#44402,#44403),
(#44404,#44405),(#44406,#44407),(#44408,#44409),(#44410,#44411),(#44412,
#44413),(#44414,#44415),(#44416,#44417),(#44418,#44419),(#44420,#44421),
(#44422,#44423),(#44424,#44425),(#44426,#44427),(#44428,#44429),(#44430,
#44431),(#44432,#44433),(#44434,#44435),(#44436,#44437),(#44438,#44439),
(#44440,#44441),(#44442,#44443),(#44444,#44445),(#44446,#44447),(#44448,
#44449),(#44450,#44451),(#44452,#44453),(#44454,#44455),(#44456,#44457),
(#44458,#44459),(#44460,#44461),(#44462,#44463),(#44464,#44465),(#44466,
#44467),(#44468,#44469),(#44470,#44471),(#44472,#44473),(#44474,#44475),
(#44476,#44477),(#44478,#44479),(#44480,#44481),(#44482,#44483),(#44484,
#44485),(#44486,#44487),(#44488,#44489),(#44490,#44491),(#44492,#44493),
(#44494,#44495),(#44496,#44497),(#44498,#44499),(#44500,#44501),(#44502,
#44503),(#44504,#44505),(#44506,#44507),(#44508,#44509),(#44510,#44511),
(#44512,#44513),(#44514,#44515),(#44516,#44517),(#44518,#44519),(#44520,
#44521),(#44522,#44523),(#44524,#44525),(#44526,#44527)),.UNSPECIFIED.,
 .F.,.F.,.F.)
B_SPLINE_SURFACE_WITH_KNOTS((6,1,1,1,1,1,1,1,1,1,1,1,1,1,1,1,1,1,1,1,1,
1,1,1,1,1,1,1,1,1,1,1,1,1,1,1,1,1,1,1,1,1,1,1,1,1,1,1,1,1,1,1,1,1,1,1,1,
1,1,1,1,1,1,1,1,6),(2,2),(-1.,-0.984615384615383,-0.969230769230768,-0.953846153846152,
-0.938461538461537,-0.923076923076922,-0.907692307692306,-0.892307692307691,
-0.876923076923076,-0.86153846153846,-0.846153846153845,-0.83076923076923,
-0.815384615384614,-0.799999999999999,-0.784615384615384,-0.769230769230768,
-0.753846153846153,-0.738461538461538,-0.723076923076922,-0.707692307692307,
-0.692307692307692,-0.676923076923076,-0.661538461538461,-0.646153846153846,
-0.63076923076923,-0.615384615384615,-0.6,-0.584615384615384,-0.569230769230769,
-0.553846153846154,-0.538461538461538,-0.523076923076923,-0.507692307692308,
-0.492307692307692,-0.476923076923077,-0.461538461538462,-0.446153846153846,
-0.430769230769231,-0.415384615384615,-0.4,-0.384615384615385,-0.369230769230769,
-0.353846153846154,-0.338461538461538,-0.323076923076923,-0.307692307692308,
-0.292307692307692,-0.276923076923077,-0.261538461538462,-0.246153846153846,
-0.230769230769231,-0.215384615384615,-0.2,-0.184615384615385,-0.169230769230769,
-0.153846153846154,-0.138461538461538,-0.123076923076923,-0.107692307692308,
-0.0923076923076923,-0.0769230769230769,-0.0615384615384615,-0.0461538461538462,
-0.0307692307692308,-0.0153846153846154,0.),(-1.,1.),.UNSPECIFIED.)
GEOMETRIC_REPRESENTATION_ITEM()
RATIONAL_B_SPLINE_SURFACE(((1.,1.),(1.,1.),(1.,1.),(1.,1.),(1.,1.),(1.,
1.),(1.,1.),(1.,1.),(1.,1.),(1.,1.),(1.,1.),(1.,1.),(1.,1.),(1.,1.),(1.,
1.),(1.,1.),(1.,1.),(1.,1.),(1.,1.),(1.,1.),(1.,1.),(1.,1.),(1.,1.),(1.,
1.),(1.,1.),(1.,1.),(1.,1.),(1.,1.),(1.,1.),(1.,1.),(1.,1.),(1.,1.),(1.,
1.),(1.,1.),(1.,1.),(1.,1.),(1.,1.),(1.,1.),(1.,1.),(1.,1.),(1.,1.),(1.,
1.),(1.,1.),(1.,1.),(1.,1.),(1.,1.),(1.,1.),(1.,1.),(1.,1.),(1.,1.),(1.,
1.),(1.,1.),(1.,1.),(1.,1.),(1.,1.),(1.,1.),(1.,1.),(1.,1.),(1.,1.),(1.,
1.),(1.,1.),(1.,1.),(1.,1.),(1.,1.),(1.,1.),(1.,1.),(1.,1.),(1.,1.),(1.,
1.),(1.,1.)))
REPRESENTATION_ITEM('')
SURFACE()
);
#72=(
BOUNDED_SURFACE()
B_SPLINE_SURFACE(5,1,((#44600,#44601),(#44602,#44603),(#44604,#44605),(#44606,
#44607),(#44608,#44609),(#44610,#44611),(#44612,#44613),(#44614,#44615),
(#44616,#44617),(#44618,#44619),(#44620,#44621),(#44622,#44623),(#44624,
#44625),(#44626,#44627),(#44628,#44629),(#44630,#44631),(#44632,#44633),
(#44634,#44635),(#44636,#44637),(#44638,#44639),(#44640,#44641),(#44642,
#44643),(#44644,#44645),(#44646,#44647),(#44648,#44649),(#44650,#44651),
(#44652,#44653),(#44654,#44655),(#44656,#44657),(#44658,#44659),(#44660,
#44661),(#44662,#44663),(#44664,#44665),(#44666,#44667),(#44668,#44669),
(#44670,#44671),(#44672,#44673),(#44674,#44675),(#44676,#44677),(#44678,
#44679),(#44680,#44681),(#44682,#44683),(#44684,#44685),(#44686,#44687),
(#44688,#44689),(#44690,#44691),(#44692,#44693),(#44694,#44695),(#44696,
#44697),(#44698,#44699),(#44700,#44701),(#44702,#44703),(#44704,#44705),
(#44706,#44707),(#44708,#44709),(#44710,#44711),(#44712,#44713),(#44714,
#44715),(#44716,#44717),(#44718,#44719),(#44720,#44721),(#44722,#44723),
(#44724,#44725),(#44726,#44727),(#44728,#44729),(#44730,#44731),(#44732,
#44733),(#44734,#44735),(#44736,#44737),(#44738,#44739)),.UNSPECIFIED.,
 .F.,.F.,.F.)
B_SPLINE_SURFACE_WITH_KNOTS((6,1,1,1,1,1,1,1,1,1,1,1,1,1,1,1,1,1,1,1,1,
1,1,1,1,1,1,1,1,1,1,1,1,1,1,1,1,1,1,1,1,1,1,1,1,1,1,1,1,1,1,1,1,1,1,1,1,
1,1,1,1,1,1,1,1,6),(2,2),(-1.,-0.984615384615383,-0.969230769230768,-0.953846153846152,
-0.938461538461537,-0.923076923076922,-0.907692307692306,-0.892307692307691,
-0.876923076923076,-0.86153846153846,-0.846153846153845,-0.83076923076923,
-0.815384615384614,-0.799999999999999,-0.784615384615384,-0.769230769230768,
-0.753846153846153,-0.738461538461538,-0.723076923076922,-0.707692307692307,
-0.692307692307692,-0.676923076923076,-0.661538461538461,-0.646153846153846,
-0.63076923076923,-0.615384615384615,-0.6,-0.584615384615384,-0.569230769230769,
-0.553846153846154,-0.538461538461538,-0.523076923076923,-0.507692307692308,
-0.492307692307692,-0.476923076923077,-0.461538461538462,-0.446153846153846,
-0.430769230769231,-0.415384615384615,-0.4,-0.384615384615385,-0.369230769230769,
-0.353846153846154,-0.338461538461538,-0.323076923076923,-0.307692307692308,
-0.292307692307692,-0.276923076923077,-0.261538461538462,-0.246153846153846,
-0.230769230769231,-0.215384615384615,-0.2,-0.184615384615385,-0.169230769230769,
-0.153846153846154,-0.138461538461538,-0.123076923076923,-0.107692307692308,
-0.0923076923076923,-0.0769230769230769,-0.0615384615384615,-0.0461538461538462,
-0.0307692307692308,-0.0153846153846154,0.),(-1.,1.),.UNSPECIFIED.)
GEOMETRIC_REPRESENTATION_ITEM()
RATIONAL_B_SPLINE_SURFACE(((1.,1.),(1.,1.),(1.,1.),(1.,1.),(1.,1.),(1.,
1.),(1.,1.),(1.,1.),(1.,1.),(1.,1.),(1.,1.),(1.,1.),(1.,1.),(1.,1.),(1.,
1.),(1.,1.),(1.,1.),(1.,1.),(1.,1.),(1.,1.),(1.,1.),(1.,1.),(1.,1.),(1.,
1.),(1.,1.),(1.,1.),(1.,1.),(1.,1.),(1.,1.),(1.,1.),(1.,1.),(1.,1.),(1.,
1.),(1.,1.),(1.,1.),(1.,1.),(1.,1.),(1.,1.),(1.,1.),(1.,1.),(1.,1.),(1.,
1.),(1.,1.),(1.,1.),(1.,1.),(1.,1.),(1.,1.),(1.,1.),(1.,1.),(1.,1.),(1.,
1.),(1.,1.),(1.,1.),(1.,1.),(1.,1.),(1.,1.),(1.,1.),(1.,1.),(1.,1.),(1.,
1.),(1.,1.),(1.,1.),(1.,1.),(1.,1.),(1.,1.),(1.,1.),(1.,1.),(1.,1.),(1.,
1.),(1.,1.)))
REPRESENTATION_ITEM('')
SURFACE()
);
#73=(
BOUNDED_SURFACE()
B_SPLINE_SURFACE(5,1,((#44830,#44831),(#44832,#44833),(#44834,#44835),(#44836,
#44837),(#44838,#44839),(#44840,#44841),(#44842,#44843),(#44844,#44845),
(#44846,#44847),(#44848,#44849),(#44850,#44851),(#44852,#44853),(#44854,
#44855),(#44856,#44857),(#44858,#44859),(#44860,#44861),(#44862,#44863),
(#44864,#44865),(#44866,#44867),(#44868,#44869),(#44870,#44871),(#44872,
#44873),(#44874,#44875),(#44876,#44877),(#44878,#44879),(#44880,#44881),
(#44882,#44883),(#44884,#44885),(#44886,#44887),(#44888,#44889),(#44890,
#44891),(#44892,#44893),(#44894,#44895),(#44896,#44897),(#44898,#44899),
(#44900,#44901),(#44902,#44903),(#44904,#44905),(#44906,#44907),(#44908,
#44909),(#44910,#44911),(#44912,#44913),(#44914,#44915),(#44916,#44917),
(#44918,#44919),(#44920,#44921),(#44922,#44923),(#44924,#44925),(#44926,
#44927),(#44928,#44929),(#44930,#44931),(#44932,#44933),(#44934,#44935),
(#44936,#44937),(#44938,#44939),(#44940,#44941),(#44942,#44943),(#44944,
#44945),(#44946,#44947),(#44948,#44949),(#44950,#44951),(#44952,#44953),
(#44954,#44955),(#44956,#44957),(#44958,#44959),(#44960,#44961),(#44962,
#44963),(#44964,#44965),(#44966,#44967),(#44968,#44969)),.UNSPECIFIED.,
 .F.,.F.,.F.)
B_SPLINE_SURFACE_WITH_KNOTS((6,1,1,1,1,1,1,1,1,1,1,1,1,1,1,1,1,1,1,1,1,
1,1,1,1,1,1,1,1,1,1,1,1,1,1,1,1,1,1,1,1,1,1,1,1,1,1,1,1,1,1,1,1,1,1,1,1,
1,1,1,1,1,1,1,1,6),(2,2),(-1.,-0.984615384615383,-0.969230769230768,-0.953846153846152,
-0.938461538461537,-0.923076923076922,-0.907692307692306,-0.892307692307691,
-0.876923076923076,-0.86153846153846,-0.846153846153845,-0.83076923076923,
-0.815384615384614,-0.799999999999999,-0.784615384615384,-0.769230769230768,
-0.753846153846153,-0.738461538461538,-0.723076923076922,-0.707692307692307,
-0.692307692307692,-0.676923076923076,-0.661538461538461,-0.646153846153846,
-0.63076923076923,-0.615384615384615,-0.6,-0.584615384615384,-0.569230769230769,
-0.553846153846154,-0.538461538461538,-0.523076923076923,-0.507692307692308,
-0.492307692307692,-0.476923076923077,-0.461538461538462,-0.446153846153846,
-0.430769230769231,-0.415384615384615,-0.4,-0.384615384615385,-0.369230769230769,
-0.353846153846154,-0.338461538461538,-0.323076923076923,-0.307692307692308,
-0.292307692307692,-0.276923076923077,-0.261538461538462,-0.246153846153846,
-0.230769230769231,-0.215384615384615,-0.2,-0.184615384615385,-0.169230769230769,
-0.153846153846154,-0.138461538461538,-0.123076923076923,-0.107692307692308,
-0.0923076923076923,-0.0769230769230769,-0.0615384615384615,-0.0461538461538462,
-0.0307692307692308,-0.0153846153846154,0.),(-1.,1.),.UNSPECIFIED.)
GEOMETRIC_REPRESENTATION_ITEM()
RATIONAL_B_SPLINE_SURFACE(((1.,1.),(1.,1.),(1.,1.),(1.,1.),(1.,1.),(1.,
1.),(1.,1.),(1.,1.),(1.,1.),(1.,1.),(1.,1.),(1.,1.),(1.,1.),(1.,1.),(1.,
1.),(1.,1.),(1.,1.),(1.,1.),(1.,1.),(1.,1.),(1.,1.),(1.,1.),(1.,1.),(1.,
1.),(1.,1.),(1.,1.),(1.,1.),(1.,1.),(1.,1.),(1.,1.),(1.,1.),(1.,1.),(1.,
1.),(1.,1.),(1.,1.),(1.,1.),(1.,1.),(1.,1.),(1.,1.),(1.,1.),(1.,1.),(1.,
1.),(1.,1.),(1.,1.),(1.,1.),(1.,1.),(1.,1.),(1.,1.),(1.,1.),(1.,1.),(1.,
1.),(1.,1.),(1.,1.),(1.,1.),(1.,1.),(1.,1.),(1.,1.),(1.,1.),(1.,1.),(1.,
1.),(1.,1.),(1.,1.),(1.,1.),(1.,1.),(1.,1.),(1.,1.),(1.,1.),(1.,1.),(1.,
1.),(1.,1.)))
REPRESENTATION_ITEM('')
SURFACE()
);
#74=(
BOUNDED_SURFACE()
B_SPLINE_SURFACE(5,1,((#45042,#45043),(#45044,#45045),(#45046,#45047),(#45048,
#45049),(#45050,#45051),(#45052,#45053),(#45054,#45055),(#45056,#45057),
(#45058,#45059),(#45060,#45061),(#45062,#45063),(#45064,#45065),(#45066,
#45067),(#45068,#45069),(#45070,#45071),(#45072,#45073),(#45074,#45075),
(#45076,#45077),(#45078,#45079),(#45080,#45081),(#45082,#45083),(#45084,
#45085),(#45086,#45087),(#45088,#45089),(#45090,#45091),(#45092,#45093),
(#45094,#45095),(#45096,#45097),(#45098,#45099),(#45100,#45101),(#45102,
#45103),(#45104,#45105),(#45106,#45107),(#45108,#45109),(#45110,#45111),
(#45112,#45113),(#45114,#45115),(#45116,#45117),(#45118,#45119),(#45120,
#45121),(#45122,#45123),(#45124,#45125),(#45126,#45127),(#45128,#45129),
(#45130,#45131),(#45132,#45133),(#45134,#45135),(#45136,#45137),(#45138,
#45139),(#45140,#45141),(#45142,#45143),(#45144,#45145),(#45146,#45147),
(#45148,#45149),(#45150,#45151),(#45152,#45153),(#45154,#45155),(#45156,
#45157),(#45158,#45159),(#45160,#45161),(#45162,#45163),(#45164,#45165),
(#45166,#45167),(#45168,#45169),(#45170,#45171),(#45172,#45173),(#45174,
#45175),(#45176,#45177),(#45178,#45179),(#45180,#45181)),.UNSPECIFIED.,
 .F.,.F.,.F.)
B_SPLINE_SURFACE_WITH_KNOTS((6,1,1,1,1,1,1,1,1,1,1,1,1,1,1,1,1,1,1,1,1,
1,1,1,1,1,1,1,1,1,1,1,1,1,1,1,1,1,1,1,1,1,1,1,1,1,1,1,1,1,1,1,1,1,1,1,1,
1,1,1,1,1,1,1,1,6),(2,2),(-1.,-0.984615384615383,-0.969230769230768,-0.953846153846152,
-0.938461538461537,-0.923076923076922,-0.907692307692306,-0.892307692307691,
-0.876923076923076,-0.86153846153846,-0.846153846153845,-0.83076923076923,
-0.815384615384614,-0.799999999999999,-0.784615384615384,-0.769230769230768,
-0.753846153846153,-0.738461538461538,-0.723076923076922,-0.707692307692307,
-0.692307692307692,-0.676923076923076,-0.661538461538461,-0.646153846153846,
-0.63076923076923,-0.615384615384615,-0.6,-0.584615384615384,-0.569230769230769,
-0.553846153846154,-0.538461538461538,-0.523076923076923,-0.507692307692308,
-0.492307692307692,-0.476923076923077,-0.461538461538462,-0.446153846153846,
-0.430769230769231,-0.415384615384615,-0.4,-0.384615384615385,-0.369230769230769,
-0.353846153846154,-0.338461538461538,-0.323076923076923,-0.307692307692308,
-0.292307692307692,-0.276923076923077,-0.261538461538462,-0.246153846153846,
-0.230769230769231,-0.215384615384615,-0.2,-0.184615384615385,-0.169230769230769,
-0.153846153846154,-0.138461538461538,-0.123076923076923,-0.107692307692308,
-0.0923076923076923,-0.0769230769230769,-0.0615384615384615,-0.0461538461538462,
-0.0307692307692308,-0.0153846153846154,0.),(-1.,1.),.UNSPECIFIED.)
GEOMETRIC_REPRESENTATION_ITEM()
RATIONAL_B_SPLINE_SURFACE(((1.,1.),(1.,1.),(1.,1.),(1.,1.),(1.,1.),(1.,
1.),(1.,1.),(1.,1.),(1.,1.),(1.,1.),(1.,1.),(1.,1.),(1.,1.),(1.,1.),(1.,
1.),(1.,1.),(1.,1.),(1.,1.),(1.,1.),(1.,1.),(1.,1.),(1.,1.),(1.,1.),(1.,
1.),(1.,1.),(1.,1.),(1.,1.),(1.,1.),(1.,1.),(1.,1.),(1.,1.),(1.,1.),(1.,
1.),(1.,1.),(1.,1.),(1.,1.),(1.,1.),(1.,1.),(1.,1.),(1.,1.),(1.,1.),(1.,
1.),(1.,1.),(1.,1.),(1.,1.),(1.,1.),(1.,1.),(1.,1.),(1.,1.),(1.,1.),(1.,
1.),(1.,1.),(1.,1.),(1.,1.),(1.,1.),(1.,1.),(1.,1.),(1.,1.),(1.,1.),(1.,
1.),(1.,1.),(1.,1.),(1.,1.),(1.,1.),(1.,1.),(1.,1.),(1.,1.),(1.,1.),(1.,
1.),(1.,1.)))
REPRESENTATION_ITEM('')
SURFACE()
);
#75=(
BOUNDED_SURFACE()
B_SPLINE_SURFACE(5,1,((#45272,#45273),(#45274,#45275),(#45276,#45277),(#45278,
#45279),(#45280,#45281),(#45282,#45283),(#45284,#45285),(#45286,#45287),
(#45288,#45289),(#45290,#45291),(#45292,#45293),(#45294,#45295),(#45296,
#45297),(#45298,#45299),(#45300,#45301),(#45302,#45303),(#45304,#45305),
(#45306,#45307),(#45308,#45309),(#45310,#45311),(#45312,#45313),(#45314,
#45315),(#45316,#45317),(#45318,#45319),(#45320,#45321),(#45322,#45323),
(#45324,#45325),(#45326,#45327),(#45328,#45329),(#45330,#45331),(#45332,
#45333),(#45334,#45335),(#45336,#45337),(#45338,#45339),(#45340,#45341),
(#45342,#45343),(#45344,#45345),(#45346,#45347),(#45348,#45349),(#45350,
#45351),(#45352,#45353),(#45354,#45355),(#45356,#45357),(#45358,#45359),
(#45360,#45361),(#45362,#45363),(#45364,#45365),(#45366,#45367),(#45368,
#45369),(#45370,#45371),(#45372,#45373),(#45374,#45375),(#45376,#45377),
(#45378,#45379),(#45380,#45381),(#45382,#45383),(#45384,#45385),(#45386,
#45387),(#45388,#45389),(#45390,#45391),(#45392,#45393),(#45394,#45395),
(#45396,#45397),(#45398,#45399),(#45400,#45401),(#45402,#45403),(#45404,
#45405),(#45406,#45407),(#45408,#45409),(#45410,#45411)),.UNSPECIFIED.,
 .F.,.F.,.F.)
B_SPLINE_SURFACE_WITH_KNOTS((6,1,1,1,1,1,1,1,1,1,1,1,1,1,1,1,1,1,1,1,1,
1,1,1,1,1,1,1,1,1,1,1,1,1,1,1,1,1,1,1,1,1,1,1,1,1,1,1,1,1,1,1,1,1,1,1,1,
1,1,1,1,1,1,1,1,6),(2,2),(-1.,-0.984615384615383,-0.969230769230768,-0.953846153846152,
-0.938461538461537,-0.923076923076922,-0.907692307692306,-0.892307692307691,
-0.876923076923076,-0.86153846153846,-0.846153846153845,-0.83076923076923,
-0.815384615384614,-0.799999999999999,-0.784615384615384,-0.769230769230768,
-0.753846153846153,-0.738461538461538,-0.723076923076922,-0.707692307692307,
-0.692307692307692,-0.676923076923076,-0.661538461538461,-0.646153846153846,
-0.63076923076923,-0.615384615384615,-0.6,-0.584615384615384,-0.569230769230769,
-0.553846153846154,-0.538461538461538,-0.523076923076923,-0.507692307692308,
-0.492307692307692,-0.476923076923077,-0.461538461538462,-0.446153846153846,
-0.430769230769231,-0.415384615384615,-0.4,-0.384615384615385,-0.369230769230769,
-0.353846153846154,-0.338461538461538,-0.323076923076923,-0.307692307692308,
-0.292307692307692,-0.276923076923077,-0.261538461538462,-0.246153846153846,
-0.230769230769231,-0.215384615384615,-0.2,-0.184615384615385,-0.169230769230769,
-0.153846153846154,-0.138461538461538,-0.123076923076923,-0.107692307692308,
-0.0923076923076923,-0.0769230769230769,-0.0615384615384615,-0.0461538461538462,
-0.0307692307692308,-0.0153846153846154,0.),(-1.,1.),.UNSPECIFIED.)
GEOMETRIC_REPRESENTATION_ITEM()
RATIONAL_B_SPLINE_SURFACE(((1.,1.),(1.,1.),(1.,1.),(1.,1.),(1.,1.),(1.,
1.),(1.,1.),(1.,1.),(1.,1.),(1.,1.),(1.,1.),(1.,1.),(1.,1.),(1.,1.),(1.,
1.),(1.,1.),(1.,1.),(1.,1.),(1.,1.),(1.,1.),(1.,1.),(1.,1.),(1.,1.),(1.,
1.),(1.,1.),(1.,1.),(1.,1.),(1.,1.),(1.,1.),(1.,1.),(1.,1.),(1.,1.),(1.,
1.),(1.,1.),(1.,1.),(1.,1.),(1.,1.),(1.,1.),(1.,1.),(1.,1.),(1.,1.),(1.,
1.),(1.,1.),(1.,1.),(1.,1.),(1.,1.),(1.,1.),(1.,1.),(1.,1.),(1.,1.),(1.,
1.),(1.,1.),(1.,1.),(1.,1.),(1.,1.),(1.,1.),(1.,1.),(1.,1.),(1.,1.),(1.,
1.),(1.,1.),(1.,1.),(1.,1.),(1.,1.),(1.,1.),(1.,1.),(1.,1.),(1.,1.),(1.,
1.),(1.,1.)))
REPRESENTATION_ITEM('')
SURFACE()
);
#76=(
BOUNDED_SURFACE()
B_SPLINE_SURFACE(5,1,((#45484,#45485),(#45486,#45487),(#45488,#45489),(#45490,
#45491),(#45492,#45493),(#45494,#45495),(#45496,#45497),(#45498,#45499),
(#45500,#45501),(#45502,#45503),(#45504,#45505),(#45506,#45507),(#45508,
#45509),(#45510,#45511),(#45512,#45513),(#45514,#45515),(#45516,#45517),
(#45518,#45519),(#45520,#45521),(#45522,#45523),(#45524,#45525),(#45526,
#45527),(#45528,#45529),(#45530,#45531),(#45532,#45533),(#45534,#45535),
(#45536,#45537),(#45538,#45539),(#45540,#45541),(#45542,#45543),(#45544,
#45545),(#45546,#45547),(#45548,#45549),(#45550,#45551),(#45552,#45553),
(#45554,#45555),(#45556,#45557),(#45558,#45559),(#45560,#45561),(#45562,
#45563),(#45564,#45565),(#45566,#45567),(#45568,#45569),(#45570,#45571),
(#45572,#45573),(#45574,#45575),(#45576,#45577),(#45578,#45579),(#45580,
#45581),(#45582,#45583),(#45584,#45585),(#45586,#45587),(#45588,#45589),
(#45590,#45591),(#45592,#45593),(#45594,#45595),(#45596,#45597),(#45598,
#45599),(#45600,#45601),(#45602,#45603),(#45604,#45605),(#45606,#45607),
(#45608,#45609),(#45610,#45611),(#45612,#45613),(#45614,#45615),(#45616,
#45617),(#45618,#45619),(#45620,#45621),(#45622,#45623)),.UNSPECIFIED.,
 .F.,.F.,.F.)
B_SPLINE_SURFACE_WITH_KNOTS((6,1,1,1,1,1,1,1,1,1,1,1,1,1,1,1,1,1,1,1,1,
1,1,1,1,1,1,1,1,1,1,1,1,1,1,1,1,1,1,1,1,1,1,1,1,1,1,1,1,1,1,1,1,1,1,1,1,
1,1,1,1,1,1,1,1,6),(2,2),(-1.,-0.984615384615383,-0.969230769230768,-0.953846153846152,
-0.938461538461537,-0.923076923076922,-0.907692307692306,-0.892307692307691,
-0.876923076923076,-0.86153846153846,-0.846153846153845,-0.83076923076923,
-0.815384615384614,-0.799999999999999,-0.784615384615384,-0.769230769230768,
-0.753846153846153,-0.738461538461538,-0.723076923076922,-0.707692307692307,
-0.692307692307692,-0.676923076923076,-0.661538461538461,-0.646153846153846,
-0.63076923076923,-0.615384615384615,-0.6,-0.584615384615384,-0.569230769230769,
-0.553846153846154,-0.538461538461538,-0.523076923076923,-0.507692307692308,
-0.492307692307692,-0.476923076923077,-0.461538461538462,-0.446153846153846,
-0.430769230769231,-0.415384615384615,-0.4,-0.384615384615385,-0.369230769230769,
-0.353846153846154,-0.338461538461538,-0.323076923076923,-0.307692307692308,
-0.292307692307692,-0.276923076923077,-0.261538461538462,-0.246153846153846,
-0.230769230769231,-0.215384615384615,-0.2,-0.184615384615385,-0.169230769230769,
-0.153846153846154,-0.138461538461538,-0.123076923076923,-0.107692307692308,
-0.0923076923076923,-0.0769230769230769,-0.0615384615384615,-0.0461538461538462,
-0.0307692307692308,-0.0153846153846154,0.),(-1.,1.),.UNSPECIFIED.)
GEOMETRIC_REPRESENTATION_ITEM()
RATIONAL_B_SPLINE_SURFACE(((1.,1.),(1.,1.),(1.,1.),(1.,1.),(1.,1.),(1.,
1.),(1.,1.),(1.,1.),(1.,1.),(1.,1.),(1.,1.),(1.,1.),(1.,1.),(1.,1.),(1.,
1.),(1.,1.),(1.,1.),(1.,1.),(1.,1.),(1.,1.),(1.,1.),(1.,1.),(1.,1.),(1.,
1.),(1.,1.),(1.,1.),(1.,1.),(1.,1.),(1.,1.),(1.,1.),(1.,1.),(1.,1.),(1.,
1.),(1.,1.),(1.,1.),(1.,1.),(1.,1.),(1.,1.),(1.,1.),(1.,1.),(1.,1.),(1.,
1.),(1.,1.),(1.,1.),(1.,1.),(1.,1.),(1.,1.),(1.,1.),(1.,1.),(1.,1.),(1.,
1.),(1.,1.),(1.,1.),(1.,1.),(1.,1.),(1.,1.),(1.,1.),(1.,1.),(1.,1.),(1.,
1.),(1.,1.),(1.,1.),(1.,1.),(1.,1.),(1.,1.),(1.,1.),(1.,1.),(1.,1.),(1.,
1.),(1.,1.)))
REPRESENTATION_ITEM('')
SURFACE()
);
#77=(
BOUNDED_SURFACE()
B_SPLINE_SURFACE(5,1,((#45714,#45715),(#45716,#45717),(#45718,#45719),(#45720,
#45721),(#45722,#45723),(#45724,#45725),(#45726,#45727),(#45728,#45729),
(#45730,#45731),(#45732,#45733),(#45734,#45735),(#45736,#45737),(#45738,
#45739),(#45740,#45741),(#45742,#45743),(#45744,#45745),(#45746,#45747),
(#45748,#45749),(#45750,#45751),(#45752,#45753),(#45754,#45755),(#45756,
#45757),(#45758,#45759),(#45760,#45761),(#45762,#45763),(#45764,#45765),
(#45766,#45767),(#45768,#45769),(#45770,#45771),(#45772,#45773),(#45774,
#45775),(#45776,#45777),(#45778,#45779),(#45780,#45781),(#45782,#45783),
(#45784,#45785),(#45786,#45787),(#45788,#45789),(#45790,#45791),(#45792,
#45793),(#45794,#45795),(#45796,#45797),(#45798,#45799),(#45800,#45801),
(#45802,#45803),(#45804,#45805),(#45806,#45807),(#45808,#45809),(#45810,
#45811),(#45812,#45813),(#45814,#45815),(#45816,#45817),(#45818,#45819),
(#45820,#45821),(#45822,#45823),(#45824,#45825),(#45826,#45827),(#45828,
#45829),(#45830,#45831),(#45832,#45833),(#45834,#45835),(#45836,#45837),
(#45838,#45839),(#45840,#45841),(#45842,#45843),(#45844,#45845),(#45846,
#45847),(#45848,#45849),(#45850,#45851),(#45852,#45853)),.UNSPECIFIED.,
 .F.,.F.,.F.)
B_SPLINE_SURFACE_WITH_KNOTS((6,1,1,1,1,1,1,1,1,1,1,1,1,1,1,1,1,1,1,1,1,
1,1,1,1,1,1,1,1,1,1,1,1,1,1,1,1,1,1,1,1,1,1,1,1,1,1,1,1,1,1,1,1,1,1,1,1,
1,1,1,1,1,1,1,1,6),(2,2),(-1.,-0.984615384615383,-0.969230769230768,-0.953846153846152,
-0.938461538461537,-0.923076923076922,-0.907692307692306,-0.892307692307691,
-0.876923076923076,-0.86153846153846,-0.846153846153845,-0.83076923076923,
-0.815384615384614,-0.799999999999999,-0.784615384615384,-0.769230769230768,
-0.753846153846153,-0.738461538461538,-0.723076923076922,-0.707692307692307,
-0.692307692307692,-0.676923076923076,-0.661538461538461,-0.646153846153846,
-0.63076923076923,-0.615384615384615,-0.6,-0.584615384615384,-0.569230769230769,
-0.553846153846154,-0.538461538461538,-0.523076923076923,-0.507692307692308,
-0.492307692307692,-0.476923076923077,-0.461538461538462,-0.446153846153846,
-0.430769230769231,-0.415384615384615,-0.4,-0.384615384615385,-0.369230769230769,
-0.353846153846154,-0.338461538461538,-0.323076923076923,-0.307692307692308,
-0.292307692307692,-0.276923076923077,-0.261538461538462,-0.246153846153846,
-0.230769230769231,-0.215384615384615,-0.2,-0.184615384615385,-0.169230769230769,
-0.153846153846154,-0.138461538461538,-0.123076923076923,-0.107692307692308,
-0.0923076923076923,-0.0769230769230769,-0.0615384615384615,-0.0461538461538462,
-0.0307692307692308,-0.0153846153846154,0.),(-1.,1.),.UNSPECIFIED.)
GEOMETRIC_REPRESENTATION_ITEM()
RATIONAL_B_SPLINE_SURFACE(((1.,1.),(1.,1.),(1.,1.),(1.,1.),(1.,1.),(1.,
1.),(1.,1.),(1.,1.),(1.,1.),(1.,1.),(1.,1.),(1.,1.),(1.,1.),(1.,1.),(1.,
1.),(1.,1.),(1.,1.),(1.,1.),(1.,1.),(1.,1.),(1.,1.),(1.,1.),(1.,1.),(1.,
1.),(1.,1.),(1.,1.),(1.,1.),(1.,1.),(1.,1.),(1.,1.),(1.,1.),(1.,1.),(1.,
1.),(1.,1.),(1.,1.),(1.,1.),(1.,1.),(1.,1.),(1.,1.),(1.,1.),(1.,1.),(1.,
1.),(1.,1.),(1.,1.),(1.,1.),(1.,1.),(1.,1.),(1.,1.),(1.,1.),(1.,1.),(1.,
1.),(1.,1.),(1.,1.),(1.,1.),(1.,1.),(1.,1.),(1.,1.),(1.,1.),(1.,1.),(1.,
1.),(1.,1.),(1.,1.),(1.,1.),(1.,1.),(1.,1.),(1.,1.),(1.,1.),(1.,1.),(1.,
1.),(1.,1.)))
REPRESENTATION_ITEM('')
SURFACE()
);
#78=(
BOUNDED_SURFACE()
B_SPLINE_SURFACE(5,1,((#45926,#45927),(#45928,#45929),(#45930,#45931),(#45932,
#45933),(#45934,#45935),(#45936,#45937),(#45938,#45939),(#45940,#45941),
(#45942,#45943),(#45944,#45945),(#45946,#45947),(#45948,#45949),(#45950,
#45951),(#45952,#45953),(#45954,#45955),(#45956,#45957),(#45958,#45959),
(#45960,#45961),(#45962,#45963),(#45964,#45965),(#45966,#45967),(#45968,
#45969),(#45970,#45971),(#45972,#45973),(#45974,#45975),(#45976,#45977),
(#45978,#45979),(#45980,#45981),(#45982,#45983),(#45984,#45985),(#45986,
#45987),(#45988,#45989),(#45990,#45991),(#45992,#45993),(#45994,#45995),
(#45996,#45997),(#45998,#45999),(#46000,#46001),(#46002,#46003),(#46004,
#46005),(#46006,#46007),(#46008,#46009),(#46010,#46011),(#46012,#46013),
(#46014,#46015),(#46016,#46017),(#46018,#46019),(#46020,#46021),(#46022,
#46023),(#46024,#46025),(#46026,#46027),(#46028,#46029),(#46030,#46031),
(#46032,#46033),(#46034,#46035),(#46036,#46037),(#46038,#46039),(#46040,
#46041),(#46042,#46043),(#46044,#46045),(#46046,#46047),(#46048,#46049),
(#46050,#46051),(#46052,#46053),(#46054,#46055),(#46056,#46057),(#46058,
#46059),(#46060,#46061),(#46062,#46063),(#46064,#46065)),.UNSPECIFIED.,
 .F.,.F.,.F.)
B_SPLINE_SURFACE_WITH_KNOTS((6,1,1,1,1,1,1,1,1,1,1,1,1,1,1,1,1,1,1,1,1,
1,1,1,1,1,1,1,1,1,1,1,1,1,1,1,1,1,1,1,1,1,1,1,1,1,1,1,1,1,1,1,1,1,1,1,1,
1,1,1,1,1,1,1,1,6),(2,2),(-1.,-0.984615384615383,-0.969230769230768,-0.953846153846152,
-0.938461538461537,-0.923076923076922,-0.907692307692306,-0.892307692307691,
-0.876923076923076,-0.86153846153846,-0.846153846153845,-0.83076923076923,
-0.815384615384614,-0.799999999999999,-0.784615384615384,-0.769230769230768,
-0.753846153846153,-0.738461538461538,-0.723076923076922,-0.707692307692307,
-0.692307692307692,-0.676923076923076,-0.661538461538461,-0.646153846153846,
-0.63076923076923,-0.615384615384615,-0.6,-0.584615384615384,-0.569230769230769,
-0.553846153846154,-0.538461538461538,-0.523076923076923,-0.507692307692308,
-0.492307692307692,-0.476923076923077,-0.461538461538462,-0.446153846153846,
-0.430769230769231,-0.415384615384615,-0.4,-0.384615384615385,-0.369230769230769,
-0.353846153846154,-0.338461538461538,-0.323076923076923,-0.307692307692308,
-0.292307692307692,-0.276923076923077,-0.261538461538462,-0.246153846153846,
-0.230769230769231,-0.215384615384615,-0.2,-0.184615384615385,-0.169230769230769,
-0.153846153846154,-0.138461538461538,-0.123076923076923,-0.107692307692308,
-0.0923076923076923,-0.0769230769230769,-0.0615384615384615,-0.0461538461538462,
-0.0307692307692308,-0.0153846153846154,0.),(-1.,1.),.UNSPECIFIED.)
GEOMETRIC_REPRESENTATION_ITEM()
RATIONAL_B_SPLINE_SURFACE(((1.,1.),(1.,1.),(1.,1.),(1.,1.),(1.,1.),(1.,
1.),(1.,1.),(1.,1.),(1.,1.),(1.,1.),(1.,1.),(1.,1.),(1.,1.),(1.,1.),(1.,
1.),(1.,1.),(1.,1.),(1.,1.),(1.,1.),(1.,1.),(1.,1.),(1.,1.),(1.,1.),(1.,
1.),(1.,1.),(1.,1.),(1.,1.),(1.,1.),(1.,1.),(1.,1.),(1.,1.),(1.,1.),(1.,
1.),(1.,1.),(1.,1.),(1.,1.),(1.,1.),(1.,1.),(1.,1.),(1.,1.),(1.,1.),(1.,
1.),(1.,1.),(1.,1.),(1.,1.),(1.,1.),(1.,1.),(1.,1.),(1.,1.),(1.,1.),(1.,
1.),(1.,1.),(1.,1.),(1.,1.),(1.,1.),(1.,1.),(1.,1.),(1.,1.),(1.,1.),(1.,
1.),(1.,1.),(1.,1.),(1.,1.),(1.,1.),(1.,1.),(1.,1.),(1.,1.),(1.,1.),(1.,
1.),(1.,1.)))
REPRESENTATION_ITEM('')
SURFACE()
);
#79=(
BOUNDED_SURFACE()
B_SPLINE_SURFACE(5,1,((#46156,#46157),(#46158,#46159),(#46160,#46161),(#46162,
#46163),(#46164,#46165),(#46166,#46167),(#46168,#46169),(#46170,#46171),
(#46172,#46173),(#46174,#46175),(#46176,#46177),(#46178,#46179),(#46180,
#46181),(#46182,#46183),(#46184,#46185),(#46186,#46187),(#46188,#46189),
(#46190,#46191),(#46192,#46193),(#46194,#46195),(#46196,#46197),(#46198,
#46199),(#46200,#46201),(#46202,#46203),(#46204,#46205),(#46206,#46207),
(#46208,#46209),(#46210,#46211),(#46212,#46213),(#46214,#46215),(#46216,
#46217),(#46218,#46219),(#46220,#46221),(#46222,#46223),(#46224,#46225),
(#46226,#46227),(#46228,#46229),(#46230,#46231),(#46232,#46233),(#46234,
#46235),(#46236,#46237),(#46238,#46239),(#46240,#46241),(#46242,#46243),
(#46244,#46245),(#46246,#46247),(#46248,#46249),(#46250,#46251),(#46252,
#46253),(#46254,#46255),(#46256,#46257),(#46258,#46259),(#46260,#46261),
(#46262,#46263),(#46264,#46265),(#46266,#46267),(#46268,#46269),(#46270,
#46271),(#46272,#46273),(#46274,#46275),(#46276,#46277),(#46278,#46279),
(#46280,#46281),(#46282,#46283),(#46284,#46285),(#46286,#46287),(#46288,
#46289),(#46290,#46291),(#46292,#46293),(#46294,#46295)),.UNSPECIFIED.,
 .F.,.F.,.F.)
B_SPLINE_SURFACE_WITH_KNOTS((6,1,1,1,1,1,1,1,1,1,1,1,1,1,1,1,1,1,1,1,1,
1,1,1,1,1,1,1,1,1,1,1,1,1,1,1,1,1,1,1,1,1,1,1,1,1,1,1,1,1,1,1,1,1,1,1,1,
1,1,1,1,1,1,1,1,6),(2,2),(-1.,-0.984615384615383,-0.969230769230768,-0.953846153846152,
-0.938461538461537,-0.923076923076922,-0.907692307692306,-0.892307692307691,
-0.876923076923076,-0.86153846153846,-0.846153846153845,-0.83076923076923,
-0.815384615384614,-0.799999999999999,-0.784615384615384,-0.769230769230768,
-0.753846153846153,-0.738461538461538,-0.723076923076922,-0.707692307692307,
-0.692307692307692,-0.676923076923076,-0.661538461538461,-0.646153846153846,
-0.63076923076923,-0.615384615384615,-0.6,-0.584615384615384,-0.569230769230769,
-0.553846153846154,-0.538461538461538,-0.523076923076923,-0.507692307692308,
-0.492307692307692,-0.476923076923077,-0.461538461538462,-0.446153846153846,
-0.430769230769231,-0.415384615384615,-0.4,-0.384615384615385,-0.369230769230769,
-0.353846153846154,-0.338461538461538,-0.323076923076923,-0.307692307692308,
-0.292307692307692,-0.276923076923077,-0.261538461538462,-0.246153846153846,
-0.230769230769231,-0.215384615384615,-0.2,-0.184615384615385,-0.169230769230769,
-0.153846153846154,-0.138461538461538,-0.123076923076923,-0.107692307692308,
-0.0923076923076923,-0.0769230769230769,-0.0615384615384615,-0.0461538461538462,
-0.0307692307692308,-0.0153846153846154,0.),(-1.,1.),.UNSPECIFIED.)
GEOMETRIC_REPRESENTATION_ITEM()
RATIONAL_B_SPLINE_SURFACE(((1.,1.),(1.,1.),(1.,1.),(1.,1.),(1.,1.),(1.,
1.),(1.,1.),(1.,1.),(1.,1.),(1.,1.),(1.,1.),(1.,1.),(1.,1.),(1.,1.),(1.,
1.),(1.,1.),(1.,1.),(1.,1.),(1.,1.),(1.,1.),(1.,1.),(1.,1.),(1.,1.),(1.,
1.),(1.,1.),(1.,1.),(1.,1.),(1.,1.),(1.,1.),(1.,1.),(1.,1.),(1.,1.),(1.,
1.),(1.,1.),(1.,1.),(1.,1.),(1.,1.),(1.,1.),(1.,1.),(1.,1.),(1.,1.),(1.,
1.),(1.,1.),(1.,1.),(1.,1.),(1.,1.),(1.,1.),(1.,1.),(1.,1.),(1.,1.),(1.,
1.),(1.,1.),(1.,1.),(1.,1.),(1.,1.),(1.,1.),(1.,1.),(1.,1.),(1.,1.),(1.,
1.),(1.,1.),(1.,1.),(1.,1.),(1.,1.),(1.,1.),(1.,1.),(1.,1.),(1.,1.),(1.,
1.),(1.,1.)))
REPRESENTATION_ITEM('')
SURFACE()
);
#80=(
BOUNDED_SURFACE()
B_SPLINE_SURFACE(5,1,((#46368,#46369),(#46370,#46371),(#46372,#46373),(#46374,
#46375),(#46376,#46377),(#46378,#46379),(#46380,#46381),(#46382,#46383),
(#46384,#46385),(#46386,#46387),(#46388,#46389),(#46390,#46391),(#46392,
#46393),(#46394,#46395),(#46396,#46397),(#46398,#46399),(#46400,#46401),
(#46402,#46403),(#46404,#46405),(#46406,#46407),(#46408,#46409),(#46410,
#46411),(#46412,#46413),(#46414,#46415),(#46416,#46417),(#46418,#46419),
(#46420,#46421),(#46422,#46423),(#46424,#46425),(#46426,#46427),(#46428,
#46429),(#46430,#46431),(#46432,#46433),(#46434,#46435),(#46436,#46437),
(#46438,#46439),(#46440,#46441),(#46442,#46443),(#46444,#46445),(#46446,
#46447),(#46448,#46449),(#46450,#46451),(#46452,#46453),(#46454,#46455),
(#46456,#46457),(#46458,#46459),(#46460,#46461),(#46462,#46463),(#46464,
#46465),(#46466,#46467),(#46468,#46469),(#46470,#46471),(#46472,#46473),
(#46474,#46475),(#46476,#46477),(#46478,#46479),(#46480,#46481),(#46482,
#46483),(#46484,#46485),(#46486,#46487),(#46488,#46489),(#46490,#46491),
(#46492,#46493),(#46494,#46495),(#46496,#46497),(#46498,#46499),(#46500,
#46501),(#46502,#46503),(#46504,#46505),(#46506,#46507)),.UNSPECIFIED.,
 .F.,.F.,.F.)
B_SPLINE_SURFACE_WITH_KNOTS((6,1,1,1,1,1,1,1,1,1,1,1,1,1,1,1,1,1,1,1,1,
1,1,1,1,1,1,1,1,1,1,1,1,1,1,1,1,1,1,1,1,1,1,1,1,1,1,1,1,1,1,1,1,1,1,1,1,
1,1,1,1,1,1,1,1,6),(2,2),(-1.,-0.984615384615383,-0.969230769230768,-0.953846153846152,
-0.938461538461537,-0.923076923076922,-0.907692307692306,-0.892307692307691,
-0.876923076923076,-0.86153846153846,-0.846153846153845,-0.83076923076923,
-0.815384615384614,-0.799999999999999,-0.784615384615384,-0.769230769230768,
-0.753846153846153,-0.738461538461538,-0.723076923076922,-0.707692307692307,
-0.692307692307692,-0.676923076923076,-0.661538461538461,-0.646153846153846,
-0.63076923076923,-0.615384615384615,-0.6,-0.584615384615384,-0.569230769230769,
-0.553846153846154,-0.538461538461538,-0.523076923076923,-0.507692307692308,
-0.492307692307692,-0.476923076923077,-0.461538461538462,-0.446153846153846,
-0.430769230769231,-0.415384615384615,-0.4,-0.384615384615385,-0.369230769230769,
-0.353846153846154,-0.338461538461538,-0.323076923076923,-0.307692307692308,
-0.292307692307692,-0.276923076923077,-0.261538461538462,-0.246153846153846,
-0.230769230769231,-0.215384615384615,-0.2,-0.184615384615385,-0.169230769230769,
-0.153846153846154,-0.138461538461538,-0.123076923076923,-0.107692307692308,
-0.0923076923076923,-0.0769230769230769,-0.0615384615384615,-0.0461538461538462,
-0.0307692307692308,-0.0153846153846154,0.),(-1.,1.),.UNSPECIFIED.)
GEOMETRIC_REPRESENTATION_ITEM()
RATIONAL_B_SPLINE_SURFACE(((1.,1.),(1.,1.),(1.,1.),(1.,1.),(1.,1.),(1.,
1.),(1.,1.),(1.,1.),(1.,1.),(1.,1.),(1.,1.),(1.,1.),(1.,1.),(1.,1.),(1.,
1.),(1.,1.),(1.,1.),(1.,1.),(1.,1.),(1.,1.),(1.,1.),(1.,1.),(1.,1.),(1.,
1.),(1.,1.),(1.,1.),(1.,1.),(1.,1.),(1.,1.),(1.,1.),(1.,1.),(1.,1.),(1.,
1.),(1.,1.),(1.,1.),(1.,1.),(1.,1.),(1.,1.),(1.,1.),(1.,1.),(1.,1.),(1.,
1.),(1.,1.),(1.,1.),(1.,1.),(1.,1.),(1.,1.),(1.,1.),(1.,1.),(1.,1.),(1.,
1.),(1.,1.),(1.,1.),(1.,1.),(1.,1.),(1.,1.),(1.,1.),(1.,1.),(1.,1.),(1.,
1.),(1.,1.),(1.,1.),(1.,1.),(1.,1.),(1.,1.),(1.,1.),(1.,1.),(1.,1.),(1.,
1.),(1.,1.)))
REPRESENTATION_ITEM('')
SURFACE()
);
#81=(
BOUNDED_SURFACE()
B_SPLINE_SURFACE(5,1,((#46598,#46599),(#46600,#46601),(#46602,#46603),(#46604,
#46605),(#46606,#46607),(#46608,#46609),(#46610,#46611),(#46612,#46613),
(#46614,#46615),(#46616,#46617),(#46618,#46619),(#46620,#46621),(#46622,
#46623),(#46624,#46625),(#46626,#46627),(#46628,#46629),(#46630,#46631),
(#46632,#46633),(#46634,#46635),(#46636,#46637),(#46638,#46639),(#46640,
#46641),(#46642,#46643),(#46644,#46645),(#46646,#46647),(#46648,#46649),
(#46650,#46651),(#46652,#46653),(#46654,#46655),(#46656,#46657),(#46658,
#46659),(#46660,#46661),(#46662,#46663),(#46664,#46665),(#46666,#46667),
(#46668,#46669),(#46670,#46671),(#46672,#46673),(#46674,#46675),(#46676,
#46677),(#46678,#46679),(#46680,#46681),(#46682,#46683),(#46684,#46685),
(#46686,#46687),(#46688,#46689),(#46690,#46691),(#46692,#46693),(#46694,
#46695),(#46696,#46697),(#46698,#46699),(#46700,#46701),(#46702,#46703),
(#46704,#46705),(#46706,#46707),(#46708,#46709),(#46710,#46711),(#46712,
#46713),(#46714,#46715),(#46716,#46717),(#46718,#46719),(#46720,#46721),
(#46722,#46723),(#46724,#46725),(#46726,#46727),(#46728,#46729),(#46730,
#46731),(#46732,#46733),(#46734,#46735),(#46736,#46737)),.UNSPECIFIED.,
 .F.,.F.,.F.)
B_SPLINE_SURFACE_WITH_KNOTS((6,1,1,1,1,1,1,1,1,1,1,1,1,1,1,1,1,1,1,1,1,
1,1,1,1,1,1,1,1,1,1,1,1,1,1,1,1,1,1,1,1,1,1,1,1,1,1,1,1,1,1,1,1,1,1,1,1,
1,1,1,1,1,1,1,1,6),(2,2),(-1.,-0.984615384615383,-0.969230769230768,-0.953846153846152,
-0.938461538461537,-0.923076923076922,-0.907692307692306,-0.892307692307691,
-0.876923076923076,-0.86153846153846,-0.846153846153845,-0.83076923076923,
-0.815384615384614,-0.799999999999999,-0.784615384615384,-0.769230769230768,
-0.753846153846153,-0.738461538461538,-0.723076923076922,-0.707692307692307,
-0.692307692307692,-0.676923076923076,-0.661538461538461,-0.646153846153846,
-0.63076923076923,-0.615384615384615,-0.6,-0.584615384615384,-0.569230769230769,
-0.553846153846154,-0.538461538461538,-0.523076923076923,-0.507692307692308,
-0.492307692307692,-0.476923076923077,-0.461538461538462,-0.446153846153846,
-0.430769230769231,-0.415384615384615,-0.4,-0.384615384615385,-0.369230769230769,
-0.353846153846154,-0.338461538461538,-0.323076923076923,-0.307692307692308,
-0.292307692307692,-0.276923076923077,-0.261538461538462,-0.246153846153846,
-0.230769230769231,-0.215384615384615,-0.2,-0.184615384615385,-0.169230769230769,
-0.153846153846154,-0.138461538461538,-0.123076923076923,-0.107692307692308,
-0.0923076923076923,-0.0769230769230769,-0.0615384615384615,-0.0461538461538462,
-0.0307692307692308,-0.0153846153846154,0.),(-1.,1.),.UNSPECIFIED.)
GEOMETRIC_REPRESENTATION_ITEM()
RATIONAL_B_SPLINE_SURFACE(((1.,1.),(1.,1.),(1.,1.),(1.,1.),(1.,1.),(1.,
1.),(1.,1.),(1.,1.),(1.,1.),(1.,1.),(1.,1.),(1.,1.),(1.,1.),(1.,1.),(1.,
1.),(1.,1.),(1.,1.),(1.,1.),(1.,1.),(1.,1.),(1.,1.),(1.,1.),(1.,1.),(1.,
1.),(1.,1.),(1.,1.),(1.,1.),(1.,1.),(1.,1.),(1.,1.),(1.,1.),(1.,1.),(1.,
1.),(1.,1.),(1.,1.),(1.,1.),(1.,1.),(1.,1.),(1.,1.),(1.,1.),(1.,1.),(1.,
1.),(1.,1.),(1.,1.),(1.,1.),(1.,1.),(1.,1.),(1.,1.),(1.,1.),(1.,1.),(1.,
1.),(1.,1.),(1.,1.),(1.,1.),(1.,1.),(1.,1.),(1.,1.),(1.,1.),(1.,1.),(1.,
1.),(1.,1.),(1.,1.),(1.,1.),(1.,1.),(1.,1.),(1.,1.),(1.,1.),(1.,1.),(1.,
1.),(1.,1.)))
REPRESENTATION_ITEM('')
SURFACE()
);
#82=(
BOUNDED_SURFACE()
B_SPLINE_SURFACE(5,1,((#46810,#46811),(#46812,#46813),(#46814,#46815),(#46816,
#46817),(#46818,#46819),(#46820,#46821),(#46822,#46823),(#46824,#46825),
(#46826,#46827),(#46828,#46829),(#46830,#46831),(#46832,#46833),(#46834,
#46835),(#46836,#46837),(#46838,#46839),(#46840,#46841),(#46842,#46843),
(#46844,#46845),(#46846,#46847),(#46848,#46849),(#46850,#46851),(#46852,
#46853),(#46854,#46855),(#46856,#46857),(#46858,#46859),(#46860,#46861),
(#46862,#46863),(#46864,#46865),(#46866,#46867),(#46868,#46869),(#46870,
#46871),(#46872,#46873),(#46874,#46875),(#46876,#46877),(#46878,#46879),
(#46880,#46881),(#46882,#46883),(#46884,#46885),(#46886,#46887),(#46888,
#46889),(#46890,#46891),(#46892,#46893),(#46894,#46895),(#46896,#46897),
(#46898,#46899),(#46900,#46901),(#46902,#46903),(#46904,#46905),(#46906,
#46907),(#46908,#46909),(#46910,#46911),(#46912,#46913),(#46914,#46915),
(#46916,#46917),(#46918,#46919),(#46920,#46921),(#46922,#46923),(#46924,
#46925),(#46926,#46927),(#46928,#46929),(#46930,#46931),(#46932,#46933),
(#46934,#46935),(#46936,#46937),(#46938,#46939),(#46940,#46941),(#46942,
#46943),(#46944,#46945),(#46946,#46947),(#46948,#46949)),.UNSPECIFIED.,
 .F.,.F.,.F.)
B_SPLINE_SURFACE_WITH_KNOTS((6,1,1,1,1,1,1,1,1,1,1,1,1,1,1,1,1,1,1,1,1,
1,1,1,1,1,1,1,1,1,1,1,1,1,1,1,1,1,1,1,1,1,1,1,1,1,1,1,1,1,1,1,1,1,1,1,1,
1,1,1,1,1,1,1,1,6),(2,2),(-1.,-0.984615384615383,-0.969230769230768,-0.953846153846152,
-0.938461538461537,-0.923076923076922,-0.907692307692306,-0.892307692307691,
-0.876923076923076,-0.86153846153846,-0.846153846153845,-0.83076923076923,
-0.815384615384614,-0.799999999999999,-0.784615384615384,-0.769230769230768,
-0.753846153846153,-0.738461538461538,-0.723076923076922,-0.707692307692307,
-0.692307692307692,-0.676923076923076,-0.661538461538461,-0.646153846153846,
-0.63076923076923,-0.615384615384615,-0.6,-0.584615384615384,-0.569230769230769,
-0.553846153846154,-0.538461538461538,-0.523076923076923,-0.507692307692308,
-0.492307692307692,-0.476923076923077,-0.461538461538462,-0.446153846153846,
-0.430769230769231,-0.415384615384615,-0.4,-0.384615384615385,-0.369230769230769,
-0.353846153846154,-0.338461538461538,-0.323076923076923,-0.307692307692308,
-0.292307692307692,-0.276923076923077,-0.261538461538462,-0.246153846153846,
-0.230769230769231,-0.215384615384615,-0.2,-0.184615384615385,-0.169230769230769,
-0.153846153846154,-0.138461538461538,-0.123076923076923,-0.107692307692308,
-0.0923076923076923,-0.0769230769230769,-0.0615384615384615,-0.0461538461538462,
-0.0307692307692308,-0.0153846153846154,0.),(-1.,1.),.UNSPECIFIED.)
GEOMETRIC_REPRESENTATION_ITEM()
RATIONAL_B_SPLINE_SURFACE(((1.,1.),(1.,1.),(1.,1.),(1.,1.),(1.,1.),(1.,
1.),(1.,1.),(1.,1.),(1.,1.),(1.,1.),(1.,1.),(1.,1.),(1.,1.),(1.,1.),(1.,
1.),(1.,1.),(1.,1.),(1.,1.),(1.,1.),(1.,1.),(1.,1.),(1.,1.),(1.,1.),(1.,
1.),(1.,1.),(1.,1.),(1.,1.),(1.,1.),(1.,1.),(1.,1.),(1.,1.),(1.,1.),(1.,
1.),(1.,1.),(1.,1.),(1.,1.),(1.,1.),(1.,1.),(1.,1.),(1.,1.),(1.,1.),(1.,
1.),(1.,1.),(1.,1.),(1.,1.),(1.,1.),(1.,1.),(1.,1.),(1.,1.),(1.,1.),(1.,
1.),(1.,1.),(1.,1.),(1.,1.),(1.,1.),(1.,1.),(1.,1.),(1.,1.),(1.,1.),(1.,
1.),(1.,1.),(1.,1.),(1.,1.),(1.,1.),(1.,1.),(1.,1.),(1.,1.),(1.,1.),(1.,
1.),(1.,1.)))
REPRESENTATION_ITEM('')
SURFACE()
);
#83=(
BOUNDED_SURFACE()
B_SPLINE_SURFACE(5,1,((#47040,#47041),(#47042,#47043),(#47044,#47045),(#47046,
#47047),(#47048,#47049),(#47050,#47051),(#47052,#47053),(#47054,#47055),
(#47056,#47057),(#47058,#47059),(#47060,#47061),(#47062,#47063),(#47064,
#47065),(#47066,#47067),(#47068,#47069),(#47070,#47071),(#47072,#47073),
(#47074,#47075),(#47076,#47077),(#47078,#47079),(#47080,#47081),(#47082,
#47083),(#47084,#47085),(#47086,#47087),(#47088,#47089),(#47090,#47091),
(#47092,#47093),(#47094,#47095),(#47096,#47097),(#47098,#47099),(#47100,
#47101),(#47102,#47103),(#47104,#47105),(#47106,#47107),(#47108,#47109),
(#47110,#47111),(#47112,#47113),(#47114,#47115),(#47116,#47117),(#47118,
#47119),(#47120,#47121),(#47122,#47123),(#47124,#47125),(#47126,#47127),
(#47128,#47129),(#47130,#47131),(#47132,#47133),(#47134,#47135),(#47136,
#47137),(#47138,#47139),(#47140,#47141),(#47142,#47143),(#47144,#47145),
(#47146,#47147),(#47148,#47149),(#47150,#47151),(#47152,#47153),(#47154,
#47155),(#47156,#47157),(#47158,#47159),(#47160,#47161),(#47162,#47163),
(#47164,#47165),(#47166,#47167),(#47168,#47169),(#47170,#47171),(#47172,
#47173),(#47174,#47175),(#47176,#47177),(#47178,#47179)),.UNSPECIFIED.,
 .F.,.F.,.F.)
B_SPLINE_SURFACE_WITH_KNOTS((6,1,1,1,1,1,1,1,1,1,1,1,1,1,1,1,1,1,1,1,1,
1,1,1,1,1,1,1,1,1,1,1,1,1,1,1,1,1,1,1,1,1,1,1,1,1,1,1,1,1,1,1,1,1,1,1,1,
1,1,1,1,1,1,1,1,6),(2,2),(-1.,-0.984615384615383,-0.969230769230768,-0.953846153846152,
-0.938461538461537,-0.923076923076922,-0.907692307692306,-0.892307692307691,
-0.876923076923076,-0.86153846153846,-0.846153846153845,-0.83076923076923,
-0.815384615384614,-0.799999999999999,-0.784615384615384,-0.769230769230768,
-0.753846153846153,-0.738461538461538,-0.723076923076922,-0.707692307692307,
-0.692307692307692,-0.676923076923076,-0.661538461538461,-0.646153846153846,
-0.63076923076923,-0.615384615384615,-0.6,-0.584615384615384,-0.569230769230769,
-0.553846153846154,-0.538461538461538,-0.523076923076923,-0.507692307692308,
-0.492307692307692,-0.476923076923077,-0.461538461538462,-0.446153846153846,
-0.430769230769231,-0.415384615384615,-0.4,-0.384615384615385,-0.369230769230769,
-0.353846153846154,-0.338461538461538,-0.323076923076923,-0.307692307692308,
-0.292307692307692,-0.276923076923077,-0.261538461538462,-0.246153846153846,
-0.230769230769231,-0.215384615384615,-0.2,-0.184615384615385,-0.169230769230769,
-0.153846153846154,-0.138461538461538,-0.123076923076923,-0.107692307692308,
-0.0923076923076923,-0.0769230769230769,-0.0615384615384615,-0.0461538461538462,
-0.0307692307692308,-0.0153846153846154,0.),(-1.,1.),.UNSPECIFIED.)
GEOMETRIC_REPRESENTATION_ITEM()
RATIONAL_B_SPLINE_SURFACE(((1.,1.),(1.,1.),(1.,1.),(1.,1.),(1.,1.),(1.,
1.),(1.,1.),(1.,1.),(1.,1.),(1.,1.),(1.,1.),(1.,1.),(1.,1.),(1.,1.),(1.,
1.),(1.,1.),(1.,1.),(1.,1.),(1.,1.),(1.,1.),(1.,1.),(1.,1.),(1.,1.),(1.,
1.),(1.,1.),(1.,1.),(1.,1.),(1.,1.),(1.,1.),(1.,1.),(1.,1.),(1.,1.),(1.,
1.),(1.,1.),(1.,1.),(1.,1.),(1.,1.),(1.,1.),(1.,1.),(1.,1.),(1.,1.),(1.,
1.),(1.,1.),(1.,1.),(1.,1.),(1.,1.),(1.,1.),(1.,1.),(1.,1.),(1.,1.),(1.,
1.),(1.,1.),(1.,1.),(1.,1.),(1.,1.),(1.,1.),(1.,1.),(1.,1.),(1.,1.),(1.,
1.),(1.,1.),(1.,1.),(1.,1.),(1.,1.),(1.,1.),(1.,1.),(1.,1.),(1.,1.),(1.,
1.),(1.,1.)))
REPRESENTATION_ITEM('')
SURFACE()
);
#84=(
BOUNDED_SURFACE()
B_SPLINE_SURFACE(5,1,((#47252,#47253),(#47254,#47255),(#47256,#47257),(#47258,
#47259),(#47260,#47261),(#47262,#47263),(#47264,#47265),(#47266,#47267),
(#47268,#47269),(#47270,#47271),(#47272,#47273),(#47274,#47275),(#47276,
#47277),(#47278,#47279),(#47280,#47281),(#47282,#47283),(#47284,#47285),
(#47286,#47287),(#47288,#47289),(#47290,#47291),(#47292,#47293),(#47294,
#47295),(#47296,#47297),(#47298,#47299),(#47300,#47301),(#47302,#47303),
(#47304,#47305),(#47306,#47307),(#47308,#47309),(#47310,#47311),(#47312,
#47313),(#47314,#47315),(#47316,#47317),(#47318,#47319),(#47320,#47321),
(#47322,#47323),(#47324,#47325),(#47326,#47327),(#47328,#47329),(#47330,
#47331),(#47332,#47333),(#47334,#47335),(#47336,#47337),(#47338,#47339),
(#47340,#47341),(#47342,#47343),(#47344,#47345),(#47346,#47347),(#47348,
#47349),(#47350,#47351),(#47352,#47353),(#47354,#47355),(#47356,#47357),
(#47358,#47359),(#47360,#47361),(#47362,#47363),(#47364,#47365),(#47366,
#47367),(#47368,#47369),(#47370,#47371),(#47372,#47373),(#47374,#47375),
(#47376,#47377),(#47378,#47379),(#47380,#47381),(#47382,#47383),(#47384,
#47385),(#47386,#47387),(#47388,#47389),(#47390,#47391)),.UNSPECIFIED.,
 .F.,.F.,.F.)
B_SPLINE_SURFACE_WITH_KNOTS((6,1,1,1,1,1,1,1,1,1,1,1,1,1,1,1,1,1,1,1,1,
1,1,1,1,1,1,1,1,1,1,1,1,1,1,1,1,1,1,1,1,1,1,1,1,1,1,1,1,1,1,1,1,1,1,1,1,
1,1,1,1,1,1,1,1,6),(2,2),(-1.,-0.984615384615383,-0.969230769230768,-0.953846153846152,
-0.938461538461537,-0.923076923076922,-0.907692307692306,-0.892307692307691,
-0.876923076923076,-0.86153846153846,-0.846153846153845,-0.83076923076923,
-0.815384615384614,-0.799999999999999,-0.784615384615384,-0.769230769230768,
-0.753846153846153,-0.738461538461538,-0.723076923076922,-0.707692307692307,
-0.692307692307692,-0.676923076923076,-0.661538461538461,-0.646153846153846,
-0.63076923076923,-0.615384615384615,-0.6,-0.584615384615384,-0.569230769230769,
-0.553846153846154,-0.538461538461538,-0.523076923076923,-0.507692307692308,
-0.492307692307692,-0.476923076923077,-0.461538461538462,-0.446153846153846,
-0.430769230769231,-0.415384615384615,-0.4,-0.384615384615385,-0.369230769230769,
-0.353846153846154,-0.338461538461538,-0.323076923076923,-0.307692307692308,
-0.292307692307692,-0.276923076923077,-0.261538461538462,-0.246153846153846,
-0.230769230769231,-0.215384615384615,-0.2,-0.184615384615385,-0.169230769230769,
-0.153846153846154,-0.138461538461538,-0.123076923076923,-0.107692307692308,
-0.0923076923076923,-0.0769230769230769,-0.0615384615384615,-0.0461538461538462,
-0.0307692307692308,-0.0153846153846154,0.),(-1.,1.),.UNSPECIFIED.)
GEOMETRIC_REPRESENTATION_ITEM()
RATIONAL_B_SPLINE_SURFACE(((1.,1.),(1.,1.),(1.,1.),(1.,1.),(1.,1.),(1.,
1.),(1.,1.),(1.,1.),(1.,1.),(1.,1.),(1.,1.),(1.,1.),(1.,1.),(1.,1.),(1.,
1.),(1.,1.),(1.,1.),(1.,1.),(1.,1.),(1.,1.),(1.,1.),(1.,1.),(1.,1.),(1.,
1.),(1.,1.),(1.,1.),(1.,1.),(1.,1.),(1.,1.),(1.,1.),(1.,1.),(1.,1.),(1.,
1.),(1.,1.),(1.,1.),(1.,1.),(1.,1.),(1.,1.),(1.,1.),(1.,1.),(1.,1.),(1.,
1.),(1.,1.),(1.,1.),(1.,1.),(1.,1.),(1.,1.),(1.,1.),(1.,1.),(1.,1.),(1.,
1.),(1.,1.),(1.,1.),(1.,1.),(1.,1.),(1.,1.),(1.,1.),(1.,1.),(1.,1.),(1.,
1.),(1.,1.),(1.,1.),(1.,1.),(1.,1.),(1.,1.),(1.,1.),(1.,1.),(1.,1.),(1.,
1.),(1.,1.)))
REPRESENTATION_ITEM('')
SURFACE()
);
#85=(
BOUNDED_SURFACE()
B_SPLINE_SURFACE(5,1,((#47482,#47483),(#47484,#47485),(#47486,#47487),(#47488,
#47489),(#47490,#47491),(#47492,#47493),(#47494,#47495),(#47496,#47497),
(#47498,#47499),(#47500,#47501),(#47502,#47503),(#47504,#47505),(#47506,
#47507),(#47508,#47509),(#47510,#47511),(#47512,#47513),(#47514,#47515),
(#47516,#47517),(#47518,#47519),(#47520,#47521),(#47522,#47523),(#47524,
#47525),(#47526,#47527),(#47528,#47529),(#47530,#47531),(#47532,#47533),
(#47534,#47535),(#47536,#47537),(#47538,#47539),(#47540,#47541),(#47542,
#47543),(#47544,#47545),(#47546,#47547),(#47548,#47549),(#47550,#47551),
(#47552,#47553),(#47554,#47555),(#47556,#47557),(#47558,#47559),(#47560,
#47561),(#47562,#47563),(#47564,#47565),(#47566,#47567),(#47568,#47569),
(#47570,#47571),(#47572,#47573),(#47574,#47575),(#47576,#47577),(#47578,
#47579),(#47580,#47581),(#47582,#47583),(#47584,#47585),(#47586,#47587),
(#47588,#47589),(#47590,#47591),(#47592,#47593),(#47594,#47595),(#47596,
#47597),(#47598,#47599),(#47600,#47601),(#47602,#47603),(#47604,#47605),
(#47606,#47607),(#47608,#47609),(#47610,#47611),(#47612,#47613),(#47614,
#47615),(#47616,#47617),(#47618,#47619),(#47620,#47621)),.UNSPECIFIED.,
 .F.,.F.,.F.)
B_SPLINE_SURFACE_WITH_KNOTS((6,1,1,1,1,1,1,1,1,1,1,1,1,1,1,1,1,1,1,1,1,
1,1,1,1,1,1,1,1,1,1,1,1,1,1,1,1,1,1,1,1,1,1,1,1,1,1,1,1,1,1,1,1,1,1,1,1,
1,1,1,1,1,1,1,1,6),(2,2),(-1.,-0.984615384615383,-0.969230769230768,-0.953846153846152,
-0.938461538461537,-0.923076923076922,-0.907692307692306,-0.892307692307691,
-0.876923076923076,-0.86153846153846,-0.846153846153845,-0.83076923076923,
-0.815384615384614,-0.799999999999999,-0.784615384615384,-0.769230769230768,
-0.753846153846153,-0.738461538461538,-0.723076923076922,-0.707692307692307,
-0.692307692307692,-0.676923076923076,-0.661538461538461,-0.646153846153846,
-0.63076923076923,-0.615384615384615,-0.6,-0.584615384615384,-0.569230769230769,
-0.553846153846154,-0.538461538461538,-0.523076923076923,-0.507692307692308,
-0.492307692307692,-0.476923076923077,-0.461538461538462,-0.446153846153846,
-0.430769230769231,-0.415384615384615,-0.4,-0.384615384615385,-0.369230769230769,
-0.353846153846154,-0.338461538461538,-0.323076923076923,-0.307692307692308,
-0.292307692307692,-0.276923076923077,-0.261538461538462,-0.246153846153846,
-0.230769230769231,-0.215384615384615,-0.2,-0.184615384615385,-0.169230769230769,
-0.153846153846154,-0.138461538461538,-0.123076923076923,-0.107692307692308,
-0.0923076923076923,-0.0769230769230769,-0.0615384615384615,-0.0461538461538462,
-0.0307692307692308,-0.0153846153846154,0.),(-1.,1.),.UNSPECIFIED.)
GEOMETRIC_REPRESENTATION_ITEM()
RATIONAL_B_SPLINE_SURFACE(((1.,1.),(1.,1.),(1.,1.),(1.,1.),(1.,1.),(1.,
1.),(1.,1.),(1.,1.),(1.,1.),(1.,1.),(1.,1.),(1.,1.),(1.,1.),(1.,1.),(1.,
1.),(1.,1.),(1.,1.),(1.,1.),(1.,1.),(1.,1.),(1.,1.),(1.,1.),(1.,1.),(1.,
1.),(1.,1.),(1.,1.),(1.,1.),(1.,1.),(1.,1.),(1.,1.),(1.,1.),(1.,1.),(1.,
1.),(1.,1.),(1.,1.),(1.,1.),(1.,1.),(1.,1.),(1.,1.),(1.,1.),(1.,1.),(1.,
1.),(1.,1.),(1.,1.),(1.,1.),(1.,1.),(1.,1.),(1.,1.),(1.,1.),(1.,1.),(1.,
1.),(1.,1.),(1.,1.),(1.,1.),(1.,1.),(1.,1.),(1.,1.),(1.,1.),(1.,1.),(1.,
1.),(1.,1.),(1.,1.),(1.,1.),(1.,1.),(1.,1.),(1.,1.),(1.,1.),(1.,1.),(1.,
1.),(1.,1.)))
REPRESENTATION_ITEM('')
SURFACE()
);
#86=(
BOUNDED_SURFACE()
B_SPLINE_SURFACE(5,1,((#47694,#47695),(#47696,#47697),(#47698,#47699),(#47700,
#47701),(#47702,#47703),(#47704,#47705),(#47706,#47707),(#47708,#47709),
(#47710,#47711),(#47712,#47713),(#47714,#47715),(#47716,#47717),(#47718,
#47719),(#47720,#47721),(#47722,#47723),(#47724,#47725),(#47726,#47727),
(#47728,#47729),(#47730,#47731),(#47732,#47733),(#47734,#47735),(#47736,
#47737),(#47738,#47739),(#47740,#47741),(#47742,#47743),(#47744,#47745),
(#47746,#47747),(#47748,#47749),(#47750,#47751),(#47752,#47753),(#47754,
#47755),(#47756,#47757),(#47758,#47759),(#47760,#47761),(#47762,#47763),
(#47764,#47765),(#47766,#47767),(#47768,#47769),(#47770,#47771),(#47772,
#47773),(#47774,#47775),(#47776,#47777),(#47778,#47779),(#47780,#47781),
(#47782,#47783),(#47784,#47785),(#47786,#47787),(#47788,#47789),(#47790,
#47791),(#47792,#47793),(#47794,#47795),(#47796,#47797),(#47798,#47799),
(#47800,#47801),(#47802,#47803),(#47804,#47805),(#47806,#47807),(#47808,
#47809),(#47810,#47811),(#47812,#47813),(#47814,#47815),(#47816,#47817),
(#47818,#47819),(#47820,#47821),(#47822,#47823),(#47824,#47825),(#47826,
#47827),(#47828,#47829),(#47830,#47831),(#47832,#47833)),.UNSPECIFIED.,
 .F.,.F.,.F.)
B_SPLINE_SURFACE_WITH_KNOTS((6,1,1,1,1,1,1,1,1,1,1,1,1,1,1,1,1,1,1,1,1,
1,1,1,1,1,1,1,1,1,1,1,1,1,1,1,1,1,1,1,1,1,1,1,1,1,1,1,1,1,1,1,1,1,1,1,1,
1,1,1,1,1,1,1,1,6),(2,2),(-1.,-0.984615384615383,-0.969230769230768,-0.953846153846152,
-0.938461538461537,-0.923076923076922,-0.907692307692306,-0.892307692307691,
-0.876923076923076,-0.86153846153846,-0.846153846153845,-0.83076923076923,
-0.815384615384614,-0.799999999999999,-0.784615384615384,-0.769230769230768,
-0.753846153846153,-0.738461538461538,-0.723076923076922,-0.707692307692307,
-0.692307692307692,-0.676923076923076,-0.661538461538461,-0.646153846153846,
-0.63076923076923,-0.615384615384615,-0.6,-0.584615384615384,-0.569230769230769,
-0.553846153846154,-0.538461538461538,-0.523076923076923,-0.507692307692308,
-0.492307692307692,-0.476923076923077,-0.461538461538462,-0.446153846153846,
-0.430769230769231,-0.415384615384615,-0.4,-0.384615384615385,-0.369230769230769,
-0.353846153846154,-0.338461538461538,-0.323076923076923,-0.307692307692308,
-0.292307692307692,-0.276923076923077,-0.261538461538462,-0.246153846153846,
-0.230769230769231,-0.215384615384615,-0.2,-0.184615384615385,-0.169230769230769,
-0.153846153846154,-0.138461538461538,-0.123076923076923,-0.107692307692308,
-0.0923076923076923,-0.0769230769230769,-0.0615384615384615,-0.0461538461538462,
-0.0307692307692308,-0.0153846153846154,0.),(-1.,1.),.UNSPECIFIED.)
GEOMETRIC_REPRESENTATION_ITEM()
RATIONAL_B_SPLINE_SURFACE(((1.,1.),(1.,1.),(1.,1.),(1.,1.),(1.,1.),(1.,
1.),(1.,1.),(1.,1.),(1.,1.),(1.,1.),(1.,1.),(1.,1.),(1.,1.),(1.,1.),(1.,
1.),(1.,1.),(1.,1.),(1.,1.),(1.,1.),(1.,1.),(1.,1.),(1.,1.),(1.,1.),(1.,
1.),(1.,1.),(1.,1.),(1.,1.),(1.,1.),(1.,1.),(1.,1.),(1.,1.),(1.,1.),(1.,
1.),(1.,1.),(1.,1.),(1.,1.),(1.,1.),(1.,1.),(1.,1.),(1.,1.),(1.,1.),(1.,
1.),(1.,1.),(1.,1.),(1.,1.),(1.,1.),(1.,1.),(1.,1.),(1.,1.),(1.,1.),(1.,
1.),(1.,1.),(1.,1.),(1.,1.),(1.,1.),(1.,1.),(1.,1.),(1.,1.),(1.,1.),(1.,
1.),(1.,1.),(1.,1.),(1.,1.),(1.,1.),(1.,1.),(1.,1.),(1.,1.),(1.,1.),(1.,
1.),(1.,1.)))
REPRESENTATION_ITEM('')
SURFACE()
);
#87=(
BOUNDED_SURFACE()
B_SPLINE_SURFACE(5,1,((#47924,#47925),(#47926,#47927),(#47928,#47929),(#47930,
#47931),(#47932,#47933),(#47934,#47935),(#47936,#47937),(#47938,#47939),
(#47940,#47941),(#47942,#47943),(#47944,#47945),(#47946,#47947),(#47948,
#47949),(#47950,#47951),(#47952,#47953),(#47954,#47955),(#47956,#47957),
(#47958,#47959),(#47960,#47961),(#47962,#47963),(#47964,#47965),(#47966,
#47967),(#47968,#47969),(#47970,#47971),(#47972,#47973),(#47974,#47975),
(#47976,#47977),(#47978,#47979),(#47980,#47981),(#47982,#47983),(#47984,
#47985),(#47986,#47987),(#47988,#47989),(#47990,#47991),(#47992,#47993),
(#47994,#47995),(#47996,#47997),(#47998,#47999),(#48000,#48001),(#48002,
#48003),(#48004,#48005),(#48006,#48007),(#48008,#48009),(#48010,#48011),
(#48012,#48013),(#48014,#48015),(#48016,#48017),(#48018,#48019),(#48020,
#48021),(#48022,#48023),(#48024,#48025),(#48026,#48027),(#48028,#48029),
(#48030,#48031),(#48032,#48033),(#48034,#48035),(#48036,#48037),(#48038,
#48039),(#48040,#48041),(#48042,#48043),(#48044,#48045),(#48046,#48047),
(#48048,#48049),(#48050,#48051),(#48052,#48053),(#48054,#48055),(#48056,
#48057),(#48058,#48059),(#48060,#48061),(#48062,#48063)),.UNSPECIFIED.,
 .F.,.F.,.F.)
B_SPLINE_SURFACE_WITH_KNOTS((6,1,1,1,1,1,1,1,1,1,1,1,1,1,1,1,1,1,1,1,1,
1,1,1,1,1,1,1,1,1,1,1,1,1,1,1,1,1,1,1,1,1,1,1,1,1,1,1,1,1,1,1,1,1,1,1,1,
1,1,1,1,1,1,1,1,6),(2,2),(-1.,-0.984615384615383,-0.969230769230768,-0.953846153846152,
-0.938461538461537,-0.923076923076922,-0.907692307692306,-0.892307692307691,
-0.876923076923076,-0.86153846153846,-0.846153846153845,-0.83076923076923,
-0.815384615384614,-0.799999999999999,-0.784615384615384,-0.769230769230768,
-0.753846153846153,-0.738461538461538,-0.723076923076922,-0.707692307692307,
-0.692307692307692,-0.676923076923076,-0.661538461538461,-0.646153846153846,
-0.63076923076923,-0.615384615384615,-0.6,-0.584615384615384,-0.569230769230769,
-0.553846153846154,-0.538461538461538,-0.523076923076923,-0.507692307692308,
-0.492307692307692,-0.476923076923077,-0.461538461538462,-0.446153846153846,
-0.430769230769231,-0.415384615384615,-0.4,-0.384615384615385,-0.369230769230769,
-0.353846153846154,-0.338461538461538,-0.323076923076923,-0.307692307692308,
-0.292307692307692,-0.276923076923077,-0.261538461538462,-0.246153846153846,
-0.230769230769231,-0.215384615384615,-0.2,-0.184615384615385,-0.169230769230769,
-0.153846153846154,-0.138461538461538,-0.123076923076923,-0.107692307692308,
-0.0923076923076923,-0.0769230769230769,-0.0615384615384615,-0.0461538461538462,
-0.0307692307692308,-0.0153846153846154,0.),(-1.,1.),.UNSPECIFIED.)
GEOMETRIC_REPRESENTATION_ITEM()
RATIONAL_B_SPLINE_SURFACE(((1.,1.),(1.,1.),(1.,1.),(1.,1.),(1.,1.),(1.,
1.),(1.,1.),(1.,1.),(1.,1.),(1.,1.),(1.,1.),(1.,1.),(1.,1.),(1.,1.),(1.,
1.),(1.,1.),(1.,1.),(1.,1.),(1.,1.),(1.,1.),(1.,1.),(1.,1.),(1.,1.),(1.,
1.),(1.,1.),(1.,1.),(1.,1.),(1.,1.),(1.,1.),(1.,1.),(1.,1.),(1.,1.),(1.,
1.),(1.,1.),(1.,1.),(1.,1.),(1.,1.),(1.,1.),(1.,1.),(1.,1.),(1.,1.),(1.,
1.),(1.,1.),(1.,1.),(1.,1.),(1.,1.),(1.,1.),(1.,1.),(1.,1.),(1.,1.),(1.,
1.),(1.,1.),(1.,1.),(1.,1.),(1.,1.),(1.,1.),(1.,1.),(1.,1.),(1.,1.),(1.,
1.),(1.,1.),(1.,1.),(1.,1.),(1.,1.),(1.,1.),(1.,1.),(1.,1.),(1.,1.),(1.,
1.),(1.,1.)))
REPRESENTATION_ITEM('')
SURFACE()
);
#88=(
BOUNDED_SURFACE()
B_SPLINE_SURFACE(5,1,((#48136,#48137),(#48138,#48139),(#48140,#48141),(#48142,
#48143),(#48144,#48145),(#48146,#48147),(#48148,#48149),(#48150,#48151),
(#48152,#48153),(#48154,#48155),(#48156,#48157),(#48158,#48159),(#48160,
#48161),(#48162,#48163),(#48164,#48165),(#48166,#48167),(#48168,#48169),
(#48170,#48171),(#48172,#48173),(#48174,#48175),(#48176,#48177),(#48178,
#48179),(#48180,#48181),(#48182,#48183),(#48184,#48185),(#48186,#48187),
(#48188,#48189),(#48190,#48191),(#48192,#48193),(#48194,#48195),(#48196,
#48197),(#48198,#48199),(#48200,#48201),(#48202,#48203),(#48204,#48205),
(#48206,#48207),(#48208,#48209),(#48210,#48211),(#48212,#48213),(#48214,
#48215),(#48216,#48217),(#48218,#48219),(#48220,#48221),(#48222,#48223),
(#48224,#48225),(#48226,#48227),(#48228,#48229),(#48230,#48231),(#48232,
#48233),(#48234,#48235),(#48236,#48237),(#48238,#48239),(#48240,#48241),
(#48242,#48243),(#48244,#48245),(#48246,#48247),(#48248,#48249),(#48250,
#48251),(#48252,#48253),(#48254,#48255),(#48256,#48257),(#48258,#48259),
(#48260,#48261),(#48262,#48263),(#48264,#48265),(#48266,#48267),(#48268,
#48269),(#48270,#48271),(#48272,#48273),(#48274,#48275)),.UNSPECIFIED.,
 .F.,.F.,.F.)
B_SPLINE_SURFACE_WITH_KNOTS((6,1,1,1,1,1,1,1,1,1,1,1,1,1,1,1,1,1,1,1,1,
1,1,1,1,1,1,1,1,1,1,1,1,1,1,1,1,1,1,1,1,1,1,1,1,1,1,1,1,1,1,1,1,1,1,1,1,
1,1,1,1,1,1,1,1,6),(2,2),(-1.,-0.984615384615383,-0.969230769230768,-0.953846153846152,
-0.938461538461537,-0.923076923076922,-0.907692307692306,-0.892307692307691,
-0.876923076923076,-0.86153846153846,-0.846153846153845,-0.83076923076923,
-0.815384615384614,-0.799999999999999,-0.784615384615384,-0.769230769230768,
-0.753846153846153,-0.738461538461538,-0.723076923076922,-0.707692307692307,
-0.692307692307692,-0.676923076923076,-0.661538461538461,-0.646153846153846,
-0.63076923076923,-0.615384615384615,-0.6,-0.584615384615384,-0.569230769230769,
-0.553846153846154,-0.538461538461538,-0.523076923076923,-0.507692307692308,
-0.492307692307692,-0.476923076923077,-0.461538461538462,-0.446153846153846,
-0.430769230769231,-0.415384615384615,-0.4,-0.384615384615385,-0.369230769230769,
-0.353846153846154,-0.338461538461538,-0.323076923076923,-0.307692307692308,
-0.292307692307692,-0.276923076923077,-0.261538461538462,-0.246153846153846,
-0.230769230769231,-0.215384615384615,-0.2,-0.184615384615385,-0.169230769230769,
-0.153846153846154,-0.138461538461538,-0.123076923076923,-0.107692307692308,
-0.0923076923076923,-0.0769230769230769,-0.0615384615384615,-0.0461538461538462,
-0.0307692307692308,-0.0153846153846154,0.),(-1.,1.),.UNSPECIFIED.)
GEOMETRIC_REPRESENTATION_ITEM()
RATIONAL_B_SPLINE_SURFACE(((1.,1.),(1.,1.),(1.,1.),(1.,1.),(1.,1.),(1.,
1.),(1.,1.),(1.,1.),(1.,1.),(1.,1.),(1.,1.),(1.,1.),(1.,1.),(1.,1.),(1.,
1.),(1.,1.),(1.,1.),(1.,1.),(1.,1.),(1.,1.),(1.,1.),(1.,1.),(1.,1.),(1.,
1.),(1.,1.),(1.,1.),(1.,1.),(1.,1.),(1.,1.),(1.,1.),(1.,1.),(1.,1.),(1.,
1.),(1.,1.),(1.,1.),(1.,1.),(1.,1.),(1.,1.),(1.,1.),(1.,1.),(1.,1.),(1.,
1.),(1.,1.),(1.,1.),(1.,1.),(1.,1.),(1.,1.),(1.,1.),(1.,1.),(1.,1.),(1.,
1.),(1.,1.),(1.,1.),(1.,1.),(1.,1.),(1.,1.),(1.,1.),(1.,1.),(1.,1.),(1.,
1.),(1.,1.),(1.,1.),(1.,1.),(1.,1.),(1.,1.),(1.,1.),(1.,1.),(1.,1.),(1.,
1.),(1.,1.)))
REPRESENTATION_ITEM('')
SURFACE()
);
#89=(
BOUNDED_SURFACE()
B_SPLINE_SURFACE(5,1,((#48366,#48367),(#48368,#48369),(#48370,#48371),(#48372,
#48373),(#48374,#48375),(#48376,#48377),(#48378,#48379),(#48380,#48381),
(#48382,#48383),(#48384,#48385),(#48386,#48387),(#48388,#48389),(#48390,
#48391),(#48392,#48393),(#48394,#48395),(#48396,#48397),(#48398,#48399),
(#48400,#48401),(#48402,#48403),(#48404,#48405),(#48406,#48407),(#48408,
#48409),(#48410,#48411),(#48412,#48413),(#48414,#48415),(#48416,#48417),
(#48418,#48419),(#48420,#48421),(#48422,#48423),(#48424,#48425),(#48426,
#48427),(#48428,#48429),(#48430,#48431),(#48432,#48433),(#48434,#48435),
(#48436,#48437),(#48438,#48439),(#48440,#48441),(#48442,#48443),(#48444,
#48445),(#48446,#48447),(#48448,#48449),(#48450,#48451),(#48452,#48453),
(#48454,#48455),(#48456,#48457),(#48458,#48459),(#48460,#48461),(#48462,
#48463),(#48464,#48465),(#48466,#48467),(#48468,#48469),(#48470,#48471),
(#48472,#48473),(#48474,#48475),(#48476,#48477),(#48478,#48479),(#48480,
#48481),(#48482,#48483),(#48484,#48485),(#48486,#48487),(#48488,#48489),
(#48490,#48491),(#48492,#48493),(#48494,#48495),(#48496,#48497),(#48498,
#48499),(#48500,#48501),(#48502,#48503),(#48504,#48505)),.UNSPECIFIED.,
 .F.,.F.,.F.)
B_SPLINE_SURFACE_WITH_KNOTS((6,1,1,1,1,1,1,1,1,1,1,1,1,1,1,1,1,1,1,1,1,
1,1,1,1,1,1,1,1,1,1,1,1,1,1,1,1,1,1,1,1,1,1,1,1,1,1,1,1,1,1,1,1,1,1,1,1,
1,1,1,1,1,1,1,1,6),(2,2),(-1.,-0.984615384615383,-0.969230769230768,-0.953846153846152,
-0.938461538461537,-0.923076923076922,-0.907692307692306,-0.892307692307691,
-0.876923076923076,-0.86153846153846,-0.846153846153845,-0.83076923076923,
-0.815384615384614,-0.799999999999999,-0.784615384615384,-0.769230769230768,
-0.753846153846153,-0.738461538461538,-0.723076923076922,-0.707692307692307,
-0.692307692307692,-0.676923076923076,-0.661538461538461,-0.646153846153846,
-0.63076923076923,-0.615384615384615,-0.6,-0.584615384615384,-0.569230769230769,
-0.553846153846154,-0.538461538461538,-0.523076923076923,-0.507692307692308,
-0.492307692307692,-0.476923076923077,-0.461538461538462,-0.446153846153846,
-0.430769230769231,-0.415384615384615,-0.4,-0.384615384615385,-0.369230769230769,
-0.353846153846154,-0.338461538461538,-0.323076923076923,-0.307692307692308,
-0.292307692307692,-0.276923076923077,-0.261538461538462,-0.246153846153846,
-0.230769230769231,-0.215384615384615,-0.2,-0.184615384615385,-0.169230769230769,
-0.153846153846154,-0.138461538461538,-0.123076923076923,-0.107692307692308,
-0.0923076923076923,-0.0769230769230769,-0.0615384615384615,-0.0461538461538462,
-0.0307692307692308,-0.0153846153846154,0.),(-1.,1.),.UNSPECIFIED.)
GEOMETRIC_REPRESENTATION_ITEM()
RATIONAL_B_SPLINE_SURFACE(((1.,1.),(1.,1.),(1.,1.),(1.,1.),(1.,1.),(1.,
1.),(1.,1.),(1.,1.),(1.,1.),(1.,1.),(1.,1.),(1.,1.),(1.,1.),(1.,1.),(1.,
1.),(1.,1.),(1.,1.),(1.,1.),(1.,1.),(1.,1.),(1.,1.),(1.,1.),(1.,1.),(1.,
1.),(1.,1.),(1.,1.),(1.,1.),(1.,1.),(1.,1.),(1.,1.),(1.,1.),(1.,1.),(1.,
1.),(1.,1.),(1.,1.),(1.,1.),(1.,1.),(1.,1.),(1.,1.),(1.,1.),(1.,1.),(1.,
1.),(1.,1.),(1.,1.),(1.,1.),(1.,1.),(1.,1.),(1.,1.),(1.,1.),(1.,1.),(1.,
1.),(1.,1.),(1.,1.),(1.,1.),(1.,1.),(1.,1.),(1.,1.),(1.,1.),(1.,1.),(1.,
1.),(1.,1.),(1.,1.),(1.,1.),(1.,1.),(1.,1.),(1.,1.),(1.,1.),(1.,1.),(1.,
1.),(1.,1.)))
REPRESENTATION_ITEM('')
SURFACE()
);
#90=(
BOUNDED_SURFACE()
B_SPLINE_SURFACE(5,1,((#48578,#48579),(#48580,#48581),(#48582,#48583),(#48584,
#48585),(#48586,#48587),(#48588,#48589),(#48590,#48591),(#48592,#48593),
(#48594,#48595),(#48596,#48597),(#48598,#48599),(#48600,#48601),(#48602,
#48603),(#48604,#48605),(#48606,#48607),(#48608,#48609),(#48610,#48611),
(#48612,#48613),(#48614,#48615),(#48616,#48617),(#48618,#48619),(#48620,
#48621),(#48622,#48623),(#48624,#48625),(#48626,#48627),(#48628,#48629),
(#48630,#48631),(#48632,#48633),(#48634,#48635),(#48636,#48637),(#48638,
#48639),(#48640,#48641),(#48642,#48643),(#48644,#48645),(#48646,#48647),
(#48648,#48649),(#48650,#48651),(#48652,#48653),(#48654,#48655),(#48656,
#48657),(#48658,#48659),(#48660,#48661),(#48662,#48663),(#48664,#48665),
(#48666,#48667),(#48668,#48669),(#48670,#48671),(#48672,#48673),(#48674,
#48675),(#48676,#48677),(#48678,#48679),(#48680,#48681),(#48682,#48683),
(#48684,#48685),(#48686,#48687),(#48688,#48689),(#48690,#48691),(#48692,
#48693),(#48694,#48695),(#48696,#48697),(#48698,#48699),(#48700,#48701),
(#48702,#48703),(#48704,#48705),(#48706,#48707),(#48708,#48709),(#48710,
#48711),(#48712,#48713),(#48714,#48715),(#48716,#48717)),.UNSPECIFIED.,
 .F.,.F.,.F.)
B_SPLINE_SURFACE_WITH_KNOTS((6,1,1,1,1,1,1,1,1,1,1,1,1,1,1,1,1,1,1,1,1,
1,1,1,1,1,1,1,1,1,1,1,1,1,1,1,1,1,1,1,1,1,1,1,1,1,1,1,1,1,1,1,1,1,1,1,1,
1,1,1,1,1,1,1,1,6),(2,2),(-1.,-0.984615384615383,-0.969230769230768,-0.953846153846152,
-0.938461538461537,-0.923076923076922,-0.907692307692306,-0.892307692307691,
-0.876923076923076,-0.86153846153846,-0.846153846153845,-0.83076923076923,
-0.815384615384614,-0.799999999999999,-0.784615384615384,-0.769230769230768,
-0.753846153846153,-0.738461538461538,-0.723076923076922,-0.707692307692307,
-0.692307692307692,-0.676923076923076,-0.661538461538461,-0.646153846153846,
-0.63076923076923,-0.615384615384615,-0.6,-0.584615384615384,-0.569230769230769,
-0.553846153846154,-0.538461538461538,-0.523076923076923,-0.507692307692308,
-0.492307692307692,-0.476923076923077,-0.461538461538462,-0.446153846153846,
-0.430769230769231,-0.415384615384615,-0.4,-0.384615384615385,-0.369230769230769,
-0.353846153846154,-0.338461538461538,-0.323076923076923,-0.307692307692308,
-0.292307692307692,-0.276923076923077,-0.261538461538462,-0.246153846153846,
-0.230769230769231,-0.215384615384615,-0.2,-0.184615384615385,-0.169230769230769,
-0.153846153846154,-0.138461538461538,-0.123076923076923,-0.107692307692308,
-0.0923076923076923,-0.0769230769230769,-0.0615384615384615,-0.0461538461538462,
-0.0307692307692308,-0.0153846153846154,0.),(-1.,1.),.UNSPECIFIED.)
GEOMETRIC_REPRESENTATION_ITEM()
RATIONAL_B_SPLINE_SURFACE(((1.,1.),(1.,1.),(1.,1.),(1.,1.),(1.,1.),(1.,
1.),(1.,1.),(1.,1.),(1.,1.),(1.,1.),(1.,1.),(1.,1.),(1.,1.),(1.,1.),(1.,
1.),(1.,1.),(1.,1.),(1.,1.),(1.,1.),(1.,1.),(1.,1.),(1.,1.),(1.,1.),(1.,
1.),(1.,1.),(1.,1.),(1.,1.),(1.,1.),(1.,1.),(1.,1.),(1.,1.),(1.,1.),(1.,
1.),(1.,1.),(1.,1.),(1.,1.),(1.,1.),(1.,1.),(1.,1.),(1.,1.),(1.,1.),(1.,
1.),(1.,1.),(1.,1.),(1.,1.),(1.,1.),(1.,1.),(1.,1.),(1.,1.),(1.,1.),(1.,
1.),(1.,1.),(1.,1.),(1.,1.),(1.,1.),(1.,1.),(1.,1.),(1.,1.),(1.,1.),(1.,
1.),(1.,1.),(1.,1.),(1.,1.),(1.,1.),(1.,1.),(1.,1.),(1.,1.),(1.,1.),(1.,
1.),(1.,1.)))
REPRESENTATION_ITEM('')
SURFACE()
);
#91=(
BOUNDED_SURFACE()
B_SPLINE_SURFACE(5,1,((#48808,#48809),(#48810,#48811),(#48812,#48813),(#48814,
#48815),(#48816,#48817),(#48818,#48819),(#48820,#48821),(#48822,#48823),
(#48824,#48825),(#48826,#48827),(#48828,#48829),(#48830,#48831),(#48832,
#48833),(#48834,#48835),(#48836,#48837),(#48838,#48839),(#48840,#48841),
(#48842,#48843),(#48844,#48845),(#48846,#48847),(#48848,#48849),(#48850,
#48851),(#48852,#48853),(#48854,#48855),(#48856,#48857),(#48858,#48859),
(#48860,#48861),(#48862,#48863),(#48864,#48865),(#48866,#48867),(#48868,
#48869),(#48870,#48871),(#48872,#48873),(#48874,#48875),(#48876,#48877),
(#48878,#48879),(#48880,#48881),(#48882,#48883),(#48884,#48885),(#48886,
#48887),(#48888,#48889),(#48890,#48891),(#48892,#48893),(#48894,#48895),
(#48896,#48897),(#48898,#48899),(#48900,#48901),(#48902,#48903),(#48904,
#48905),(#48906,#48907),(#48908,#48909),(#48910,#48911),(#48912,#48913),
(#48914,#48915),(#48916,#48917),(#48918,#48919),(#48920,#48921),(#48922,
#48923),(#48924,#48925),(#48926,#48927),(#48928,#48929),(#48930,#48931),
(#48932,#48933),(#48934,#48935),(#48936,#48937),(#48938,#48939),(#48940,
#48941),(#48942,#48943),(#48944,#48945),(#48946,#48947)),.UNSPECIFIED.,
 .F.,.F.,.F.)
B_SPLINE_SURFACE_WITH_KNOTS((6,1,1,1,1,1,1,1,1,1,1,1,1,1,1,1,1,1,1,1,1,
1,1,1,1,1,1,1,1,1,1,1,1,1,1,1,1,1,1,1,1,1,1,1,1,1,1,1,1,1,1,1,1,1,1,1,1,
1,1,1,1,1,1,1,1,6),(2,2),(-1.,-0.984615384615383,-0.969230769230768,-0.953846153846152,
-0.938461538461537,-0.923076923076922,-0.907692307692306,-0.892307692307691,
-0.876923076923076,-0.86153846153846,-0.846153846153845,-0.83076923076923,
-0.815384615384614,-0.799999999999999,-0.784615384615384,-0.769230769230768,
-0.753846153846153,-0.738461538461538,-0.723076923076922,-0.707692307692307,
-0.692307692307692,-0.676923076923076,-0.661538461538461,-0.646153846153846,
-0.63076923076923,-0.615384615384615,-0.6,-0.584615384615384,-0.569230769230769,
-0.553846153846154,-0.538461538461538,-0.523076923076923,-0.507692307692308,
-0.492307692307692,-0.476923076923077,-0.461538461538462,-0.446153846153846,
-0.430769230769231,-0.415384615384615,-0.4,-0.384615384615385,-0.369230769230769,
-0.353846153846154,-0.338461538461538,-0.323076923076923,-0.307692307692308,
-0.292307692307692,-0.276923076923077,-0.261538461538462,-0.246153846153846,
-0.230769230769231,-0.215384615384615,-0.2,-0.184615384615385,-0.169230769230769,
-0.153846153846154,-0.138461538461538,-0.123076923076923,-0.107692307692308,
-0.0923076923076923,-0.0769230769230769,-0.0615384615384615,-0.0461538461538462,
-0.0307692307692308,-0.0153846153846154,0.),(-1.,1.),.UNSPECIFIED.)
GEOMETRIC_REPRESENTATION_ITEM()
RATIONAL_B_SPLINE_SURFACE(((1.,1.),(1.,1.),(1.,1.),(1.,1.),(1.,1.),(1.,
1.),(1.,1.),(1.,1.),(1.,1.),(1.,1.),(1.,1.),(1.,1.),(1.,1.),(1.,1.),(1.,
1.),(1.,1.),(1.,1.),(1.,1.),(1.,1.),(1.,1.),(1.,1.),(1.,1.),(1.,1.),(1.,
1.),(1.,1.),(1.,1.),(1.,1.),(1.,1.),(1.,1.),(1.,1.),(1.,1.),(1.,1.),(1.,
1.),(1.,1.),(1.,1.),(1.,1.),(1.,1.),(1.,1.),(1.,1.),(1.,1.),(1.,1.),(1.,
1.),(1.,1.),(1.,1.),(1.,1.),(1.,1.),(1.,1.),(1.,1.),(1.,1.),(1.,1.),(1.,
1.),(1.,1.),(1.,1.),(1.,1.),(1.,1.),(1.,1.),(1.,1.),(1.,1.),(1.,1.),(1.,
1.),(1.,1.),(1.,1.),(1.,1.),(1.,1.),(1.,1.),(1.,1.),(1.,1.),(1.,1.),(1.,
1.),(1.,1.)))
REPRESENTATION_ITEM('')
SURFACE()
);
#92=(
BOUNDED_SURFACE()
B_SPLINE_SURFACE(5,1,((#49020,#49021),(#49022,#49023),(#49024,#49025),(#49026,
#49027),(#49028,#49029),(#49030,#49031),(#49032,#49033),(#49034,#49035),
(#49036,#49037),(#49038,#49039),(#49040,#49041),(#49042,#49043),(#49044,
#49045),(#49046,#49047),(#49048,#49049),(#49050,#49051),(#49052,#49053),
(#49054,#49055),(#49056,#49057),(#49058,#49059),(#49060,#49061),(#49062,
#49063),(#49064,#49065),(#49066,#49067),(#49068,#49069),(#49070,#49071),
(#49072,#49073),(#49074,#49075),(#49076,#49077),(#49078,#49079),(#49080,
#49081),(#49082,#49083),(#49084,#49085),(#49086,#49087),(#49088,#49089),
(#49090,#49091),(#49092,#49093),(#49094,#49095),(#49096,#49097),(#49098,
#49099),(#49100,#49101),(#49102,#49103),(#49104,#49105),(#49106,#49107),
(#49108,#49109),(#49110,#49111),(#49112,#49113),(#49114,#49115),(#49116,
#49117),(#49118,#49119),(#49120,#49121),(#49122,#49123),(#49124,#49125),
(#49126,#49127),(#49128,#49129),(#49130,#49131),(#49132,#49133),(#49134,
#49135),(#49136,#49137),(#49138,#49139),(#49140,#49141),(#49142,#49143),
(#49144,#49145),(#49146,#49147),(#49148,#49149),(#49150,#49151),(#49152,
#49153),(#49154,#49155),(#49156,#49157),(#49158,#49159)),.UNSPECIFIED.,
 .F.,.F.,.F.)
B_SPLINE_SURFACE_WITH_KNOTS((6,1,1,1,1,1,1,1,1,1,1,1,1,1,1,1,1,1,1,1,1,
1,1,1,1,1,1,1,1,1,1,1,1,1,1,1,1,1,1,1,1,1,1,1,1,1,1,1,1,1,1,1,1,1,1,1,1,
1,1,1,1,1,1,1,1,6),(2,2),(-1.,-0.984615384615383,-0.969230769230768,-0.953846153846152,
-0.938461538461537,-0.923076923076922,-0.907692307692306,-0.892307692307691,
-0.876923076923076,-0.86153846153846,-0.846153846153845,-0.83076923076923,
-0.815384615384614,-0.799999999999999,-0.784615384615384,-0.769230769230768,
-0.753846153846153,-0.738461538461538,-0.723076923076922,-0.707692307692307,
-0.692307692307692,-0.676923076923076,-0.661538461538461,-0.646153846153846,
-0.63076923076923,-0.615384615384615,-0.6,-0.584615384615384,-0.569230769230769,
-0.553846153846154,-0.538461538461538,-0.523076923076923,-0.507692307692308,
-0.492307692307692,-0.476923076923077,-0.461538461538462,-0.446153846153846,
-0.430769230769231,-0.415384615384615,-0.4,-0.384615384615385,-0.369230769230769,
-0.353846153846154,-0.338461538461538,-0.323076923076923,-0.307692307692308,
-0.292307692307692,-0.276923076923077,-0.261538461538462,-0.246153846153846,
-0.230769230769231,-0.215384615384615,-0.2,-0.184615384615385,-0.169230769230769,
-0.153846153846154,-0.138461538461538,-0.123076923076923,-0.107692307692308,
-0.0923076923076923,-0.0769230769230769,-0.0615384615384615,-0.0461538461538462,
-0.0307692307692308,-0.0153846153846154,0.),(-1.,1.),.UNSPECIFIED.)
GEOMETRIC_REPRESENTATION_ITEM()
RATIONAL_B_SPLINE_SURFACE(((1.,1.),(1.,1.),(1.,1.),(1.,1.),(1.,1.),(1.,
1.),(1.,1.),(1.,1.),(1.,1.),(1.,1.),(1.,1.),(1.,1.),(1.,1.),(1.,1.),(1.,
1.),(1.,1.),(1.,1.),(1.,1.),(1.,1.),(1.,1.),(1.,1.),(1.,1.),(1.,1.),(1.,
1.),(1.,1.),(1.,1.),(1.,1.),(1.,1.),(1.,1.),(1.,1.),(1.,1.),(1.,1.),(1.,
1.),(1.,1.),(1.,1.),(1.,1.),(1.,1.),(1.,1.),(1.,1.),(1.,1.),(1.,1.),(1.,
1.),(1.,1.),(1.,1.),(1.,1.),(1.,1.),(1.,1.),(1.,1.),(1.,1.),(1.,1.),(1.,
1.),(1.,1.),(1.,1.),(1.,1.),(1.,1.),(1.,1.),(1.,1.),(1.,1.),(1.,1.),(1.,
1.),(1.,1.),(1.,1.),(1.,1.),(1.,1.),(1.,1.),(1.,1.),(1.,1.),(1.,1.),(1.,
1.),(1.,1.)))
REPRESENTATION_ITEM('')
SURFACE()
);
#93=(
BOUNDED_SURFACE()
B_SPLINE_SURFACE(5,1,((#49250,#49251),(#49252,#49253),(#49254,#49255),(#49256,
#49257),(#49258,#49259),(#49260,#49261),(#49262,#49263),(#49264,#49265),
(#49266,#49267),(#49268,#49269),(#49270,#49271),(#49272,#49273),(#49274,
#49275),(#49276,#49277),(#49278,#49279),(#49280,#49281),(#49282,#49283),
(#49284,#49285),(#49286,#49287),(#49288,#49289),(#49290,#49291),(#49292,
#49293),(#49294,#49295),(#49296,#49297),(#49298,#49299),(#49300,#49301),
(#49302,#49303),(#49304,#49305),(#49306,#49307),(#49308,#49309),(#49310,
#49311),(#49312,#49313),(#49314,#49315),(#49316,#49317),(#49318,#49319),
(#49320,#49321),(#49322,#49323),(#49324,#49325),(#49326,#49327),(#49328,
#49329),(#49330,#49331),(#49332,#49333),(#49334,#49335),(#49336,#49337),
(#49338,#49339),(#49340,#49341),(#49342,#49343),(#49344,#49345),(#49346,
#49347),(#49348,#49349),(#49350,#49351),(#49352,#49353),(#49354,#49355),
(#49356,#49357),(#49358,#49359),(#49360,#49361),(#49362,#49363),(#49364,
#49365),(#49366,#49367),(#49368,#49369),(#49370,#49371),(#49372,#49373),
(#49374,#49375),(#49376,#49377),(#49378,#49379),(#49380,#49381),(#49382,
#49383),(#49384,#49385),(#49386,#49387),(#49388,#49389)),.UNSPECIFIED.,
 .F.,.F.,.F.)
B_SPLINE_SURFACE_WITH_KNOTS((6,1,1,1,1,1,1,1,1,1,1,1,1,1,1,1,1,1,1,1,1,
1,1,1,1,1,1,1,1,1,1,1,1,1,1,1,1,1,1,1,1,1,1,1,1,1,1,1,1,1,1,1,1,1,1,1,1,
1,1,1,1,1,1,1,1,6),(2,2),(-1.,-0.984615384615383,-0.969230769230768,-0.953846153846152,
-0.938461538461537,-0.923076923076922,-0.907692307692306,-0.892307692307691,
-0.876923076923076,-0.86153846153846,-0.846153846153845,-0.83076923076923,
-0.815384615384614,-0.799999999999999,-0.784615384615384,-0.769230769230768,
-0.753846153846153,-0.738461538461538,-0.723076923076922,-0.707692307692307,
-0.692307692307692,-0.676923076923076,-0.661538461538461,-0.646153846153846,
-0.63076923076923,-0.615384615384615,-0.6,-0.584615384615384,-0.569230769230769,
-0.553846153846154,-0.538461538461538,-0.523076923076923,-0.507692307692308,
-0.492307692307692,-0.476923076923077,-0.461538461538462,-0.446153846153846,
-0.430769230769231,-0.415384615384615,-0.4,-0.384615384615385,-0.369230769230769,
-0.353846153846154,-0.338461538461538,-0.323076923076923,-0.307692307692308,
-0.292307692307692,-0.276923076923077,-0.261538461538462,-0.246153846153846,
-0.230769230769231,-0.215384615384615,-0.2,-0.184615384615385,-0.169230769230769,
-0.153846153846154,-0.138461538461538,-0.123076923076923,-0.107692307692308,
-0.0923076923076923,-0.0769230769230769,-0.0615384615384615,-0.0461538461538462,
-0.0307692307692308,-0.0153846153846154,0.),(-1.,1.),.UNSPECIFIED.)
GEOMETRIC_REPRESENTATION_ITEM()
RATIONAL_B_SPLINE_SURFACE(((1.,1.),(1.,1.),(1.,1.),(1.,1.),(1.,1.),(1.,
1.),(1.,1.),(1.,1.),(1.,1.),(1.,1.),(1.,1.),(1.,1.),(1.,1.),(1.,1.),(1.,
1.),(1.,1.),(1.,1.),(1.,1.),(1.,1.),(1.,1.),(1.,1.),(1.,1.),(1.,1.),(1.,
1.),(1.,1.),(1.,1.),(1.,1.),(1.,1.),(1.,1.),(1.,1.),(1.,1.),(1.,1.),(1.,
1.),(1.,1.),(1.,1.),(1.,1.),(1.,1.),(1.,1.),(1.,1.),(1.,1.),(1.,1.),(1.,
1.),(1.,1.),(1.,1.),(1.,1.),(1.,1.),(1.,1.),(1.,1.),(1.,1.),(1.,1.),(1.,
1.),(1.,1.),(1.,1.),(1.,1.),(1.,1.),(1.,1.),(1.,1.),(1.,1.),(1.,1.),(1.,
1.),(1.,1.),(1.,1.),(1.,1.),(1.,1.),(1.,1.),(1.,1.),(1.,1.),(1.,1.),(1.,
1.),(1.,1.)))
REPRESENTATION_ITEM('')
SURFACE()
);
#94=(
BOUNDED_SURFACE()
B_SPLINE_SURFACE(5,1,((#49462,#49463),(#49464,#49465),(#49466,#49467),(#49468,
#49469),(#49470,#49471),(#49472,#49473),(#49474,#49475),(#49476,#49477),
(#49478,#49479),(#49480,#49481),(#49482,#49483),(#49484,#49485),(#49486,
#49487),(#49488,#49489),(#49490,#49491),(#49492,#49493),(#49494,#49495),
(#49496,#49497),(#49498,#49499),(#49500,#49501),(#49502,#49503),(#49504,
#49505),(#49506,#49507),(#49508,#49509),(#49510,#49511),(#49512,#49513),
(#49514,#49515),(#49516,#49517),(#49518,#49519),(#49520,#49521),(#49522,
#49523),(#49524,#49525),(#49526,#49527),(#49528,#49529),(#49530,#49531),
(#49532,#49533),(#49534,#49535),(#49536,#49537),(#49538,#49539),(#49540,
#49541),(#49542,#49543),(#49544,#49545),(#49546,#49547),(#49548,#49549),
(#49550,#49551),(#49552,#49553),(#49554,#49555),(#49556,#49557),(#49558,
#49559),(#49560,#49561),(#49562,#49563),(#49564,#49565),(#49566,#49567),
(#49568,#49569),(#49570,#49571),(#49572,#49573),(#49574,#49575),(#49576,
#49577),(#49578,#49579),(#49580,#49581),(#49582,#49583),(#49584,#49585),
(#49586,#49587),(#49588,#49589),(#49590,#49591),(#49592,#49593),(#49594,
#49595),(#49596,#49597),(#49598,#49599),(#49600,#49601)),.UNSPECIFIED.,
 .F.,.F.,.F.)
B_SPLINE_SURFACE_WITH_KNOTS((6,1,1,1,1,1,1,1,1,1,1,1,1,1,1,1,1,1,1,1,1,
1,1,1,1,1,1,1,1,1,1,1,1,1,1,1,1,1,1,1,1,1,1,1,1,1,1,1,1,1,1,1,1,1,1,1,1,
1,1,1,1,1,1,1,1,6),(2,2),(-1.,-0.984615384615383,-0.969230769230768,-0.953846153846152,
-0.938461538461537,-0.923076923076922,-0.907692307692306,-0.892307692307691,
-0.876923076923076,-0.86153846153846,-0.846153846153845,-0.83076923076923,
-0.815384615384614,-0.799999999999999,-0.784615384615384,-0.769230769230768,
-0.753846153846153,-0.738461538461538,-0.723076923076922,-0.707692307692307,
-0.692307692307692,-0.676923076923076,-0.661538461538461,-0.646153846153846,
-0.63076923076923,-0.615384615384615,-0.6,-0.584615384615384,-0.569230769230769,
-0.553846153846154,-0.538461538461538,-0.523076923076923,-0.507692307692308,
-0.492307692307692,-0.476923076923077,-0.461538461538462,-0.446153846153846,
-0.430769230769231,-0.415384615384615,-0.4,-0.384615384615385,-0.369230769230769,
-0.353846153846154,-0.338461538461538,-0.323076923076923,-0.307692307692308,
-0.292307692307692,-0.276923076923077,-0.261538461538462,-0.246153846153846,
-0.230769230769231,-0.215384615384615,-0.2,-0.184615384615385,-0.169230769230769,
-0.153846153846154,-0.138461538461538,-0.123076923076923,-0.107692307692308,
-0.0923076923076923,-0.0769230769230769,-0.0615384615384615,-0.0461538461538462,
-0.0307692307692308,-0.0153846153846154,0.),(-1.,1.),.UNSPECIFIED.)
GEOMETRIC_REPRESENTATION_ITEM()
RATIONAL_B_SPLINE_SURFACE(((1.,1.),(1.,1.),(1.,1.),(1.,1.),(1.,1.),(1.,
1.),(1.,1.),(1.,1.),(1.,1.),(1.,1.),(1.,1.),(1.,1.),(1.,1.),(1.,1.),(1.,
1.),(1.,1.),(1.,1.),(1.,1.),(1.,1.),(1.,1.),(1.,1.),(1.,1.),(1.,1.),(1.,
1.),(1.,1.),(1.,1.),(1.,1.),(1.,1.),(1.,1.),(1.,1.),(1.,1.),(1.,1.),(1.,
1.),(1.,1.),(1.,1.),(1.,1.),(1.,1.),(1.,1.),(1.,1.),(1.,1.),(1.,1.),(1.,
1.),(1.,1.),(1.,1.),(1.,1.),(1.,1.),(1.,1.),(1.,1.),(1.,1.),(1.,1.),(1.,
1.),(1.,1.),(1.,1.),(1.,1.),(1.,1.),(1.,1.),(1.,1.),(1.,1.),(1.,1.),(1.,
1.),(1.,1.),(1.,1.),(1.,1.),(1.,1.),(1.,1.),(1.,1.),(1.,1.),(1.,1.),(1.,
1.),(1.,1.)))
REPRESENTATION_ITEM('')
SURFACE()
);
#95=(
BOUNDED_SURFACE()
B_SPLINE_SURFACE(5,1,((#49692,#49693),(#49694,#49695),(#49696,#49697),(#49698,
#49699),(#49700,#49701),(#49702,#49703),(#49704,#49705),(#49706,#49707),
(#49708,#49709),(#49710,#49711),(#49712,#49713),(#49714,#49715),(#49716,
#49717),(#49718,#49719),(#49720,#49721),(#49722,#49723),(#49724,#49725),
(#49726,#49727),(#49728,#49729),(#49730,#49731),(#49732,#49733),(#49734,
#49735),(#49736,#49737),(#49738,#49739),(#49740,#49741),(#49742,#49743),
(#49744,#49745),(#49746,#49747),(#49748,#49749),(#49750,#49751),(#49752,
#49753),(#49754,#49755),(#49756,#49757),(#49758,#49759),(#49760,#49761),
(#49762,#49763),(#49764,#49765),(#49766,#49767),(#49768,#49769),(#49770,
#49771),(#49772,#49773),(#49774,#49775),(#49776,#49777),(#49778,#49779),
(#49780,#49781),(#49782,#49783),(#49784,#49785),(#49786,#49787),(#49788,
#49789),(#49790,#49791),(#49792,#49793),(#49794,#49795),(#49796,#49797),
(#49798,#49799),(#49800,#49801),(#49802,#49803),(#49804,#49805),(#49806,
#49807),(#49808,#49809),(#49810,#49811),(#49812,#49813),(#49814,#49815),
(#49816,#49817),(#49818,#49819),(#49820,#49821),(#49822,#49823),(#49824,
#49825),(#49826,#49827),(#49828,#49829),(#49830,#49831)),.UNSPECIFIED.,
 .F.,.F.,.F.)
B_SPLINE_SURFACE_WITH_KNOTS((6,1,1,1,1,1,1,1,1,1,1,1,1,1,1,1,1,1,1,1,1,
1,1,1,1,1,1,1,1,1,1,1,1,1,1,1,1,1,1,1,1,1,1,1,1,1,1,1,1,1,1,1,1,1,1,1,1,
1,1,1,1,1,1,1,1,6),(2,2),(-1.,-0.984615384615383,-0.969230769230768,-0.953846153846152,
-0.938461538461537,-0.923076923076922,-0.907692307692306,-0.892307692307691,
-0.876923076923076,-0.86153846153846,-0.846153846153845,-0.83076923076923,
-0.815384615384614,-0.799999999999999,-0.784615384615384,-0.769230769230768,
-0.753846153846153,-0.738461538461538,-0.723076923076922,-0.707692307692307,
-0.692307692307692,-0.676923076923076,-0.661538461538461,-0.646153846153846,
-0.63076923076923,-0.615384615384615,-0.6,-0.584615384615384,-0.569230769230769,
-0.553846153846154,-0.538461538461538,-0.523076923076923,-0.507692307692308,
-0.492307692307692,-0.476923076923077,-0.461538461538462,-0.446153846153846,
-0.430769230769231,-0.415384615384615,-0.4,-0.384615384615385,-0.369230769230769,
-0.353846153846154,-0.338461538461538,-0.323076923076923,-0.307692307692308,
-0.292307692307692,-0.276923076923077,-0.261538461538462,-0.246153846153846,
-0.230769230769231,-0.215384615384615,-0.2,-0.184615384615385,-0.169230769230769,
-0.153846153846154,-0.138461538461538,-0.123076923076923,-0.107692307692308,
-0.0923076923076923,-0.0769230769230769,-0.0615384615384615,-0.0461538461538462,
-0.0307692307692308,-0.0153846153846154,0.),(-1.,1.),.UNSPECIFIED.)
GEOMETRIC_REPRESENTATION_ITEM()
RATIONAL_B_SPLINE_SURFACE(((1.,1.),(1.,1.),(1.,1.),(1.,1.),(1.,1.),(1.,
1.),(1.,1.),(1.,1.),(1.,1.),(1.,1.),(1.,1.),(1.,1.),(1.,1.),(1.,1.),(1.,
1.),(1.,1.),(1.,1.),(1.,1.),(1.,1.),(1.,1.),(1.,1.),(1.,1.),(1.,1.),(1.,
1.),(1.,1.),(1.,1.),(1.,1.),(1.,1.),(1.,1.),(1.,1.),(1.,1.),(1.,1.),(1.,
1.),(1.,1.),(1.,1.),(1.,1.),(1.,1.),(1.,1.),(1.,1.),(1.,1.),(1.,1.),(1.,
1.),(1.,1.),(1.,1.),(1.,1.),(1.,1.),(1.,1.),(1.,1.),(1.,1.),(1.,1.),(1.,
1.),(1.,1.),(1.,1.),(1.,1.),(1.,1.),(1.,1.),(1.,1.),(1.,1.),(1.,1.),(1.,
1.),(1.,1.),(1.,1.),(1.,1.),(1.,1.),(1.,1.),(1.,1.),(1.,1.),(1.,1.),(1.,
1.),(1.,1.)))
REPRESENTATION_ITEM('')
SURFACE()
);
#96=(
BOUNDED_SURFACE()
B_SPLINE_SURFACE(5,1,((#49904,#49905),(#49906,#49907),(#49908,#49909),(#49910,
#49911),(#49912,#49913),(#49914,#49915),(#49916,#49917),(#49918,#49919),
(#49920,#49921),(#49922,#49923),(#49924,#49925),(#49926,#49927),(#49928,
#49929),(#49930,#49931),(#49932,#49933),(#49934,#49935),(#49936,#49937),
(#49938,#49939),(#49940,#49941),(#49942,#49943),(#49944,#49945),(#49946,
#49947),(#49948,#49949),(#49950,#49951),(#49952,#49953),(#49954,#49955),
(#49956,#49957),(#49958,#49959),(#49960,#49961),(#49962,#49963),(#49964,
#49965),(#49966,#49967),(#49968,#49969),(#49970,#49971),(#49972,#49973),
(#49974,#49975),(#49976,#49977),(#49978,#49979),(#49980,#49981),(#49982,
#49983),(#49984,#49985),(#49986,#49987),(#49988,#49989),(#49990,#49991),
(#49992,#49993),(#49994,#49995),(#49996,#49997),(#49998,#49999),(#50000,
#50001),(#50002,#50003),(#50004,#50005),(#50006,#50007),(#50008,#50009),
(#50010,#50011),(#50012,#50013),(#50014,#50015),(#50016,#50017),(#50018,
#50019),(#50020,#50021),(#50022,#50023),(#50024,#50025),(#50026,#50027),
(#50028,#50029),(#50030,#50031),(#50032,#50033),(#50034,#50035),(#50036,
#50037),(#50038,#50039),(#50040,#50041),(#50042,#50043)),.UNSPECIFIED.,
 .F.,.F.,.F.)
B_SPLINE_SURFACE_WITH_KNOTS((6,1,1,1,1,1,1,1,1,1,1,1,1,1,1,1,1,1,1,1,1,
1,1,1,1,1,1,1,1,1,1,1,1,1,1,1,1,1,1,1,1,1,1,1,1,1,1,1,1,1,1,1,1,1,1,1,1,
1,1,1,1,1,1,1,1,6),(2,2),(-1.,-0.984615384615383,-0.969230769230768,-0.953846153846152,
-0.938461538461537,-0.923076923076922,-0.907692307692306,-0.892307692307691,
-0.876923076923076,-0.86153846153846,-0.846153846153845,-0.83076923076923,
-0.815384615384614,-0.799999999999999,-0.784615384615384,-0.769230769230768,
-0.753846153846153,-0.738461538461538,-0.723076923076922,-0.707692307692307,
-0.692307692307692,-0.676923076923076,-0.661538461538461,-0.646153846153846,
-0.63076923076923,-0.615384615384615,-0.6,-0.584615384615384,-0.569230769230769,
-0.553846153846154,-0.538461538461538,-0.523076923076923,-0.507692307692308,
-0.492307692307692,-0.476923076923077,-0.461538461538462,-0.446153846153846,
-0.430769230769231,-0.415384615384615,-0.4,-0.384615384615385,-0.369230769230769,
-0.353846153846154,-0.338461538461538,-0.323076923076923,-0.307692307692308,
-0.292307692307692,-0.276923076923077,-0.261538461538462,-0.246153846153846,
-0.230769230769231,-0.215384615384615,-0.2,-0.184615384615385,-0.169230769230769,
-0.153846153846154,-0.138461538461538,-0.123076923076923,-0.107692307692308,
-0.0923076923076923,-0.0769230769230769,-0.0615384615384615,-0.0461538461538462,
-0.0307692307692308,-0.0153846153846154,0.),(-1.,1.),.UNSPECIFIED.)
GEOMETRIC_REPRESENTATION_ITEM()
RATIONAL_B_SPLINE_SURFACE(((1.,1.),(1.,1.),(1.,1.),(1.,1.),(1.,1.),(1.,
1.),(1.,1.),(1.,1.),(1.,1.),(1.,1.),(1.,1.),(1.,1.),(1.,1.),(1.,1.),(1.,
1.),(1.,1.),(1.,1.),(1.,1.),(1.,1.),(1.,1.),(1.,1.),(1.,1.),(1.,1.),(1.,
1.),(1.,1.),(1.,1.),(1.,1.),(1.,1.),(1.,1.),(1.,1.),(1.,1.),(1.,1.),(1.,
1.),(1.,1.),(1.,1.),(1.,1.),(1.,1.),(1.,1.),(1.,1.),(1.,1.),(1.,1.),(1.,
1.),(1.,1.),(1.,1.),(1.,1.),(1.,1.),(1.,1.),(1.,1.),(1.,1.),(1.,1.),(1.,
1.),(1.,1.),(1.,1.),(1.,1.),(1.,1.),(1.,1.),(1.,1.),(1.,1.),(1.,1.),(1.,
1.),(1.,1.),(1.,1.),(1.,1.),(1.,1.),(1.,1.),(1.,1.),(1.,1.),(1.,1.),(1.,
1.),(1.,1.)))
REPRESENTATION_ITEM('')
SURFACE()
);
#97=(
BOUNDED_SURFACE()
B_SPLINE_SURFACE(5,1,((#50134,#50135),(#50136,#50137),(#50138,#50139),(#50140,
#50141),(#50142,#50143),(#50144,#50145),(#50146,#50147),(#50148,#50149),
(#50150,#50151),(#50152,#50153),(#50154,#50155),(#50156,#50157),(#50158,
#50159),(#50160,#50161),(#50162,#50163),(#50164,#50165),(#50166,#50167),
(#50168,#50169),(#50170,#50171),(#50172,#50173),(#50174,#50175),(#50176,
#50177),(#50178,#50179),(#50180,#50181),(#50182,#50183),(#50184,#50185),
(#50186,#50187),(#50188,#50189),(#50190,#50191),(#50192,#50193),(#50194,
#50195),(#50196,#50197),(#50198,#50199),(#50200,#50201),(#50202,#50203),
(#50204,#50205),(#50206,#50207),(#50208,#50209),(#50210,#50211),(#50212,
#50213),(#50214,#50215),(#50216,#50217),(#50218,#50219),(#50220,#50221),
(#50222,#50223),(#50224,#50225),(#50226,#50227),(#50228,#50229),(#50230,
#50231),(#50232,#50233),(#50234,#50235),(#50236,#50237),(#50238,#50239),
(#50240,#50241),(#50242,#50243),(#50244,#50245),(#50246,#50247),(#50248,
#50249),(#50250,#50251),(#50252,#50253),(#50254,#50255),(#50256,#50257),
(#50258,#50259),(#50260,#50261),(#50262,#50263),(#50264,#50265),(#50266,
#50267),(#50268,#50269),(#50270,#50271),(#50272,#50273)),.UNSPECIFIED.,
 .F.,.F.,.F.)
B_SPLINE_SURFACE_WITH_KNOTS((6,1,1,1,1,1,1,1,1,1,1,1,1,1,1,1,1,1,1,1,1,
1,1,1,1,1,1,1,1,1,1,1,1,1,1,1,1,1,1,1,1,1,1,1,1,1,1,1,1,1,1,1,1,1,1,1,1,
1,1,1,1,1,1,1,1,6),(2,2),(-1.,-0.984615384615383,-0.969230769230768,-0.953846153846152,
-0.938461538461537,-0.923076923076922,-0.907692307692306,-0.892307692307691,
-0.876923076923076,-0.86153846153846,-0.846153846153845,-0.83076923076923,
-0.815384615384614,-0.799999999999999,-0.784615384615384,-0.769230769230768,
-0.753846153846153,-0.738461538461538,-0.723076923076922,-0.707692307692307,
-0.692307692307692,-0.676923076923076,-0.661538461538461,-0.646153846153846,
-0.63076923076923,-0.615384615384615,-0.6,-0.584615384615384,-0.569230769230769,
-0.553846153846154,-0.538461538461538,-0.523076923076923,-0.507692307692308,
-0.492307692307692,-0.476923076923077,-0.461538461538462,-0.446153846153846,
-0.430769230769231,-0.415384615384615,-0.4,-0.384615384615385,-0.369230769230769,
-0.353846153846154,-0.338461538461538,-0.323076923076923,-0.307692307692308,
-0.292307692307692,-0.276923076923077,-0.261538461538462,-0.246153846153846,
-0.230769230769231,-0.215384615384615,-0.2,-0.184615384615385,-0.169230769230769,
-0.153846153846154,-0.138461538461538,-0.123076923076923,-0.107692307692308,
-0.0923076923076923,-0.0769230769230769,-0.0615384615384615,-0.0461538461538462,
-0.0307692307692308,-0.0153846153846154,0.),(-1.,1.),.UNSPECIFIED.)
GEOMETRIC_REPRESENTATION_ITEM()
RATIONAL_B_SPLINE_SURFACE(((1.,1.),(1.,1.),(1.,1.),(1.,1.),(1.,1.),(1.,
1.),(1.,1.),(1.,1.),(1.,1.),(1.,1.),(1.,1.),(1.,1.),(1.,1.),(1.,1.),(1.,
1.),(1.,1.),(1.,1.),(1.,1.),(1.,1.),(1.,1.),(1.,1.),(1.,1.),(1.,1.),(1.,
1.),(1.,1.),(1.,1.),(1.,1.),(1.,1.),(1.,1.),(1.,1.),(1.,1.),(1.,1.),(1.,
1.),(1.,1.),(1.,1.),(1.,1.),(1.,1.),(1.,1.),(1.,1.),(1.,1.),(1.,1.),(1.,
1.),(1.,1.),(1.,1.),(1.,1.),(1.,1.),(1.,1.),(1.,1.),(1.,1.),(1.,1.),(1.,
1.),(1.,1.),(1.,1.),(1.,1.),(1.,1.),(1.,1.),(1.,1.),(1.,1.),(1.,1.),(1.,
1.),(1.,1.),(1.,1.),(1.,1.),(1.,1.),(1.,1.),(1.,1.),(1.,1.),(1.,1.),(1.,
1.),(1.,1.)))
REPRESENTATION_ITEM('')
SURFACE()
);
#98=(
BOUNDED_SURFACE()
B_SPLINE_SURFACE(5,1,((#50346,#50347),(#50348,#50349),(#50350,#50351),(#50352,
#50353),(#50354,#50355),(#50356,#50357),(#50358,#50359),(#50360,#50361),
(#50362,#50363),(#50364,#50365),(#50366,#50367),(#50368,#50369),(#50370,
#50371),(#50372,#50373),(#50374,#50375),(#50376,#50377),(#50378,#50379),
(#50380,#50381),(#50382,#50383),(#50384,#50385),(#50386,#50387),(#50388,
#50389),(#50390,#50391),(#50392,#50393),(#50394,#50395),(#50396,#50397),
(#50398,#50399),(#50400,#50401),(#50402,#50403),(#50404,#50405),(#50406,
#50407),(#50408,#50409),(#50410,#50411),(#50412,#50413),(#50414,#50415),
(#50416,#50417),(#50418,#50419),(#50420,#50421),(#50422,#50423),(#50424,
#50425),(#50426,#50427),(#50428,#50429),(#50430,#50431),(#50432,#50433),
(#50434,#50435),(#50436,#50437),(#50438,#50439),(#50440,#50441),(#50442,
#50443),(#50444,#50445),(#50446,#50447),(#50448,#50449),(#50450,#50451),
(#50452,#50453),(#50454,#50455),(#50456,#50457),(#50458,#50459),(#50460,
#50461),(#50462,#50463),(#50464,#50465),(#50466,#50467),(#50468,#50469),
(#50470,#50471),(#50472,#50473),(#50474,#50475),(#50476,#50477),(#50478,
#50479),(#50480,#50481),(#50482,#50483),(#50484,#50485)),.UNSPECIFIED.,
 .F.,.F.,.F.)
B_SPLINE_SURFACE_WITH_KNOTS((6,1,1,1,1,1,1,1,1,1,1,1,1,1,1,1,1,1,1,1,1,
1,1,1,1,1,1,1,1,1,1,1,1,1,1,1,1,1,1,1,1,1,1,1,1,1,1,1,1,1,1,1,1,1,1,1,1,
1,1,1,1,1,1,1,1,6),(2,2),(-1.,-0.984615384615383,-0.969230769230768,-0.953846153846152,
-0.938461538461537,-0.923076923076922,-0.907692307692306,-0.892307692307691,
-0.876923076923076,-0.86153846153846,-0.846153846153845,-0.83076923076923,
-0.815384615384614,-0.799999999999999,-0.784615384615384,-0.769230769230768,
-0.753846153846153,-0.738461538461538,-0.723076923076922,-0.707692307692307,
-0.692307692307692,-0.676923076923076,-0.661538461538461,-0.646153846153846,
-0.63076923076923,-0.615384615384615,-0.6,-0.584615384615384,-0.569230769230769,
-0.553846153846154,-0.538461538461538,-0.523076923076923,-0.507692307692308,
-0.492307692307692,-0.476923076923077,-0.461538461538462,-0.446153846153846,
-0.430769230769231,-0.415384615384615,-0.4,-0.384615384615385,-0.369230769230769,
-0.353846153846154,-0.338461538461538,-0.323076923076923,-0.307692307692308,
-0.292307692307692,-0.276923076923077,-0.261538461538462,-0.246153846153846,
-0.230769230769231,-0.215384615384615,-0.2,-0.184615384615385,-0.169230769230769,
-0.153846153846154,-0.138461538461538,-0.123076923076923,-0.107692307692308,
-0.0923076923076923,-0.0769230769230769,-0.0615384615384615,-0.0461538461538462,
-0.0307692307692308,-0.0153846153846154,0.),(-1.,1.),.UNSPECIFIED.)
GEOMETRIC_REPRESENTATION_ITEM()
RATIONAL_B_SPLINE_SURFACE(((1.,1.),(1.,1.),(1.,1.),(1.,1.),(1.,1.),(1.,
1.),(1.,1.),(1.,1.),(1.,1.),(1.,1.),(1.,1.),(1.,1.),(1.,1.),(1.,1.),(1.,
1.),(1.,1.),(1.,1.),(1.,1.),(1.,1.),(1.,1.),(1.,1.),(1.,1.),(1.,1.),(1.,
1.),(1.,1.),(1.,1.),(1.,1.),(1.,1.),(1.,1.),(1.,1.),(1.,1.),(1.,1.),(1.,
1.),(1.,1.),(1.,1.),(1.,1.),(1.,1.),(1.,1.),(1.,1.),(1.,1.),(1.,1.),(1.,
1.),(1.,1.),(1.,1.),(1.,1.),(1.,1.),(1.,1.),(1.,1.),(1.,1.),(1.,1.),(1.,
1.),(1.,1.),(1.,1.),(1.,1.),(1.,1.),(1.,1.),(1.,1.),(1.,1.),(1.,1.),(1.,
1.),(1.,1.),(1.,1.),(1.,1.),(1.,1.),(1.,1.),(1.,1.),(1.,1.),(1.,1.),(1.,
1.),(1.,1.)))
REPRESENTATION_ITEM('')
SURFACE()
);
#99=(
BOUNDED_SURFACE()
B_SPLINE_SURFACE(5,1,((#50576,#50577),(#50578,#50579),(#50580,#50581),(#50582,
#50583),(#50584,#50585),(#50586,#50587),(#50588,#50589),(#50590,#50591),
(#50592,#50593),(#50594,#50595),(#50596,#50597),(#50598,#50599),(#50600,
#50601),(#50602,#50603),(#50604,#50605),(#50606,#50607),(#50608,#50609),
(#50610,#50611),(#50612,#50613),(#50614,#50615),(#50616,#50617),(#50618,
#50619),(#50620,#50621),(#50622,#50623),(#50624,#50625),(#50626,#50627),
(#50628,#50629),(#50630,#50631),(#50632,#50633),(#50634,#50635),(#50636,
#50637),(#50638,#50639),(#50640,#50641),(#50642,#50643),(#50644,#50645),
(#50646,#50647),(#50648,#50649),(#50650,#50651),(#50652,#50653),(#50654,
#50655),(#50656,#50657),(#50658,#50659),(#50660,#50661),(#50662,#50663),
(#50664,#50665),(#50666,#50667),(#50668,#50669),(#50670,#50671),(#50672,
#50673),(#50674,#50675),(#50676,#50677),(#50678,#50679),(#50680,#50681),
(#50682,#50683),(#50684,#50685),(#50686,#50687),(#50688,#50689),(#50690,
#50691),(#50692,#50693),(#50694,#50695),(#50696,#50697),(#50698,#50699),
(#50700,#50701),(#50702,#50703),(#50704,#50705),(#50706,#50707),(#50708,
#50709),(#50710,#50711),(#50712,#50713),(#50714,#50715)),.UNSPECIFIED.,
 .F.,.F.,.F.)
B_SPLINE_SURFACE_WITH_KNOTS((6,1,1,1,1,1,1,1,1,1,1,1,1,1,1,1,1,1,1,1,1,
1,1,1,1,1,1,1,1,1,1,1,1,1,1,1,1,1,1,1,1,1,1,1,1,1,1,1,1,1,1,1,1,1,1,1,1,
1,1,1,1,1,1,1,1,6),(2,2),(-1.,-0.984615384615383,-0.969230769230768,-0.953846153846152,
-0.938461538461537,-0.923076923076922,-0.907692307692306,-0.892307692307691,
-0.876923076923076,-0.86153846153846,-0.846153846153845,-0.83076923076923,
-0.815384615384614,-0.799999999999999,-0.784615384615384,-0.769230769230768,
-0.753846153846153,-0.738461538461538,-0.723076923076922,-0.707692307692307,
-0.692307692307692,-0.676923076923076,-0.661538461538461,-0.646153846153846,
-0.63076923076923,-0.615384615384615,-0.6,-0.584615384615384,-0.569230769230769,
-0.553846153846154,-0.538461538461538,-0.523076923076923,-0.507692307692308,
-0.492307692307692,-0.476923076923077,-0.461538461538462,-0.446153846153846,
-0.430769230769231,-0.415384615384615,-0.4,-0.384615384615385,-0.369230769230769,
-0.353846153846154,-0.338461538461538,-0.323076923076923,-0.307692307692308,
-0.292307692307692,-0.276923076923077,-0.261538461538462,-0.246153846153846,
-0.230769230769231,-0.215384615384615,-0.2,-0.184615384615385,-0.169230769230769,
-0.153846153846154,-0.138461538461538,-0.123076923076923,-0.107692307692308,
-0.0923076923076923,-0.0769230769230769,-0.0615384615384615,-0.0461538461538462,
-0.0307692307692308,-0.0153846153846154,0.),(-1.,1.),.UNSPECIFIED.)
GEOMETRIC_REPRESENTATION_ITEM()
RATIONAL_B_SPLINE_SURFACE(((1.,1.),(1.,1.),(1.,1.),(1.,1.),(1.,1.),(1.,
1.),(1.,1.),(1.,1.),(1.,1.),(1.,1.),(1.,1.),(1.,1.),(1.,1.),(1.,1.),(1.,
1.),(1.,1.),(1.,1.),(1.,1.),(1.,1.),(1.,1.),(1.,1.),(1.,1.),(1.,1.),(1.,
1.),(1.,1.),(1.,1.),(1.,1.),(1.,1.),(1.,1.),(1.,1.),(1.,1.),(1.,1.),(1.,
1.),(1.,1.),(1.,1.),(1.,1.),(1.,1.),(1.,1.),(1.,1.),(1.,1.),(1.,1.),(1.,
1.),(1.,1.),(1.,1.),(1.,1.),(1.,1.),(1.,1.),(1.,1.),(1.,1.),(1.,1.),(1.,
1.),(1.,1.),(1.,1.),(1.,1.),(1.,1.),(1.,1.),(1.,1.),(1.,1.),(1.,1.),(1.,
1.),(1.,1.),(1.,1.),(1.,1.),(1.,1.),(1.,1.),(1.,1.),(1.,1.),(1.,1.),(1.,
1.),(1.,1.)))
REPRESENTATION_ITEM('')
SURFACE()
);
#100=(
BOUNDED_SURFACE()
B_SPLINE_SURFACE(5,1,((#50788,#50789),(#50790,#50791),(#50792,#50793),(#50794,
#50795),(#50796,#50797),(#50798,#50799),(#50800,#50801),(#50802,#50803),
(#50804,#50805),(#50806,#50807),(#50808,#50809),(#50810,#50811),(#50812,
#50813),(#50814,#50815),(#50816,#50817),(#50818,#50819),(#50820,#50821),
(#50822,#50823),(#50824,#50825),(#50826,#50827),(#50828,#50829),(#50830,
#50831),(#50832,#50833),(#50834,#50835),(#50836,#50837),(#50838,#50839),
(#50840,#50841),(#50842,#50843),(#50844,#50845),(#50846,#50847),(#50848,
#50849),(#50850,#50851),(#50852,#50853),(#50854,#50855),(#50856,#50857),
(#50858,#50859),(#50860,#50861),(#50862,#50863),(#50864,#50865),(#50866,
#50867),(#50868,#50869),(#50870,#50871),(#50872,#50873),(#50874,#50875),
(#50876,#50877),(#50878,#50879),(#50880,#50881),(#50882,#50883),(#50884,
#50885),(#50886,#50887),(#50888,#50889),(#50890,#50891),(#50892,#50893),
(#50894,#50895),(#50896,#50897),(#50898,#50899),(#50900,#50901),(#50902,
#50903),(#50904,#50905),(#50906,#50907),(#50908,#50909),(#50910,#50911),
(#50912,#50913),(#50914,#50915),(#50916,#50917),(#50918,#50919),(#50920,
#50921),(#50922,#50923),(#50924,#50925),(#50926,#50927)),.UNSPECIFIED.,
 .F.,.F.,.F.)
B_SPLINE_SURFACE_WITH_KNOTS((6,1,1,1,1,1,1,1,1,1,1,1,1,1,1,1,1,1,1,1,1,
1,1,1,1,1,1,1,1,1,1,1,1,1,1,1,1,1,1,1,1,1,1,1,1,1,1,1,1,1,1,1,1,1,1,1,1,
1,1,1,1,1,1,1,1,6),(2,2),(-1.,-0.984615384615383,-0.969230769230768,-0.953846153846152,
-0.938461538461537,-0.923076923076922,-0.907692307692306,-0.892307692307691,
-0.876923076923076,-0.86153846153846,-0.846153846153845,-0.83076923076923,
-0.815384615384614,-0.799999999999999,-0.784615384615384,-0.769230769230768,
-0.753846153846153,-0.738461538461538,-0.723076923076922,-0.707692307692307,
-0.692307692307692,-0.676923076923076,-0.661538461538461,-0.646153846153846,
-0.63076923076923,-0.615384615384615,-0.6,-0.584615384615384,-0.569230769230769,
-0.553846153846154,-0.538461538461538,-0.523076923076923,-0.507692307692308,
-0.492307692307692,-0.476923076923077,-0.461538461538462,-0.446153846153846,
-0.430769230769231,-0.415384615384615,-0.4,-0.384615384615385,-0.369230769230769,
-0.353846153846154,-0.338461538461538,-0.323076923076923,-0.307692307692308,
-0.292307692307692,-0.276923076923077,-0.261538461538462,-0.246153846153846,
-0.230769230769231,-0.215384615384615,-0.2,-0.184615384615385,-0.169230769230769,
-0.153846153846154,-0.138461538461538,-0.123076923076923,-0.107692307692308,
-0.0923076923076923,-0.0769230769230769,-0.0615384615384615,-0.0461538461538462,
-0.0307692307692308,-0.0153846153846154,0.),(-1.,1.),.UNSPECIFIED.)
GEOMETRIC_REPRESENTATION_ITEM()
RATIONAL_B_SPLINE_SURFACE(((1.,1.),(1.,1.),(1.,1.),(1.,1.),(1.,1.),(1.,
1.),(1.,1.),(1.,1.),(1.,1.),(1.,1.),(1.,1.),(1.,1.),(1.,1.),(1.,1.),(1.,
1.),(1.,1.),(1.,1.),(1.,1.),(1.,1.),(1.,1.),(1.,1.),(1.,1.),(1.,1.),(1.,
1.),(1.,1.),(1.,1.),(1.,1.),(1.,1.),(1.,1.),(1.,1.),(1.,1.),(1.,1.),(1.,
1.),(1.,1.),(1.,1.),(1.,1.),(1.,1.),(1.,1.),(1.,1.),(1.,1.),(1.,1.),(1.,
1.),(1.,1.),(1.,1.),(1.,1.),(1.,1.),(1.,1.),(1.,1.),(1.,1.),(1.,1.),(1.,
1.),(1.,1.),(1.,1.),(1.,1.),(1.,1.),(1.,1.),(1.,1.),(1.,1.),(1.,1.),(1.,
1.),(1.,1.),(1.,1.),(1.,1.),(1.,1.),(1.,1.),(1.,1.),(1.,1.),(1.,1.),(1.,
1.),(1.,1.)))
REPRESENTATION_ITEM('')
SURFACE()
);
#101=(
BOUNDED_SURFACE()
B_SPLINE_SURFACE(5,1,((#51018,#51019),(#51020,#51021),(#51022,#51023),(#51024,
#51025),(#51026,#51027),(#51028,#51029),(#51030,#51031),(#51032,#51033),
(#51034,#51035),(#51036,#51037),(#51038,#51039),(#51040,#51041),(#51042,
#51043),(#51044,#51045),(#51046,#51047),(#51048,#51049),(#51050,#51051),
(#51052,#51053),(#51054,#51055),(#51056,#51057),(#51058,#51059),(#51060,
#51061),(#51062,#51063),(#51064,#51065),(#51066,#51067),(#51068,#51069),
(#51070,#51071),(#51072,#51073),(#51074,#51075),(#51076,#51077),(#51078,
#51079),(#51080,#51081),(#51082,#51083),(#51084,#51085),(#51086,#51087),
(#51088,#51089),(#51090,#51091),(#51092,#51093),(#51094,#51095),(#51096,
#51097),(#51098,#51099),(#51100,#51101),(#51102,#51103),(#51104,#51105),
(#51106,#51107),(#51108,#51109),(#51110,#51111),(#51112,#51113),(#51114,
#51115),(#51116,#51117),(#51118,#51119),(#51120,#51121),(#51122,#51123),
(#51124,#51125),(#51126,#51127),(#51128,#51129),(#51130,#51131),(#51132,
#51133),(#51134,#51135),(#51136,#51137),(#51138,#51139),(#51140,#51141),
(#51142,#51143),(#51144,#51145),(#51146,#51147),(#51148,#51149),(#51150,
#51151),(#51152,#51153),(#51154,#51155),(#51156,#51157)),.UNSPECIFIED.,
 .F.,.F.,.F.)
B_SPLINE_SURFACE_WITH_KNOTS((6,1,1,1,1,1,1,1,1,1,1,1,1,1,1,1,1,1,1,1,1,
1,1,1,1,1,1,1,1,1,1,1,1,1,1,1,1,1,1,1,1,1,1,1,1,1,1,1,1,1,1,1,1,1,1,1,1,
1,1,1,1,1,1,1,1,6),(2,2),(-1.,-0.984615384615383,-0.969230769230768,-0.953846153846152,
-0.938461538461537,-0.923076923076922,-0.907692307692306,-0.892307692307691,
-0.876923076923076,-0.86153846153846,-0.846153846153845,-0.83076923076923,
-0.815384615384614,-0.799999999999999,-0.784615384615384,-0.769230769230768,
-0.753846153846153,-0.738461538461538,-0.723076923076922,-0.707692307692307,
-0.692307692307692,-0.676923076923076,-0.661538461538461,-0.646153846153846,
-0.63076923076923,-0.615384615384615,-0.6,-0.584615384615384,-0.569230769230769,
-0.553846153846154,-0.538461538461538,-0.523076923076923,-0.507692307692308,
-0.492307692307692,-0.476923076923077,-0.461538461538462,-0.446153846153846,
-0.430769230769231,-0.415384615384615,-0.4,-0.384615384615385,-0.369230769230769,
-0.353846153846154,-0.338461538461538,-0.323076923076923,-0.307692307692308,
-0.292307692307692,-0.276923076923077,-0.261538461538462,-0.246153846153846,
-0.230769230769231,-0.215384615384615,-0.2,-0.184615384615385,-0.169230769230769,
-0.153846153846154,-0.138461538461538,-0.123076923076923,-0.107692307692308,
-0.0923076923076923,-0.0769230769230769,-0.0615384615384615,-0.0461538461538462,
-0.0307692307692308,-0.0153846153846154,0.),(-1.,1.),.UNSPECIFIED.)
GEOMETRIC_REPRESENTATION_ITEM()
RATIONAL_B_SPLINE_SURFACE(((1.,1.),(1.,1.),(1.,1.),(1.,1.),(1.,1.),(1.,
1.),(1.,1.),(1.,1.),(1.,1.),(1.,1.),(1.,1.),(1.,1.),(1.,1.),(1.,1.),(1.,
1.),(1.,1.),(1.,1.),(1.,1.),(1.,1.),(1.,1.),(1.,1.),(1.,1.),(1.,1.),(1.,
1.),(1.,1.),(1.,1.),(1.,1.),(1.,1.),(1.,1.),(1.,1.),(1.,1.),(1.,1.),(1.,
1.),(1.,1.),(1.,1.),(1.,1.),(1.,1.),(1.,1.),(1.,1.),(1.,1.),(1.,1.),(1.,
1.),(1.,1.),(1.,1.),(1.,1.),(1.,1.),(1.,1.),(1.,1.),(1.,1.),(1.,1.),(1.,
1.),(1.,1.),(1.,1.),(1.,1.),(1.,1.),(1.,1.),(1.,1.),(1.,1.),(1.,1.),(1.,
1.),(1.,1.),(1.,1.),(1.,1.),(1.,1.),(1.,1.),(1.,1.),(1.,1.),(1.,1.),(1.,
1.),(1.,1.)))
REPRESENTATION_ITEM('')
SURFACE()
);
#102=(
BOUNDED_SURFACE()
B_SPLINE_SURFACE(5,1,((#51230,#51231),(#51232,#51233),(#51234,#51235),(#51236,
#51237),(#51238,#51239),(#51240,#51241),(#51242,#51243),(#51244,#51245),
(#51246,#51247),(#51248,#51249),(#51250,#51251),(#51252,#51253),(#51254,
#51255),(#51256,#51257),(#51258,#51259),(#51260,#51261),(#51262,#51263),
(#51264,#51265),(#51266,#51267),(#51268,#51269),(#51270,#51271),(#51272,
#51273),(#51274,#51275),(#51276,#51277),(#51278,#51279),(#51280,#51281),
(#51282,#51283),(#51284,#51285),(#51286,#51287),(#51288,#51289),(#51290,
#51291),(#51292,#51293),(#51294,#51295),(#51296,#51297),(#51298,#51299),
(#51300,#51301),(#51302,#51303),(#51304,#51305),(#51306,#51307),(#51308,
#51309),(#51310,#51311),(#51312,#51313),(#51314,#51315),(#51316,#51317),
(#51318,#51319),(#51320,#51321),(#51322,#51323),(#51324,#51325),(#51326,
#51327),(#51328,#51329),(#51330,#51331),(#51332,#51333),(#51334,#51335),
(#51336,#51337),(#51338,#51339),(#51340,#51341),(#51342,#51343),(#51344,
#51345),(#51346,#51347),(#51348,#51349),(#51350,#51351),(#51352,#51353),
(#51354,#51355),(#51356,#51357),(#51358,#51359),(#51360,#51361),(#51362,
#51363),(#51364,#51365),(#51366,#51367),(#51368,#51369)),.UNSPECIFIED.,
 .F.,.F.,.F.)
B_SPLINE_SURFACE_WITH_KNOTS((6,1,1,1,1,1,1,1,1,1,1,1,1,1,1,1,1,1,1,1,1,
1,1,1,1,1,1,1,1,1,1,1,1,1,1,1,1,1,1,1,1,1,1,1,1,1,1,1,1,1,1,1,1,1,1,1,1,
1,1,1,1,1,1,1,1,6),(2,2),(-1.,-0.984615384615383,-0.969230769230768,-0.953846153846152,
-0.938461538461537,-0.923076923076922,-0.907692307692306,-0.892307692307691,
-0.876923076923076,-0.86153846153846,-0.846153846153845,-0.83076923076923,
-0.815384615384614,-0.799999999999999,-0.784615384615384,-0.769230769230768,
-0.753846153846153,-0.738461538461538,-0.723076923076922,-0.707692307692307,
-0.692307692307692,-0.676923076923076,-0.661538461538461,-0.646153846153846,
-0.63076923076923,-0.615384615384615,-0.6,-0.584615384615384,-0.569230769230769,
-0.553846153846154,-0.538461538461538,-0.523076923076923,-0.507692307692308,
-0.492307692307692,-0.476923076923077,-0.461538461538462,-0.446153846153846,
-0.430769230769231,-0.415384615384615,-0.4,-0.384615384615385,-0.369230769230769,
-0.353846153846154,-0.338461538461538,-0.323076923076923,-0.307692307692308,
-0.292307692307692,-0.276923076923077,-0.261538461538462,-0.246153846153846,
-0.230769230769231,-0.215384615384615,-0.2,-0.184615384615385,-0.169230769230769,
-0.153846153846154,-0.138461538461538,-0.123076923076923,-0.107692307692308,
-0.0923076923076923,-0.0769230769230769,-0.0615384615384615,-0.0461538461538462,
-0.0307692307692308,-0.0153846153846154,0.),(-1.,1.),.UNSPECIFIED.)
GEOMETRIC_REPRESENTATION_ITEM()
RATIONAL_B_SPLINE_SURFACE(((1.,1.),(1.,1.),(1.,1.),(1.,1.),(1.,1.),(1.,
1.),(1.,1.),(1.,1.),(1.,1.),(1.,1.),(1.,1.),(1.,1.),(1.,1.),(1.,1.),(1.,
1.),(1.,1.),(1.,1.),(1.,1.),(1.,1.),(1.,1.),(1.,1.),(1.,1.),(1.,1.),(1.,
1.),(1.,1.),(1.,1.),(1.,1.),(1.,1.),(1.,1.),(1.,1.),(1.,1.),(1.,1.),(1.,
1.),(1.,1.),(1.,1.),(1.,1.),(1.,1.),(1.,1.),(1.,1.),(1.,1.),(1.,1.),(1.,
1.),(1.,1.),(1.,1.),(1.,1.),(1.,1.),(1.,1.),(1.,1.),(1.,1.),(1.,1.),(1.,
1.),(1.,1.),(1.,1.),(1.,1.),(1.,1.),(1.,1.),(1.,1.),(1.,1.),(1.,1.),(1.,
1.),(1.,1.),(1.,1.),(1.,1.),(1.,1.),(1.,1.),(1.,1.),(1.,1.),(1.,1.),(1.,
1.),(1.,1.)))
REPRESENTATION_ITEM('')
SURFACE()
);
#103=(
BOUNDED_SURFACE()
B_SPLINE_SURFACE(5,1,((#51460,#51461),(#51462,#51463),(#51464,#51465),(#51466,
#51467),(#51468,#51469),(#51470,#51471),(#51472,#51473),(#51474,#51475),
(#51476,#51477),(#51478,#51479),(#51480,#51481),(#51482,#51483),(#51484,
#51485),(#51486,#51487),(#51488,#51489),(#51490,#51491),(#51492,#51493),
(#51494,#51495),(#51496,#51497),(#51498,#51499),(#51500,#51501),(#51502,
#51503),(#51504,#51505),(#51506,#51507),(#51508,#51509),(#51510,#51511),
(#51512,#51513),(#51514,#51515),(#51516,#51517),(#51518,#51519),(#51520,
#51521),(#51522,#51523),(#51524,#51525),(#51526,#51527),(#51528,#51529),
(#51530,#51531),(#51532,#51533),(#51534,#51535),(#51536,#51537),(#51538,
#51539),(#51540,#51541),(#51542,#51543),(#51544,#51545),(#51546,#51547),
(#51548,#51549),(#51550,#51551),(#51552,#51553),(#51554,#51555),(#51556,
#51557),(#51558,#51559),(#51560,#51561),(#51562,#51563),(#51564,#51565),
(#51566,#51567),(#51568,#51569),(#51570,#51571),(#51572,#51573),(#51574,
#51575),(#51576,#51577),(#51578,#51579),(#51580,#51581),(#51582,#51583),
(#51584,#51585),(#51586,#51587),(#51588,#51589),(#51590,#51591),(#51592,
#51593),(#51594,#51595),(#51596,#51597),(#51598,#51599)),.UNSPECIFIED.,
 .F.,.F.,.F.)
B_SPLINE_SURFACE_WITH_KNOTS((6,1,1,1,1,1,1,1,1,1,1,1,1,1,1,1,1,1,1,1,1,
1,1,1,1,1,1,1,1,1,1,1,1,1,1,1,1,1,1,1,1,1,1,1,1,1,1,1,1,1,1,1,1,1,1,1,1,
1,1,1,1,1,1,1,1,6),(2,2),(-1.,-0.984615384615383,-0.969230769230768,-0.953846153846152,
-0.938461538461537,-0.923076923076922,-0.907692307692306,-0.892307692307691,
-0.876923076923076,-0.86153846153846,-0.846153846153845,-0.83076923076923,
-0.815384615384614,-0.799999999999999,-0.784615384615384,-0.769230769230768,
-0.753846153846153,-0.738461538461538,-0.723076923076922,-0.707692307692307,
-0.692307692307692,-0.676923076923076,-0.661538461538461,-0.646153846153846,
-0.63076923076923,-0.615384615384615,-0.6,-0.584615384615384,-0.569230769230769,
-0.553846153846154,-0.538461538461538,-0.523076923076923,-0.507692307692308,
-0.492307692307692,-0.476923076923077,-0.461538461538462,-0.446153846153846,
-0.430769230769231,-0.415384615384615,-0.4,-0.384615384615385,-0.369230769230769,
-0.353846153846154,-0.338461538461538,-0.323076923076923,-0.307692307692308,
-0.292307692307692,-0.276923076923077,-0.261538461538462,-0.246153846153846,
-0.230769230769231,-0.215384615384615,-0.2,-0.184615384615385,-0.169230769230769,
-0.153846153846154,-0.138461538461538,-0.123076923076923,-0.107692307692308,
-0.0923076923076923,-0.0769230769230769,-0.0615384615384615,-0.0461538461538462,
-0.0307692307692308,-0.0153846153846154,0.),(-1.,1.),.UNSPECIFIED.)
GEOMETRIC_REPRESENTATION_ITEM()
RATIONAL_B_SPLINE_SURFACE(((1.,1.),(1.,1.),(1.,1.),(1.,1.),(1.,1.),(1.,
1.),(1.,1.),(1.,1.),(1.,1.),(1.,1.),(1.,1.),(1.,1.),(1.,1.),(1.,1.),(1.,
1.),(1.,1.),(1.,1.),(1.,1.),(1.,1.),(1.,1.),(1.,1.),(1.,1.),(1.,1.),(1.,
1.),(1.,1.),(1.,1.),(1.,1.),(1.,1.),(1.,1.),(1.,1.),(1.,1.),(1.,1.),(1.,
1.),(1.,1.),(1.,1.),(1.,1.),(1.,1.),(1.,1.),(1.,1.),(1.,1.),(1.,1.),(1.,
1.),(1.,1.),(1.,1.),(1.,1.),(1.,1.),(1.,1.),(1.,1.),(1.,1.),(1.,1.),(1.,
1.),(1.,1.),(1.,1.),(1.,1.),(1.,1.),(1.,1.),(1.,1.),(1.,1.),(1.,1.),(1.,
1.),(1.,1.),(1.,1.),(1.,1.),(1.,1.),(1.,1.),(1.,1.),(1.,1.),(1.,1.),(1.,
1.),(1.,1.)))
REPRESENTATION_ITEM('')
SURFACE()
);
#104=(
BOUNDED_SURFACE()
B_SPLINE_SURFACE(5,1,((#51672,#51673),(#51674,#51675),(#51676,#51677),(#51678,
#51679),(#51680,#51681),(#51682,#51683),(#51684,#51685),(#51686,#51687),
(#51688,#51689),(#51690,#51691),(#51692,#51693),(#51694,#51695),(#51696,
#51697),(#51698,#51699),(#51700,#51701),(#51702,#51703),(#51704,#51705),
(#51706,#51707),(#51708,#51709),(#51710,#51711),(#51712,#51713),(#51714,
#51715),(#51716,#51717),(#51718,#51719),(#51720,#51721),(#51722,#51723),
(#51724,#51725),(#51726,#51727),(#51728,#51729),(#51730,#51731),(#51732,
#51733),(#51734,#51735),(#51736,#51737),(#51738,#51739),(#51740,#51741),
(#51742,#51743),(#51744,#51745),(#51746,#51747),(#51748,#51749),(#51750,
#51751),(#51752,#51753),(#51754,#51755),(#51756,#51757),(#51758,#51759),
(#51760,#51761),(#51762,#51763),(#51764,#51765),(#51766,#51767),(#51768,
#51769),(#51770,#51771),(#51772,#51773),(#51774,#51775),(#51776,#51777),
(#51778,#51779),(#51780,#51781),(#51782,#51783),(#51784,#51785),(#51786,
#51787),(#51788,#51789),(#51790,#51791),(#51792,#51793),(#51794,#51795),
(#51796,#51797),(#51798,#51799),(#51800,#51801),(#51802,#51803),(#51804,
#51805),(#51806,#51807),(#51808,#51809),(#51810,#51811)),.UNSPECIFIED.,
 .F.,.F.,.F.)
B_SPLINE_SURFACE_WITH_KNOTS((6,1,1,1,1,1,1,1,1,1,1,1,1,1,1,1,1,1,1,1,1,
1,1,1,1,1,1,1,1,1,1,1,1,1,1,1,1,1,1,1,1,1,1,1,1,1,1,1,1,1,1,1,1,1,1,1,1,
1,1,1,1,1,1,1,1,6),(2,2),(-1.,-0.984615384615383,-0.969230769230768,-0.953846153846152,
-0.938461538461537,-0.923076923076922,-0.907692307692306,-0.892307692307691,
-0.876923076923076,-0.86153846153846,-0.846153846153845,-0.83076923076923,
-0.815384615384614,-0.799999999999999,-0.784615384615384,-0.769230769230768,
-0.753846153846153,-0.738461538461538,-0.723076923076922,-0.707692307692307,
-0.692307692307692,-0.676923076923076,-0.661538461538461,-0.646153846153846,
-0.63076923076923,-0.615384615384615,-0.6,-0.584615384615384,-0.569230769230769,
-0.553846153846154,-0.538461538461538,-0.523076923076923,-0.507692307692308,
-0.492307692307692,-0.476923076923077,-0.461538461538462,-0.446153846153846,
-0.430769230769231,-0.415384615384615,-0.4,-0.384615384615385,-0.369230769230769,
-0.353846153846154,-0.338461538461538,-0.323076923076923,-0.307692307692308,
-0.292307692307692,-0.276923076923077,-0.261538461538462,-0.246153846153846,
-0.230769230769231,-0.215384615384615,-0.2,-0.184615384615385,-0.169230769230769,
-0.153846153846154,-0.138461538461538,-0.123076923076923,-0.107692307692308,
-0.0923076923076923,-0.0769230769230769,-0.0615384615384615,-0.0461538461538462,
-0.0307692307692308,-0.0153846153846154,0.),(-1.,1.),.UNSPECIFIED.)
GEOMETRIC_REPRESENTATION_ITEM()
RATIONAL_B_SPLINE_SURFACE(((1.,1.),(1.,1.),(1.,1.),(1.,1.),(1.,1.),(1.,
1.),(1.,1.),(1.,1.),(1.,1.),(1.,1.),(1.,1.),(1.,1.),(1.,1.),(1.,1.),(1.,
1.),(1.,1.),(1.,1.),(1.,1.),(1.,1.),(1.,1.),(1.,1.),(1.,1.),(1.,1.),(1.,
1.),(1.,1.),(1.,1.),(1.,1.),(1.,1.),(1.,1.),(1.,1.),(1.,1.),(1.,1.),(1.,
1.),(1.,1.),(1.,1.),(1.,1.),(1.,1.),(1.,1.),(1.,1.),(1.,1.),(1.,1.),(1.,
1.),(1.,1.),(1.,1.),(1.,1.),(1.,1.),(1.,1.),(1.,1.),(1.,1.),(1.,1.),(1.,
1.),(1.,1.),(1.,1.),(1.,1.),(1.,1.),(1.,1.),(1.,1.),(1.,1.),(1.,1.),(1.,
1.),(1.,1.),(1.,1.),(1.,1.),(1.,1.),(1.,1.),(1.,1.),(1.,1.),(1.,1.),(1.,
1.),(1.,1.)))
REPRESENTATION_ITEM('')
SURFACE()
);
#105=(
BOUNDED_SURFACE()
B_SPLINE_SURFACE(5,1,((#51902,#51903),(#51904,#51905),(#51906,#51907),(#51908,
#51909),(#51910,#51911),(#51912,#51913),(#51914,#51915),(#51916,#51917),
(#51918,#51919),(#51920,#51921),(#51922,#51923),(#51924,#51925),(#51926,
#51927),(#51928,#51929),(#51930,#51931),(#51932,#51933),(#51934,#51935),
(#51936,#51937),(#51938,#51939),(#51940,#51941),(#51942,#51943),(#51944,
#51945),(#51946,#51947),(#51948,#51949),(#51950,#51951),(#51952,#51953),
(#51954,#51955),(#51956,#51957),(#51958,#51959),(#51960,#51961),(#51962,
#51963),(#51964,#51965),(#51966,#51967),(#51968,#51969),(#51970,#51971),
(#51972,#51973),(#51974,#51975),(#51976,#51977),(#51978,#51979),(#51980,
#51981),(#51982,#51983),(#51984,#51985),(#51986,#51987),(#51988,#51989),
(#51990,#51991),(#51992,#51993),(#51994,#51995),(#51996,#51997),(#51998,
#51999),(#52000,#52001),(#52002,#52003),(#52004,#52005),(#52006,#52007),
(#52008,#52009),(#52010,#52011),(#52012,#52013),(#52014,#52015),(#52016,
#52017),(#52018,#52019),(#52020,#52021),(#52022,#52023),(#52024,#52025),
(#52026,#52027),(#52028,#52029),(#52030,#52031),(#52032,#52033),(#52034,
#52035),(#52036,#52037),(#52038,#52039),(#52040,#52041)),.UNSPECIFIED.,
 .F.,.F.,.F.)
B_SPLINE_SURFACE_WITH_KNOTS((6,1,1,1,1,1,1,1,1,1,1,1,1,1,1,1,1,1,1,1,1,
1,1,1,1,1,1,1,1,1,1,1,1,1,1,1,1,1,1,1,1,1,1,1,1,1,1,1,1,1,1,1,1,1,1,1,1,
1,1,1,1,1,1,1,1,6),(2,2),(-1.,-0.984615384615383,-0.969230769230768,-0.953846153846152,
-0.938461538461537,-0.923076923076922,-0.907692307692306,-0.892307692307691,
-0.876923076923076,-0.86153846153846,-0.846153846153845,-0.83076923076923,
-0.815384615384614,-0.799999999999999,-0.784615384615384,-0.769230769230768,
-0.753846153846153,-0.738461538461538,-0.723076923076922,-0.707692307692307,
-0.692307692307692,-0.676923076923076,-0.661538461538461,-0.646153846153846,
-0.63076923076923,-0.615384615384615,-0.6,-0.584615384615384,-0.569230769230769,
-0.553846153846154,-0.538461538461538,-0.523076923076923,-0.507692307692308,
-0.492307692307692,-0.476923076923077,-0.461538461538462,-0.446153846153846,
-0.430769230769231,-0.415384615384615,-0.4,-0.384615384615385,-0.369230769230769,
-0.353846153846154,-0.338461538461538,-0.323076923076923,-0.307692307692308,
-0.292307692307692,-0.276923076923077,-0.261538461538462,-0.246153846153846,
-0.230769230769231,-0.215384615384615,-0.2,-0.184615384615385,-0.169230769230769,
-0.153846153846154,-0.138461538461538,-0.123076923076923,-0.107692307692308,
-0.0923076923076923,-0.0769230769230769,-0.0615384615384615,-0.0461538461538462,
-0.0307692307692308,-0.0153846153846154,0.),(-1.,1.),.UNSPECIFIED.)
GEOMETRIC_REPRESENTATION_ITEM()
RATIONAL_B_SPLINE_SURFACE(((1.,1.),(1.,1.),(1.,1.),(1.,1.),(1.,1.),(1.,
1.),(1.,1.),(1.,1.),(1.,1.),(1.,1.),(1.,1.),(1.,1.),(1.,1.),(1.,1.),(1.,
1.),(1.,1.),(1.,1.),(1.,1.),(1.,1.),(1.,1.),(1.,1.),(1.,1.),(1.,1.),(1.,
1.),(1.,1.),(1.,1.),(1.,1.),(1.,1.),(1.,1.),(1.,1.),(1.,1.),(1.,1.),(1.,
1.),(1.,1.),(1.,1.),(1.,1.),(1.,1.),(1.,1.),(1.,1.),(1.,1.),(1.,1.),(1.,
1.),(1.,1.),(1.,1.),(1.,1.),(1.,1.),(1.,1.),(1.,1.),(1.,1.),(1.,1.),(1.,
1.),(1.,1.),(1.,1.),(1.,1.),(1.,1.),(1.,1.),(1.,1.),(1.,1.),(1.,1.),(1.,
1.),(1.,1.),(1.,1.),(1.,1.),(1.,1.),(1.,1.),(1.,1.),(1.,1.),(1.,1.),(1.,
1.),(1.,1.)))
REPRESENTATION_ITEM('')
SURFACE()
);
#106=(
BOUNDED_SURFACE()
B_SPLINE_SURFACE(5,1,((#52114,#52115),(#52116,#52117),(#52118,#52119),(#52120,
#52121),(#52122,#52123),(#52124,#52125),(#52126,#52127),(#52128,#52129),
(#52130,#52131),(#52132,#52133),(#52134,#52135),(#52136,#52137),(#52138,
#52139),(#52140,#52141),(#52142,#52143),(#52144,#52145),(#52146,#52147),
(#52148,#52149),(#52150,#52151),(#52152,#52153),(#52154,#52155),(#52156,
#52157),(#52158,#52159),(#52160,#52161),(#52162,#52163),(#52164,#52165),
(#52166,#52167),(#52168,#52169),(#52170,#52171),(#52172,#52173),(#52174,
#52175),(#52176,#52177),(#52178,#52179),(#52180,#52181),(#52182,#52183),
(#52184,#52185),(#52186,#52187),(#52188,#52189),(#52190,#52191),(#52192,
#52193),(#52194,#52195),(#52196,#52197),(#52198,#52199),(#52200,#52201),
(#52202,#52203),(#52204,#52205),(#52206,#52207),(#52208,#52209),(#52210,
#52211),(#52212,#52213),(#52214,#52215),(#52216,#52217),(#52218,#52219),
(#52220,#52221),(#52222,#52223),(#52224,#52225),(#52226,#52227),(#52228,
#52229),(#52230,#52231),(#52232,#52233),(#52234,#52235),(#52236,#52237),
(#52238,#52239),(#52240,#52241),(#52242,#52243),(#52244,#52245),(#52246,
#52247),(#52248,#52249),(#52250,#52251),(#52252,#52253)),.UNSPECIFIED.,
 .F.,.F.,.F.)
B_SPLINE_SURFACE_WITH_KNOTS((6,1,1,1,1,1,1,1,1,1,1,1,1,1,1,1,1,1,1,1,1,
1,1,1,1,1,1,1,1,1,1,1,1,1,1,1,1,1,1,1,1,1,1,1,1,1,1,1,1,1,1,1,1,1,1,1,1,
1,1,1,1,1,1,1,1,6),(2,2),(-1.,-0.984615384615383,-0.969230769230768,-0.953846153846152,
-0.938461538461537,-0.923076923076922,-0.907692307692306,-0.892307692307691,
-0.876923076923076,-0.86153846153846,-0.846153846153845,-0.83076923076923,
-0.815384615384614,-0.799999999999999,-0.784615384615384,-0.769230769230768,
-0.753846153846153,-0.738461538461538,-0.723076923076922,-0.707692307692307,
-0.692307692307692,-0.676923076923076,-0.661538461538461,-0.646153846153846,
-0.63076923076923,-0.615384615384615,-0.6,-0.584615384615384,-0.569230769230769,
-0.553846153846154,-0.538461538461538,-0.523076923076923,-0.507692307692308,
-0.492307692307692,-0.476923076923077,-0.461538461538462,-0.446153846153846,
-0.430769230769231,-0.415384615384615,-0.4,-0.384615384615385,-0.369230769230769,
-0.353846153846154,-0.338461538461538,-0.323076923076923,-0.307692307692308,
-0.292307692307692,-0.276923076923077,-0.261538461538462,-0.246153846153846,
-0.230769230769231,-0.215384615384615,-0.2,-0.184615384615385,-0.169230769230769,
-0.153846153846154,-0.138461538461538,-0.123076923076923,-0.107692307692308,
-0.0923076923076923,-0.0769230769230769,-0.0615384615384615,-0.0461538461538462,
-0.0307692307692308,-0.0153846153846154,0.),(-1.,1.),.UNSPECIFIED.)
GEOMETRIC_REPRESENTATION_ITEM()
RATIONAL_B_SPLINE_SURFACE(((1.,1.),(1.,1.),(1.,1.),(1.,1.),(1.,1.),(1.,
1.),(1.,1.),(1.,1.),(1.,1.),(1.,1.),(1.,1.),(1.,1.),(1.,1.),(1.,1.),(1.,
1.),(1.,1.),(1.,1.),(1.,1.),(1.,1.),(1.,1.),(1.,1.),(1.,1.),(1.,1.),(1.,
1.),(1.,1.),(1.,1.),(1.,1.),(1.,1.),(1.,1.),(1.,1.),(1.,1.),(1.,1.),(1.,
1.),(1.,1.),(1.,1.),(1.,1.),(1.,1.),(1.,1.),(1.,1.),(1.,1.),(1.,1.),(1.,
1.),(1.,1.),(1.,1.),(1.,1.),(1.,1.),(1.,1.),(1.,1.),(1.,1.),(1.,1.),(1.,
1.),(1.,1.),(1.,1.),(1.,1.),(1.,1.),(1.,1.),(1.,1.),(1.,1.),(1.,1.),(1.,
1.),(1.,1.),(1.,1.),(1.,1.),(1.,1.),(1.,1.),(1.,1.),(1.,1.),(1.,1.),(1.,
1.),(1.,1.)))
REPRESENTATION_ITEM('')
SURFACE()
);
#107=(
BOUNDED_SURFACE()
B_SPLINE_SURFACE(5,1,((#52344,#52345),(#52346,#52347),(#52348,#52349),(#52350,
#52351),(#52352,#52353),(#52354,#52355),(#52356,#52357),(#52358,#52359),
(#52360,#52361),(#52362,#52363),(#52364,#52365),(#52366,#52367),(#52368,
#52369),(#52370,#52371),(#52372,#52373),(#52374,#52375),(#52376,#52377),
(#52378,#52379),(#52380,#52381),(#52382,#52383),(#52384,#52385),(#52386,
#52387),(#52388,#52389),(#52390,#52391),(#52392,#52393),(#52394,#52395),
(#52396,#52397),(#52398,#52399),(#52400,#52401),(#52402,#52403),(#52404,
#52405),(#52406,#52407),(#52408,#52409),(#52410,#52411),(#52412,#52413),
(#52414,#52415),(#52416,#52417),(#52418,#52419),(#52420,#52421),(#52422,
#52423),(#52424,#52425),(#52426,#52427),(#52428,#52429),(#52430,#52431),
(#52432,#52433),(#52434,#52435),(#52436,#52437),(#52438,#52439),(#52440,
#52441),(#52442,#52443),(#52444,#52445),(#52446,#52447),(#52448,#52449),
(#52450,#52451),(#52452,#52453),(#52454,#52455),(#52456,#52457),(#52458,
#52459),(#52460,#52461),(#52462,#52463),(#52464,#52465),(#52466,#52467),
(#52468,#52469),(#52470,#52471),(#52472,#52473),(#52474,#52475),(#52476,
#52477),(#52478,#52479),(#52480,#52481),(#52482,#52483)),.UNSPECIFIED.,
 .F.,.F.,.F.)
B_SPLINE_SURFACE_WITH_KNOTS((6,1,1,1,1,1,1,1,1,1,1,1,1,1,1,1,1,1,1,1,1,
1,1,1,1,1,1,1,1,1,1,1,1,1,1,1,1,1,1,1,1,1,1,1,1,1,1,1,1,1,1,1,1,1,1,1,1,
1,1,1,1,1,1,1,1,6),(2,2),(-1.,-0.984615384615383,-0.969230769230768,-0.953846153846152,
-0.938461538461537,-0.923076923076922,-0.907692307692306,-0.892307692307691,
-0.876923076923076,-0.86153846153846,-0.846153846153845,-0.83076923076923,
-0.815384615384614,-0.799999999999999,-0.784615384615384,-0.769230769230768,
-0.753846153846153,-0.738461538461538,-0.723076923076922,-0.707692307692307,
-0.692307692307692,-0.676923076923076,-0.661538461538461,-0.646153846153846,
-0.63076923076923,-0.615384615384615,-0.6,-0.584615384615384,-0.569230769230769,
-0.553846153846154,-0.538461538461538,-0.523076923076923,-0.507692307692308,
-0.492307692307692,-0.476923076923077,-0.461538461538462,-0.446153846153846,
-0.430769230769231,-0.415384615384615,-0.4,-0.384615384615385,-0.369230769230769,
-0.353846153846154,-0.338461538461538,-0.323076923076923,-0.307692307692308,
-0.292307692307692,-0.276923076923077,-0.261538461538462,-0.246153846153846,
-0.230769230769231,-0.215384615384615,-0.2,-0.184615384615385,-0.169230769230769,
-0.153846153846154,-0.138461538461538,-0.123076923076923,-0.107692307692308,
-0.0923076923076923,-0.0769230769230769,-0.0615384615384615,-0.0461538461538462,
-0.0307692307692308,-0.0153846153846154,0.),(-1.,1.),.UNSPECIFIED.)
GEOMETRIC_REPRESENTATION_ITEM()
RATIONAL_B_SPLINE_SURFACE(((1.,1.),(1.,1.),(1.,1.),(1.,1.),(1.,1.),(1.,
1.),(1.,1.),(1.,1.),(1.,1.),(1.,1.),(1.,1.),(1.,1.),(1.,1.),(1.,1.),(1.,
1.),(1.,1.),(1.,1.),(1.,1.),(1.,1.),(1.,1.),(1.,1.),(1.,1.),(1.,1.),(1.,
1.),(1.,1.),(1.,1.),(1.,1.),(1.,1.),(1.,1.),(1.,1.),(1.,1.),(1.,1.),(1.,
1.),(1.,1.),(1.,1.),(1.,1.),(1.,1.),(1.,1.),(1.,1.),(1.,1.),(1.,1.),(1.,
1.),(1.,1.),(1.,1.),(1.,1.),(1.,1.),(1.,1.),(1.,1.),(1.,1.),(1.,1.),(1.,
1.),(1.,1.),(1.,1.),(1.,1.),(1.,1.),(1.,1.),(1.,1.),(1.,1.),(1.,1.),(1.,
1.),(1.,1.),(1.,1.),(1.,1.),(1.,1.),(1.,1.),(1.,1.),(1.,1.),(1.,1.),(1.,
1.),(1.,1.)))
REPRESENTATION_ITEM('')
SURFACE()
);
#108=(
BOUNDED_SURFACE()
B_SPLINE_SURFACE(5,1,((#52556,#52557),(#52558,#52559),(#52560,#52561),(#52562,
#52563),(#52564,#52565),(#52566,#52567),(#52568,#52569),(#52570,#52571),
(#52572,#52573),(#52574,#52575),(#52576,#52577),(#52578,#52579),(#52580,
#52581),(#52582,#52583),(#52584,#52585),(#52586,#52587),(#52588,#52589),
(#52590,#52591),(#52592,#52593),(#52594,#52595),(#52596,#52597),(#52598,
#52599),(#52600,#52601),(#52602,#52603),(#52604,#52605),(#52606,#52607),
(#52608,#52609),(#52610,#52611),(#52612,#52613),(#52614,#52615),(#52616,
#52617),(#52618,#52619),(#52620,#52621),(#52622,#52623),(#52624,#52625),
(#52626,#52627),(#52628,#52629),(#52630,#52631),(#52632,#52633),(#52634,
#52635),(#52636,#52637),(#52638,#52639),(#52640,#52641),(#52642,#52643),
(#52644,#52645),(#52646,#52647),(#52648,#52649),(#52650,#52651),(#52652,
#52653),(#52654,#52655),(#52656,#52657),(#52658,#52659),(#52660,#52661),
(#52662,#52663),(#52664,#52665),(#52666,#52667),(#52668,#52669),(#52670,
#52671),(#52672,#52673),(#52674,#52675),(#52676,#52677),(#52678,#52679),
(#52680,#52681),(#52682,#52683),(#52684,#52685),(#52686,#52687),(#52688,
#52689),(#52690,#52691),(#52692,#52693),(#52694,#52695)),.UNSPECIFIED.,
 .F.,.F.,.F.)
B_SPLINE_SURFACE_WITH_KNOTS((6,1,1,1,1,1,1,1,1,1,1,1,1,1,1,1,1,1,1,1,1,
1,1,1,1,1,1,1,1,1,1,1,1,1,1,1,1,1,1,1,1,1,1,1,1,1,1,1,1,1,1,1,1,1,1,1,1,
1,1,1,1,1,1,1,1,6),(2,2),(-1.,-0.984615384615383,-0.969230769230768,-0.953846153846152,
-0.938461538461537,-0.923076923076922,-0.907692307692306,-0.892307692307691,
-0.876923076923076,-0.86153846153846,-0.846153846153845,-0.83076923076923,
-0.815384615384614,-0.799999999999999,-0.784615384615384,-0.769230769230768,
-0.753846153846153,-0.738461538461538,-0.723076923076922,-0.707692307692307,
-0.692307692307692,-0.676923076923076,-0.661538461538461,-0.646153846153846,
-0.63076923076923,-0.615384615384615,-0.6,-0.584615384615384,-0.569230769230769,
-0.553846153846154,-0.538461538461538,-0.523076923076923,-0.507692307692308,
-0.492307692307692,-0.476923076923077,-0.461538461538462,-0.446153846153846,
-0.430769230769231,-0.415384615384615,-0.4,-0.384615384615385,-0.369230769230769,
-0.353846153846154,-0.338461538461538,-0.323076923076923,-0.307692307692308,
-0.292307692307692,-0.276923076923077,-0.261538461538462,-0.246153846153846,
-0.230769230769231,-0.215384615384615,-0.2,-0.184615384615385,-0.169230769230769,
-0.153846153846154,-0.138461538461538,-0.123076923076923,-0.107692307692308,
-0.0923076923076923,-0.0769230769230769,-0.0615384615384615,-0.0461538461538462,
-0.0307692307692308,-0.0153846153846154,0.),(-1.,1.),.UNSPECIFIED.)
GEOMETRIC_REPRESENTATION_ITEM()
RATIONAL_B_SPLINE_SURFACE(((1.,1.),(1.,1.),(1.,1.),(1.,1.),(1.,1.),(1.,
1.),(1.,1.),(1.,1.),(1.,1.),(1.,1.),(1.,1.),(1.,1.),(1.,1.),(1.,1.),(1.,
1.),(1.,1.),(1.,1.),(1.,1.),(1.,1.),(1.,1.),(1.,1.),(1.,1.),(1.,1.),(1.,
1.),(1.,1.),(1.,1.),(1.,1.),(1.,1.),(1.,1.),(1.,1.),(1.,1.),(1.,1.),(1.,
1.),(1.,1.),(1.,1.),(1.,1.),(1.,1.),(1.,1.),(1.,1.),(1.,1.),(1.,1.),(1.,
1.),(1.,1.),(1.,1.),(1.,1.),(1.,1.),(1.,1.),(1.,1.),(1.,1.),(1.,1.),(1.,
1.),(1.,1.),(1.,1.),(1.,1.),(1.,1.),(1.,1.),(1.,1.),(1.,1.),(1.,1.),(1.,
1.),(1.,1.),(1.,1.),(1.,1.),(1.,1.),(1.,1.),(1.,1.),(1.,1.),(1.,1.),(1.,
1.),(1.,1.)))
REPRESENTATION_ITEM('')
SURFACE()
);
#109=(
BOUNDED_SURFACE()
B_SPLINE_SURFACE(5,1,((#52786,#52787),(#52788,#52789),(#52790,#52791),(#52792,
#52793),(#52794,#52795),(#52796,#52797),(#52798,#52799),(#52800,#52801),
(#52802,#52803),(#52804,#52805),(#52806,#52807),(#52808,#52809),(#52810,
#52811),(#52812,#52813),(#52814,#52815),(#52816,#52817),(#52818,#52819),
(#52820,#52821),(#52822,#52823),(#52824,#52825),(#52826,#52827),(#52828,
#52829),(#52830,#52831),(#52832,#52833),(#52834,#52835),(#52836,#52837),
(#52838,#52839),(#52840,#52841),(#52842,#52843),(#52844,#52845),(#52846,
#52847),(#52848,#52849),(#52850,#52851),(#52852,#52853),(#52854,#52855),
(#52856,#52857),(#52858,#52859),(#52860,#52861),(#52862,#52863),(#52864,
#52865),(#52866,#52867),(#52868,#52869),(#52870,#52871),(#52872,#52873),
(#52874,#52875),(#52876,#52877),(#52878,#52879),(#52880,#52881),(#52882,
#52883),(#52884,#52885),(#52886,#52887),(#52888,#52889),(#52890,#52891),
(#52892,#52893),(#52894,#52895),(#52896,#52897),(#52898,#52899),(#52900,
#52901),(#52902,#52903),(#52904,#52905),(#52906,#52907),(#52908,#52909),
(#52910,#52911),(#52912,#52913),(#52914,#52915),(#52916,#52917),(#52918,
#52919),(#52920,#52921),(#52922,#52923),(#52924,#52925)),.UNSPECIFIED.,
 .F.,.F.,.F.)
B_SPLINE_SURFACE_WITH_KNOTS((6,1,1,1,1,1,1,1,1,1,1,1,1,1,1,1,1,1,1,1,1,
1,1,1,1,1,1,1,1,1,1,1,1,1,1,1,1,1,1,1,1,1,1,1,1,1,1,1,1,1,1,1,1,1,1,1,1,
1,1,1,1,1,1,1,1,6),(2,2),(-1.,-0.984615384615383,-0.969230769230768,-0.953846153846152,
-0.938461538461537,-0.923076923076922,-0.907692307692306,-0.892307692307691,
-0.876923076923076,-0.86153846153846,-0.846153846153845,-0.83076923076923,
-0.815384615384614,-0.799999999999999,-0.784615384615384,-0.769230769230768,
-0.753846153846153,-0.738461538461538,-0.723076923076922,-0.707692307692307,
-0.692307692307692,-0.676923076923076,-0.661538461538461,-0.646153846153846,
-0.63076923076923,-0.615384615384615,-0.6,-0.584615384615384,-0.569230769230769,
-0.553846153846154,-0.538461538461538,-0.523076923076923,-0.507692307692308,
-0.492307692307692,-0.476923076923077,-0.461538461538462,-0.446153846153846,
-0.430769230769231,-0.415384615384615,-0.4,-0.384615384615385,-0.369230769230769,
-0.353846153846154,-0.338461538461538,-0.323076923076923,-0.307692307692308,
-0.292307692307692,-0.276923076923077,-0.261538461538462,-0.246153846153846,
-0.230769230769231,-0.215384615384615,-0.2,-0.184615384615385,-0.169230769230769,
-0.153846153846154,-0.138461538461538,-0.123076923076923,-0.107692307692308,
-0.0923076923076923,-0.0769230769230769,-0.0615384615384615,-0.0461538461538462,
-0.0307692307692308,-0.0153846153846154,0.),(-1.,1.),.UNSPECIFIED.)
GEOMETRIC_REPRESENTATION_ITEM()
RATIONAL_B_SPLINE_SURFACE(((1.,1.),(1.,1.),(1.,1.),(1.,1.),(1.,1.),(1.,
1.),(1.,1.),(1.,1.),(1.,1.),(1.,1.),(1.,1.),(1.,1.),(1.,1.),(1.,1.),(1.,
1.),(1.,1.),(1.,1.),(1.,1.),(1.,1.),(1.,1.),(1.,1.),(1.,1.),(1.,1.),(1.,
1.),(1.,1.),(1.,1.),(1.,1.),(1.,1.),(1.,1.),(1.,1.),(1.,1.),(1.,1.),(1.,
1.),(1.,1.),(1.,1.),(1.,1.),(1.,1.),(1.,1.),(1.,1.),(1.,1.),(1.,1.),(1.,
1.),(1.,1.),(1.,1.),(1.,1.),(1.,1.),(1.,1.),(1.,1.),(1.,1.),(1.,1.),(1.,
1.),(1.,1.),(1.,1.),(1.,1.),(1.,1.),(1.,1.),(1.,1.),(1.,1.),(1.,1.),(1.,
1.),(1.,1.),(1.,1.),(1.,1.),(1.,1.),(1.,1.),(1.,1.),(1.,1.),(1.,1.),(1.,
1.),(1.,1.)))
REPRESENTATION_ITEM('')
SURFACE()
);
#110=(
BOUNDED_SURFACE()
B_SPLINE_SURFACE(5,1,((#52998,#52999),(#53000,#53001),(#53002,#53003),(#53004,
#53005),(#53006,#53007),(#53008,#53009),(#53010,#53011),(#53012,#53013),
(#53014,#53015),(#53016,#53017),(#53018,#53019),(#53020,#53021),(#53022,
#53023),(#53024,#53025),(#53026,#53027),(#53028,#53029),(#53030,#53031),
(#53032,#53033),(#53034,#53035),(#53036,#53037),(#53038,#53039),(#53040,
#53041),(#53042,#53043),(#53044,#53045),(#53046,#53047),(#53048,#53049),
(#53050,#53051),(#53052,#53053),(#53054,#53055),(#53056,#53057),(#53058,
#53059),(#53060,#53061),(#53062,#53063),(#53064,#53065),(#53066,#53067),
(#53068,#53069),(#53070,#53071),(#53072,#53073),(#53074,#53075),(#53076,
#53077),(#53078,#53079),(#53080,#53081),(#53082,#53083),(#53084,#53085),
(#53086,#53087),(#53088,#53089),(#53090,#53091),(#53092,#53093),(#53094,
#53095),(#53096,#53097),(#53098,#53099),(#53100,#53101),(#53102,#53103),
(#53104,#53105),(#53106,#53107),(#53108,#53109),(#53110,#53111),(#53112,
#53113),(#53114,#53115),(#53116,#53117),(#53118,#53119),(#53120,#53121),
(#53122,#53123),(#53124,#53125),(#53126,#53127),(#53128,#53129),(#53130,
#53131),(#53132,#53133),(#53134,#53135),(#53136,#53137)),.UNSPECIFIED.,
 .F.,.F.,.F.)
B_SPLINE_SURFACE_WITH_KNOTS((6,1,1,1,1,1,1,1,1,1,1,1,1,1,1,1,1,1,1,1,1,
1,1,1,1,1,1,1,1,1,1,1,1,1,1,1,1,1,1,1,1,1,1,1,1,1,1,1,1,1,1,1,1,1,1,1,1,
1,1,1,1,1,1,1,1,6),(2,2),(-1.,-0.984615384615383,-0.969230769230768,-0.953846153846152,
-0.938461538461537,-0.923076923076922,-0.907692307692306,-0.892307692307691,
-0.876923076923076,-0.86153846153846,-0.846153846153845,-0.83076923076923,
-0.815384615384614,-0.799999999999999,-0.784615384615384,-0.769230769230768,
-0.753846153846153,-0.738461538461538,-0.723076923076922,-0.707692307692307,
-0.692307692307692,-0.676923076923076,-0.661538461538461,-0.646153846153846,
-0.63076923076923,-0.615384615384615,-0.6,-0.584615384615384,-0.569230769230769,
-0.553846153846154,-0.538461538461538,-0.523076923076923,-0.507692307692308,
-0.492307692307692,-0.476923076923077,-0.461538461538462,-0.446153846153846,
-0.430769230769231,-0.415384615384615,-0.4,-0.384615384615385,-0.369230769230769,
-0.353846153846154,-0.338461538461538,-0.323076923076923,-0.307692307692308,
-0.292307692307692,-0.276923076923077,-0.261538461538462,-0.246153846153846,
-0.230769230769231,-0.215384615384615,-0.2,-0.184615384615385,-0.169230769230769,
-0.153846153846154,-0.138461538461538,-0.123076923076923,-0.107692307692308,
-0.0923076923076923,-0.0769230769230769,-0.0615384615384615,-0.0461538461538462,
-0.0307692307692308,-0.0153846153846154,0.),(-1.,1.),.UNSPECIFIED.)
GEOMETRIC_REPRESENTATION_ITEM()
RATIONAL_B_SPLINE_SURFACE(((1.,1.),(1.,1.),(1.,1.),(1.,1.),(1.,1.),(1.,
1.),(1.,1.),(1.,1.),(1.,1.),(1.,1.),(1.,1.),(1.,1.),(1.,1.),(1.,1.),(1.,
1.),(1.,1.),(1.,1.),(1.,1.),(1.,1.),(1.,1.),(1.,1.),(1.,1.),(1.,1.),(1.,
1.),(1.,1.),(1.,1.),(1.,1.),(1.,1.),(1.,1.),(1.,1.),(1.,1.),(1.,1.),(1.,
1.),(1.,1.),(1.,1.),(1.,1.),(1.,1.),(1.,1.),(1.,1.),(1.,1.),(1.,1.),(1.,
1.),(1.,1.),(1.,1.),(1.,1.),(1.,1.),(1.,1.),(1.,1.),(1.,1.),(1.,1.),(1.,
1.),(1.,1.),(1.,1.),(1.,1.),(1.,1.),(1.,1.),(1.,1.),(1.,1.),(1.,1.),(1.,
1.),(1.,1.),(1.,1.),(1.,1.),(1.,1.),(1.,1.),(1.,1.),(1.,1.),(1.,1.),(1.,
1.),(1.,1.)))
REPRESENTATION_ITEM('')
SURFACE()
);
#111=(
BOUNDED_SURFACE()
B_SPLINE_SURFACE(5,1,((#53228,#53229),(#53230,#53231),(#53232,#53233),(#53234,
#53235),(#53236,#53237),(#53238,#53239),(#53240,#53241),(#53242,#53243),
(#53244,#53245),(#53246,#53247),(#53248,#53249),(#53250,#53251),(#53252,
#53253),(#53254,#53255),(#53256,#53257),(#53258,#53259),(#53260,#53261),
(#53262,#53263),(#53264,#53265),(#53266,#53267),(#53268,#53269),(#53270,
#53271),(#53272,#53273),(#53274,#53275),(#53276,#53277),(#53278,#53279),
(#53280,#53281),(#53282,#53283),(#53284,#53285),(#53286,#53287),(#53288,
#53289),(#53290,#53291),(#53292,#53293),(#53294,#53295),(#53296,#53297),
(#53298,#53299),(#53300,#53301),(#53302,#53303),(#53304,#53305),(#53306,
#53307),(#53308,#53309),(#53310,#53311),(#53312,#53313),(#53314,#53315),
(#53316,#53317),(#53318,#53319),(#53320,#53321),(#53322,#53323),(#53324,
#53325),(#53326,#53327),(#53328,#53329),(#53330,#53331),(#53332,#53333),
(#53334,#53335),(#53336,#53337),(#53338,#53339),(#53340,#53341),(#53342,
#53343),(#53344,#53345),(#53346,#53347),(#53348,#53349),(#53350,#53351),
(#53352,#53353),(#53354,#53355),(#53356,#53357),(#53358,#53359),(#53360,
#53361),(#53362,#53363),(#53364,#53365),(#53366,#53367)),.UNSPECIFIED.,
 .F.,.F.,.F.)
B_SPLINE_SURFACE_WITH_KNOTS((6,1,1,1,1,1,1,1,1,1,1,1,1,1,1,1,1,1,1,1,1,
1,1,1,1,1,1,1,1,1,1,1,1,1,1,1,1,1,1,1,1,1,1,1,1,1,1,1,1,1,1,1,1,1,1,1,1,
1,1,1,1,1,1,1,1,6),(2,2),(-1.,-0.984615384615383,-0.969230769230768,-0.953846153846152,
-0.938461538461537,-0.923076923076922,-0.907692307692306,-0.892307692307691,
-0.876923076923076,-0.86153846153846,-0.846153846153845,-0.83076923076923,
-0.815384615384614,-0.799999999999999,-0.784615384615384,-0.769230769230768,
-0.753846153846153,-0.738461538461538,-0.723076923076922,-0.707692307692307,
-0.692307692307692,-0.676923076923076,-0.661538461538461,-0.646153846153846,
-0.63076923076923,-0.615384615384615,-0.6,-0.584615384615384,-0.569230769230769,
-0.553846153846154,-0.538461538461538,-0.523076923076923,-0.507692307692308,
-0.492307692307692,-0.476923076923077,-0.461538461538462,-0.446153846153846,
-0.430769230769231,-0.415384615384615,-0.4,-0.384615384615385,-0.369230769230769,
-0.353846153846154,-0.338461538461538,-0.323076923076923,-0.307692307692308,
-0.292307692307692,-0.276923076923077,-0.261538461538462,-0.246153846153846,
-0.230769230769231,-0.215384615384615,-0.2,-0.184615384615385,-0.169230769230769,
-0.153846153846154,-0.138461538461538,-0.123076923076923,-0.107692307692308,
-0.0923076923076923,-0.0769230769230769,-0.0615384615384615,-0.0461538461538462,
-0.0307692307692308,-0.0153846153846154,0.),(-1.,1.),.UNSPECIFIED.)
GEOMETRIC_REPRESENTATION_ITEM()
RATIONAL_B_SPLINE_SURFACE(((1.,1.),(1.,1.),(1.,1.),(1.,1.),(1.,1.),(1.,
1.),(1.,1.),(1.,1.),(1.,1.),(1.,1.),(1.,1.),(1.,1.),(1.,1.),(1.,1.),(1.,
1.),(1.,1.),(1.,1.),(1.,1.),(1.,1.),(1.,1.),(1.,1.),(1.,1.),(1.,1.),(1.,
1.),(1.,1.),(1.,1.),(1.,1.),(1.,1.),(1.,1.),(1.,1.),(1.,1.),(1.,1.),(1.,
1.),(1.,1.),(1.,1.),(1.,1.),(1.,1.),(1.,1.),(1.,1.),(1.,1.),(1.,1.),(1.,
1.),(1.,1.),(1.,1.),(1.,1.),(1.,1.),(1.,1.),(1.,1.),(1.,1.),(1.,1.),(1.,
1.),(1.,1.),(1.,1.),(1.,1.),(1.,1.),(1.,1.),(1.,1.),(1.,1.),(1.,1.),(1.,
1.),(1.,1.),(1.,1.),(1.,1.),(1.,1.),(1.,1.),(1.,1.),(1.,1.),(1.,1.),(1.,
1.),(1.,1.)))
REPRESENTATION_ITEM('')
SURFACE()
);
#112=(
BOUNDED_SURFACE()
B_SPLINE_SURFACE(5,1,((#53440,#53441),(#53442,#53443),(#53444,#53445),(#53446,
#53447),(#53448,#53449),(#53450,#53451),(#53452,#53453),(#53454,#53455),
(#53456,#53457),(#53458,#53459),(#53460,#53461),(#53462,#53463),(#53464,
#53465),(#53466,#53467),(#53468,#53469),(#53470,#53471),(#53472,#53473),
(#53474,#53475),(#53476,#53477),(#53478,#53479),(#53480,#53481),(#53482,
#53483),(#53484,#53485),(#53486,#53487),(#53488,#53489),(#53490,#53491),
(#53492,#53493),(#53494,#53495),(#53496,#53497),(#53498,#53499),(#53500,
#53501),(#53502,#53503),(#53504,#53505),(#53506,#53507),(#53508,#53509),
(#53510,#53511),(#53512,#53513),(#53514,#53515),(#53516,#53517),(#53518,
#53519),(#53520,#53521),(#53522,#53523),(#53524,#53525),(#53526,#53527),
(#53528,#53529),(#53530,#53531),(#53532,#53533),(#53534,#53535),(#53536,
#53537),(#53538,#53539),(#53540,#53541),(#53542,#53543),(#53544,#53545),
(#53546,#53547),(#53548,#53549),(#53550,#53551),(#53552,#53553),(#53554,
#53555),(#53556,#53557),(#53558,#53559),(#53560,#53561),(#53562,#53563),
(#53564,#53565),(#53566,#53567),(#53568,#53569),(#53570,#53571),(#53572,
#53573),(#53574,#53575),(#53576,#53577),(#53578,#53579)),.UNSPECIFIED.,
 .F.,.F.,.F.)
B_SPLINE_SURFACE_WITH_KNOTS((6,1,1,1,1,1,1,1,1,1,1,1,1,1,1,1,1,1,1,1,1,
1,1,1,1,1,1,1,1,1,1,1,1,1,1,1,1,1,1,1,1,1,1,1,1,1,1,1,1,1,1,1,1,1,1,1,1,
1,1,1,1,1,1,1,1,6),(2,2),(-1.,-0.984615384615383,-0.969230769230768,-0.953846153846152,
-0.938461538461537,-0.923076923076922,-0.907692307692306,-0.892307692307691,
-0.876923076923076,-0.86153846153846,-0.846153846153845,-0.83076923076923,
-0.815384615384614,-0.799999999999999,-0.784615384615384,-0.769230769230768,
-0.753846153846153,-0.738461538461538,-0.723076923076922,-0.707692307692307,
-0.692307692307692,-0.676923076923076,-0.661538461538461,-0.646153846153846,
-0.63076923076923,-0.615384615384615,-0.6,-0.584615384615384,-0.569230769230769,
-0.553846153846154,-0.538461538461538,-0.523076923076923,-0.507692307692308,
-0.492307692307692,-0.476923076923077,-0.461538461538462,-0.446153846153846,
-0.430769230769231,-0.415384615384615,-0.4,-0.384615384615385,-0.369230769230769,
-0.353846153846154,-0.338461538461538,-0.323076923076923,-0.307692307692308,
-0.292307692307692,-0.276923076923077,-0.261538461538462,-0.246153846153846,
-0.230769230769231,-0.215384615384615,-0.2,-0.184615384615385,-0.169230769230769,
-0.153846153846154,-0.138461538461538,-0.123076923076923,-0.107692307692308,
-0.0923076923076923,-0.0769230769230769,-0.0615384615384615,-0.0461538461538462,
-0.0307692307692308,-0.0153846153846154,0.),(-1.,1.),.UNSPECIFIED.)
GEOMETRIC_REPRESENTATION_ITEM()
RATIONAL_B_SPLINE_SURFACE(((1.,1.),(1.,1.),(1.,1.),(1.,1.),(1.,1.),(1.,
1.),(1.,1.),(1.,1.),(1.,1.),(1.,1.),(1.,1.),(1.,1.),(1.,1.),(1.,1.),(1.,
1.),(1.,1.),(1.,1.),(1.,1.),(1.,1.),(1.,1.),(1.,1.),(1.,1.),(1.,1.),(1.,
1.),(1.,1.),(1.,1.),(1.,1.),(1.,1.),(1.,1.),(1.,1.),(1.,1.),(1.,1.),(1.,
1.),(1.,1.),(1.,1.),(1.,1.),(1.,1.),(1.,1.),(1.,1.),(1.,1.),(1.,1.),(1.,
1.),(1.,1.),(1.,1.),(1.,1.),(1.,1.),(1.,1.),(1.,1.),(1.,1.),(1.,1.),(1.,
1.),(1.,1.),(1.,1.),(1.,1.),(1.,1.),(1.,1.),(1.,1.),(1.,1.),(1.,1.),(1.,
1.),(1.,1.),(1.,1.),(1.,1.),(1.,1.),(1.,1.),(1.,1.),(1.,1.),(1.,1.),(1.,
1.),(1.,1.)))
REPRESENTATION_ITEM('')
SURFACE()
);
#113=(
BOUNDED_SURFACE()
B_SPLINE_SURFACE(5,1,((#53670,#53671),(#53672,#53673),(#53674,#53675),(#53676,
#53677),(#53678,#53679),(#53680,#53681),(#53682,#53683),(#53684,#53685),
(#53686,#53687),(#53688,#53689),(#53690,#53691),(#53692,#53693),(#53694,
#53695),(#53696,#53697),(#53698,#53699),(#53700,#53701),(#53702,#53703),
(#53704,#53705),(#53706,#53707),(#53708,#53709),(#53710,#53711),(#53712,
#53713),(#53714,#53715),(#53716,#53717),(#53718,#53719),(#53720,#53721),
(#53722,#53723),(#53724,#53725),(#53726,#53727),(#53728,#53729),(#53730,
#53731),(#53732,#53733),(#53734,#53735),(#53736,#53737),(#53738,#53739),
(#53740,#53741),(#53742,#53743),(#53744,#53745),(#53746,#53747),(#53748,
#53749),(#53750,#53751),(#53752,#53753),(#53754,#53755),(#53756,#53757),
(#53758,#53759),(#53760,#53761),(#53762,#53763),(#53764,#53765),(#53766,
#53767),(#53768,#53769),(#53770,#53771),(#53772,#53773),(#53774,#53775),
(#53776,#53777),(#53778,#53779),(#53780,#53781),(#53782,#53783),(#53784,
#53785),(#53786,#53787),(#53788,#53789),(#53790,#53791),(#53792,#53793),
(#53794,#53795),(#53796,#53797),(#53798,#53799),(#53800,#53801),(#53802,
#53803),(#53804,#53805),(#53806,#53807),(#53808,#53809)),.UNSPECIFIED.,
 .F.,.F.,.F.)
B_SPLINE_SURFACE_WITH_KNOTS((6,1,1,1,1,1,1,1,1,1,1,1,1,1,1,1,1,1,1,1,1,
1,1,1,1,1,1,1,1,1,1,1,1,1,1,1,1,1,1,1,1,1,1,1,1,1,1,1,1,1,1,1,1,1,1,1,1,
1,1,1,1,1,1,1,1,6),(2,2),(-1.,-0.984615384615383,-0.969230769230768,-0.953846153846152,
-0.938461538461537,-0.923076923076922,-0.907692307692306,-0.892307692307691,
-0.876923076923076,-0.86153846153846,-0.846153846153845,-0.83076923076923,
-0.815384615384614,-0.799999999999999,-0.784615384615384,-0.769230769230768,
-0.753846153846153,-0.738461538461538,-0.723076923076922,-0.707692307692307,
-0.692307692307692,-0.676923076923076,-0.661538461538461,-0.646153846153846,
-0.63076923076923,-0.615384615384615,-0.6,-0.584615384615384,-0.569230769230769,
-0.553846153846154,-0.538461538461538,-0.523076923076923,-0.507692307692308,
-0.492307692307692,-0.476923076923077,-0.461538461538462,-0.446153846153846,
-0.430769230769231,-0.415384615384615,-0.4,-0.384615384615385,-0.369230769230769,
-0.353846153846154,-0.338461538461538,-0.323076923076923,-0.307692307692308,
-0.292307692307692,-0.276923076923077,-0.261538461538462,-0.246153846153846,
-0.230769230769231,-0.215384615384615,-0.2,-0.184615384615385,-0.169230769230769,
-0.153846153846154,-0.138461538461538,-0.123076923076923,-0.107692307692308,
-0.0923076923076923,-0.0769230769230769,-0.0615384615384615,-0.0461538461538462,
-0.0307692307692308,-0.0153846153846154,0.),(-1.,1.),.UNSPECIFIED.)
GEOMETRIC_REPRESENTATION_ITEM()
RATIONAL_B_SPLINE_SURFACE(((1.,1.),(1.,1.),(1.,1.),(1.,1.),(1.,1.),(1.,
1.),(1.,1.),(1.,1.),(1.,1.),(1.,1.),(1.,1.),(1.,1.),(1.,1.),(1.,1.),(1.,
1.),(1.,1.),(1.,1.),(1.,1.),(1.,1.),(1.,1.),(1.,1.),(1.,1.),(1.,1.),(1.,
1.),(1.,1.),(1.,1.),(1.,1.),(1.,1.),(1.,1.),(1.,1.),(1.,1.),(1.,1.),(1.,
1.),(1.,1.),(1.,1.),(1.,1.),(1.,1.),(1.,1.),(1.,1.),(1.,1.),(1.,1.),(1.,
1.),(1.,1.),(1.,1.),(1.,1.),(1.,1.),(1.,1.),(1.,1.),(1.,1.),(1.,1.),(1.,
1.),(1.,1.),(1.,1.),(1.,1.),(1.,1.),(1.,1.),(1.,1.),(1.,1.),(1.,1.),(1.,
1.),(1.,1.),(1.,1.),(1.,1.),(1.,1.),(1.,1.),(1.,1.),(1.,1.),(1.,1.),(1.,
1.),(1.,1.)))
REPRESENTATION_ITEM('')
SURFACE()
);
#114=(
BOUNDED_SURFACE()
B_SPLINE_SURFACE(5,1,((#53882,#53883),(#53884,#53885),(#53886,#53887),(#53888,
#53889),(#53890,#53891),(#53892,#53893),(#53894,#53895),(#53896,#53897),
(#53898,#53899),(#53900,#53901),(#53902,#53903),(#53904,#53905),(#53906,
#53907),(#53908,#53909),(#53910,#53911),(#53912,#53913),(#53914,#53915),
(#53916,#53917),(#53918,#53919),(#53920,#53921),(#53922,#53923),(#53924,
#53925),(#53926,#53927),(#53928,#53929),(#53930,#53931),(#53932,#53933),
(#53934,#53935),(#53936,#53937),(#53938,#53939),(#53940,#53941),(#53942,
#53943),(#53944,#53945),(#53946,#53947),(#53948,#53949),(#53950,#53951),
(#53952,#53953),(#53954,#53955),(#53956,#53957),(#53958,#53959),(#53960,
#53961),(#53962,#53963),(#53964,#53965),(#53966,#53967),(#53968,#53969),
(#53970,#53971),(#53972,#53973),(#53974,#53975),(#53976,#53977),(#53978,
#53979),(#53980,#53981),(#53982,#53983),(#53984,#53985),(#53986,#53987),
(#53988,#53989),(#53990,#53991),(#53992,#53993),(#53994,#53995),(#53996,
#53997),(#53998,#53999),(#54000,#54001),(#54002,#54003),(#54004,#54005),
(#54006,#54007),(#54008,#54009),(#54010,#54011),(#54012,#54013),(#54014,
#54015),(#54016,#54017),(#54018,#54019),(#54020,#54021)),.UNSPECIFIED.,
 .F.,.F.,.F.)
B_SPLINE_SURFACE_WITH_KNOTS((6,1,1,1,1,1,1,1,1,1,1,1,1,1,1,1,1,1,1,1,1,
1,1,1,1,1,1,1,1,1,1,1,1,1,1,1,1,1,1,1,1,1,1,1,1,1,1,1,1,1,1,1,1,1,1,1,1,
1,1,1,1,1,1,1,1,6),(2,2),(-1.,-0.984615384615383,-0.969230769230768,-0.953846153846152,
-0.938461538461537,-0.923076923076922,-0.907692307692306,-0.892307692307691,
-0.876923076923076,-0.86153846153846,-0.846153846153845,-0.83076923076923,
-0.815384615384614,-0.799999999999999,-0.784615384615384,-0.769230769230768,
-0.753846153846153,-0.738461538461538,-0.723076923076922,-0.707692307692307,
-0.692307692307692,-0.676923076923076,-0.661538461538461,-0.646153846153846,
-0.63076923076923,-0.615384615384615,-0.6,-0.584615384615384,-0.569230769230769,
-0.553846153846154,-0.538461538461538,-0.523076923076923,-0.507692307692308,
-0.492307692307692,-0.476923076923077,-0.461538461538462,-0.446153846153846,
-0.430769230769231,-0.415384615384615,-0.4,-0.384615384615385,-0.369230769230769,
-0.353846153846154,-0.338461538461538,-0.323076923076923,-0.307692307692308,
-0.292307692307692,-0.276923076923077,-0.261538461538462,-0.246153846153846,
-0.230769230769231,-0.215384615384615,-0.2,-0.184615384615385,-0.169230769230769,
-0.153846153846154,-0.138461538461538,-0.123076923076923,-0.107692307692308,
-0.0923076923076923,-0.0769230769230769,-0.0615384615384615,-0.0461538461538462,
-0.0307692307692308,-0.0153846153846154,0.),(-1.,1.),.UNSPECIFIED.)
GEOMETRIC_REPRESENTATION_ITEM()
RATIONAL_B_SPLINE_SURFACE(((1.,1.),(1.,1.),(1.,1.),(1.,1.),(1.,1.),(1.,
1.),(1.,1.),(1.,1.),(1.,1.),(1.,1.),(1.,1.),(1.,1.),(1.,1.),(1.,1.),(1.,
1.),(1.,1.),(1.,1.),(1.,1.),(1.,1.),(1.,1.),(1.,1.),(1.,1.),(1.,1.),(1.,
1.),(1.,1.),(1.,1.),(1.,1.),(1.,1.),(1.,1.),(1.,1.),(1.,1.),(1.,1.),(1.,
1.),(1.,1.),(1.,1.),(1.,1.),(1.,1.),(1.,1.),(1.,1.),(1.,1.),(1.,1.),(1.,
1.),(1.,1.),(1.,1.),(1.,1.),(1.,1.),(1.,1.),(1.,1.),(1.,1.),(1.,1.),(1.,
1.),(1.,1.),(1.,1.),(1.,1.),(1.,1.),(1.,1.),(1.,1.),(1.,1.),(1.,1.),(1.,
1.),(1.,1.),(1.,1.),(1.,1.),(1.,1.),(1.,1.),(1.,1.),(1.,1.),(1.,1.),(1.,
1.),(1.,1.)))
REPRESENTATION_ITEM('')
SURFACE()
);
#115=(
BOUNDED_SURFACE()
B_SPLINE_SURFACE(5,1,((#54112,#54113),(#54114,#54115),(#54116,#54117),(#54118,
#54119),(#54120,#54121),(#54122,#54123),(#54124,#54125),(#54126,#54127),
(#54128,#54129),(#54130,#54131),(#54132,#54133),(#54134,#54135),(#54136,
#54137),(#54138,#54139),(#54140,#54141),(#54142,#54143),(#54144,#54145),
(#54146,#54147),(#54148,#54149),(#54150,#54151),(#54152,#54153),(#54154,
#54155),(#54156,#54157),(#54158,#54159),(#54160,#54161),(#54162,#54163),
(#54164,#54165),(#54166,#54167),(#54168,#54169),(#54170,#54171),(#54172,
#54173),(#54174,#54175),(#54176,#54177),(#54178,#54179),(#54180,#54181),
(#54182,#54183),(#54184,#54185),(#54186,#54187),(#54188,#54189),(#54190,
#54191),(#54192,#54193),(#54194,#54195),(#54196,#54197),(#54198,#54199),
(#54200,#54201),(#54202,#54203),(#54204,#54205),(#54206,#54207),(#54208,
#54209),(#54210,#54211),(#54212,#54213),(#54214,#54215),(#54216,#54217),
(#54218,#54219),(#54220,#54221),(#54222,#54223),(#54224,#54225),(#54226,
#54227),(#54228,#54229),(#54230,#54231),(#54232,#54233),(#54234,#54235),
(#54236,#54237),(#54238,#54239),(#54240,#54241),(#54242,#54243),(#54244,
#54245),(#54246,#54247),(#54248,#54249),(#54250,#54251)),.UNSPECIFIED.,
 .F.,.F.,.F.)
B_SPLINE_SURFACE_WITH_KNOTS((6,1,1,1,1,1,1,1,1,1,1,1,1,1,1,1,1,1,1,1,1,
1,1,1,1,1,1,1,1,1,1,1,1,1,1,1,1,1,1,1,1,1,1,1,1,1,1,1,1,1,1,1,1,1,1,1,1,
1,1,1,1,1,1,1,1,6),(2,2),(-1.,-0.984615384615383,-0.969230769230768,-0.953846153846152,
-0.938461538461537,-0.923076923076922,-0.907692307692306,-0.892307692307691,
-0.876923076923076,-0.86153846153846,-0.846153846153845,-0.83076923076923,
-0.815384615384614,-0.799999999999999,-0.784615384615384,-0.769230769230768,
-0.753846153846153,-0.738461538461538,-0.723076923076922,-0.707692307692307,
-0.692307692307692,-0.676923076923076,-0.661538461538461,-0.646153846153846,
-0.63076923076923,-0.615384615384615,-0.6,-0.584615384615384,-0.569230769230769,
-0.553846153846154,-0.538461538461538,-0.523076923076923,-0.507692307692308,
-0.492307692307692,-0.476923076923077,-0.461538461538462,-0.446153846153846,
-0.430769230769231,-0.415384615384615,-0.4,-0.384615384615385,-0.369230769230769,
-0.353846153846154,-0.338461538461538,-0.323076923076923,-0.307692307692308,
-0.292307692307692,-0.276923076923077,-0.261538461538462,-0.246153846153846,
-0.230769230769231,-0.215384615384615,-0.2,-0.184615384615385,-0.169230769230769,
-0.153846153846154,-0.138461538461538,-0.123076923076923,-0.107692307692308,
-0.0923076923076923,-0.0769230769230769,-0.0615384615384615,-0.0461538461538462,
-0.0307692307692308,-0.0153846153846154,0.),(-1.,1.),.UNSPECIFIED.)
GEOMETRIC_REPRESENTATION_ITEM()
RATIONAL_B_SPLINE_SURFACE(((1.,1.),(1.,1.),(1.,1.),(1.,1.),(1.,1.),(1.,
1.),(1.,1.),(1.,1.),(1.,1.),(1.,1.),(1.,1.),(1.,1.),(1.,1.),(1.,1.),(1.,
1.),(1.,1.),(1.,1.),(1.,1.),(1.,1.),(1.,1.),(1.,1.),(1.,1.),(1.,1.),(1.,
1.),(1.,1.),(1.,1.),(1.,1.),(1.,1.),(1.,1.),(1.,1.),(1.,1.),(1.,1.),(1.,
1.),(1.,1.),(1.,1.),(1.,1.),(1.,1.),(1.,1.),(1.,1.),(1.,1.),(1.,1.),(1.,
1.),(1.,1.),(1.,1.),(1.,1.),(1.,1.),(1.,1.),(1.,1.),(1.,1.),(1.,1.),(1.,
1.),(1.,1.),(1.,1.),(1.,1.),(1.,1.),(1.,1.),(1.,1.),(1.,1.),(1.,1.),(1.,
1.),(1.,1.),(1.,1.),(1.,1.),(1.,1.),(1.,1.),(1.,1.),(1.,1.),(1.,1.),(1.,
1.),(1.,1.)))
REPRESENTATION_ITEM('')
SURFACE()
);
#116=(
BOUNDED_SURFACE()
B_SPLINE_SURFACE(5,1,((#54324,#54325),(#54326,#54327),(#54328,#54329),(#54330,
#54331),(#54332,#54333),(#54334,#54335),(#54336,#54337),(#54338,#54339),
(#54340,#54341),(#54342,#54343),(#54344,#54345),(#54346,#54347),(#54348,
#54349),(#54350,#54351),(#54352,#54353),(#54354,#54355),(#54356,#54357),
(#54358,#54359),(#54360,#54361),(#54362,#54363),(#54364,#54365),(#54366,
#54367),(#54368,#54369),(#54370,#54371),(#54372,#54373),(#54374,#54375),
(#54376,#54377),(#54378,#54379),(#54380,#54381),(#54382,#54383),(#54384,
#54385),(#54386,#54387),(#54388,#54389),(#54390,#54391),(#54392,#54393),
(#54394,#54395),(#54396,#54397),(#54398,#54399),(#54400,#54401),(#54402,
#54403),(#54404,#54405),(#54406,#54407),(#54408,#54409),(#54410,#54411),
(#54412,#54413),(#54414,#54415),(#54416,#54417),(#54418,#54419),(#54420,
#54421),(#54422,#54423),(#54424,#54425),(#54426,#54427),(#54428,#54429),
(#54430,#54431),(#54432,#54433),(#54434,#54435),(#54436,#54437),(#54438,
#54439),(#54440,#54441),(#54442,#54443),(#54444,#54445),(#54446,#54447),
(#54448,#54449),(#54450,#54451),(#54452,#54453),(#54454,#54455),(#54456,
#54457),(#54458,#54459),(#54460,#54461),(#54462,#54463)),.UNSPECIFIED.,
 .F.,.F.,.F.)
B_SPLINE_SURFACE_WITH_KNOTS((6,1,1,1,1,1,1,1,1,1,1,1,1,1,1,1,1,1,1,1,1,
1,1,1,1,1,1,1,1,1,1,1,1,1,1,1,1,1,1,1,1,1,1,1,1,1,1,1,1,1,1,1,1,1,1,1,1,
1,1,1,1,1,1,1,1,6),(2,2),(-1.,-0.984615384615383,-0.969230769230768,-0.953846153846152,
-0.938461538461537,-0.923076923076922,-0.907692307692306,-0.892307692307691,
-0.876923076923076,-0.86153846153846,-0.846153846153845,-0.83076923076923,
-0.815384615384614,-0.799999999999999,-0.784615384615384,-0.769230769230768,
-0.753846153846153,-0.738461538461538,-0.723076923076922,-0.707692307692307,
-0.692307692307692,-0.676923076923076,-0.661538461538461,-0.646153846153846,
-0.63076923076923,-0.615384615384615,-0.6,-0.584615384615384,-0.569230769230769,
-0.553846153846154,-0.538461538461538,-0.523076923076923,-0.507692307692308,
-0.492307692307692,-0.476923076923077,-0.461538461538462,-0.446153846153846,
-0.430769230769231,-0.415384615384615,-0.4,-0.384615384615385,-0.369230769230769,
-0.353846153846154,-0.338461538461538,-0.323076923076923,-0.307692307692308,
-0.292307692307692,-0.276923076923077,-0.261538461538462,-0.246153846153846,
-0.230769230769231,-0.215384615384615,-0.2,-0.184615384615385,-0.169230769230769,
-0.153846153846154,-0.138461538461538,-0.123076923076923,-0.107692307692308,
-0.0923076923076923,-0.0769230769230769,-0.0615384615384615,-0.0461538461538462,
-0.0307692307692308,-0.0153846153846154,0.),(-1.,1.),.UNSPECIFIED.)
GEOMETRIC_REPRESENTATION_ITEM()
RATIONAL_B_SPLINE_SURFACE(((1.,1.),(1.,1.),(1.,1.),(1.,1.),(1.,1.),(1.,
1.),(1.,1.),(1.,1.),(1.,1.),(1.,1.),(1.,1.),(1.,1.),(1.,1.),(1.,1.),(1.,
1.),(1.,1.),(1.,1.),(1.,1.),(1.,1.),(1.,1.),(1.,1.),(1.,1.),(1.,1.),(1.,
1.),(1.,1.),(1.,1.),(1.,1.),(1.,1.),(1.,1.),(1.,1.),(1.,1.),(1.,1.),(1.,
1.),(1.,1.),(1.,1.),(1.,1.),(1.,1.),(1.,1.),(1.,1.),(1.,1.),(1.,1.),(1.,
1.),(1.,1.),(1.,1.),(1.,1.),(1.,1.),(1.,1.),(1.,1.),(1.,1.),(1.,1.),(1.,
1.),(1.,1.),(1.,1.),(1.,1.),(1.,1.),(1.,1.),(1.,1.),(1.,1.),(1.,1.),(1.,
1.),(1.,1.),(1.,1.),(1.,1.),(1.,1.),(1.,1.),(1.,1.),(1.,1.),(1.,1.),(1.,
1.),(1.,1.)))
REPRESENTATION_ITEM('')
SURFACE()
);
#117=(
BOUNDED_SURFACE()
B_SPLINE_SURFACE(5,1,((#54554,#54555),(#54556,#54557),(#54558,#54559),(#54560,
#54561),(#54562,#54563),(#54564,#54565),(#54566,#54567),(#54568,#54569),
(#54570,#54571),(#54572,#54573),(#54574,#54575),(#54576,#54577),(#54578,
#54579),(#54580,#54581),(#54582,#54583),(#54584,#54585),(#54586,#54587),
(#54588,#54589),(#54590,#54591),(#54592,#54593),(#54594,#54595),(#54596,
#54597),(#54598,#54599),(#54600,#54601),(#54602,#54603),(#54604,#54605),
(#54606,#54607),(#54608,#54609),(#54610,#54611),(#54612,#54613),(#54614,
#54615),(#54616,#54617),(#54618,#54619),(#54620,#54621),(#54622,#54623),
(#54624,#54625),(#54626,#54627),(#54628,#54629),(#54630,#54631),(#54632,
#54633),(#54634,#54635),(#54636,#54637),(#54638,#54639),(#54640,#54641),
(#54642,#54643),(#54644,#54645),(#54646,#54647),(#54648,#54649),(#54650,
#54651),(#54652,#54653),(#54654,#54655),(#54656,#54657),(#54658,#54659),
(#54660,#54661),(#54662,#54663),(#54664,#54665),(#54666,#54667),(#54668,
#54669),(#54670,#54671),(#54672,#54673),(#54674,#54675),(#54676,#54677),
(#54678,#54679),(#54680,#54681),(#54682,#54683),(#54684,#54685),(#54686,
#54687),(#54688,#54689),(#54690,#54691),(#54692,#54693)),.UNSPECIFIED.,
 .F.,.F.,.F.)
B_SPLINE_SURFACE_WITH_KNOTS((6,1,1,1,1,1,1,1,1,1,1,1,1,1,1,1,1,1,1,1,1,
1,1,1,1,1,1,1,1,1,1,1,1,1,1,1,1,1,1,1,1,1,1,1,1,1,1,1,1,1,1,1,1,1,1,1,1,
1,1,1,1,1,1,1,1,6),(2,2),(-1.,-0.984615384615383,-0.969230769230768,-0.953846153846152,
-0.938461538461537,-0.923076923076922,-0.907692307692306,-0.892307692307691,
-0.876923076923076,-0.86153846153846,-0.846153846153845,-0.83076923076923,
-0.815384615384614,-0.799999999999999,-0.784615384615384,-0.769230769230768,
-0.753846153846153,-0.738461538461538,-0.723076923076922,-0.707692307692307,
-0.692307692307692,-0.676923076923076,-0.661538461538461,-0.646153846153846,
-0.63076923076923,-0.615384615384615,-0.6,-0.584615384615384,-0.569230769230769,
-0.553846153846154,-0.538461538461538,-0.523076923076923,-0.507692307692308,
-0.492307692307692,-0.476923076923077,-0.461538461538462,-0.446153846153846,
-0.430769230769231,-0.415384615384615,-0.4,-0.384615384615385,-0.369230769230769,
-0.353846153846154,-0.338461538461538,-0.323076923076923,-0.307692307692308,
-0.292307692307692,-0.276923076923077,-0.261538461538462,-0.246153846153846,
-0.230769230769231,-0.215384615384615,-0.2,-0.184615384615385,-0.169230769230769,
-0.153846153846154,-0.138461538461538,-0.123076923076923,-0.107692307692308,
-0.0923076923076923,-0.0769230769230769,-0.0615384615384615,-0.0461538461538462,
-0.0307692307692308,-0.0153846153846154,0.),(-1.,1.),.UNSPECIFIED.)
GEOMETRIC_REPRESENTATION_ITEM()
RATIONAL_B_SPLINE_SURFACE(((1.,1.),(1.,1.),(1.,1.),(1.,1.),(1.,1.),(1.,
1.),(1.,1.),(1.,1.),(1.,1.),(1.,1.),(1.,1.),(1.,1.),(1.,1.),(1.,1.),(1.,
1.),(1.,1.),(1.,1.),(1.,1.),(1.,1.),(1.,1.),(1.,1.),(1.,1.),(1.,1.),(1.,
1.),(1.,1.),(1.,1.),(1.,1.),(1.,1.),(1.,1.),(1.,1.),(1.,1.),(1.,1.),(1.,
1.),(1.,1.),(1.,1.),(1.,1.),(1.,1.),(1.,1.),(1.,1.),(1.,1.),(1.,1.),(1.,
1.),(1.,1.),(1.,1.),(1.,1.),(1.,1.),(1.,1.),(1.,1.),(1.,1.),(1.,1.),(1.,
1.),(1.,1.),(1.,1.),(1.,1.),(1.,1.),(1.,1.),(1.,1.),(1.,1.),(1.,1.),(1.,
1.),(1.,1.),(1.,1.),(1.,1.),(1.,1.),(1.,1.),(1.,1.),(1.,1.),(1.,1.),(1.,
1.),(1.,1.)))
REPRESENTATION_ITEM('')
SURFACE()
);
#118=(
BOUNDED_SURFACE()
B_SPLINE_SURFACE(5,1,((#54766,#54767),(#54768,#54769),(#54770,#54771),(#54772,
#54773),(#54774,#54775),(#54776,#54777),(#54778,#54779),(#54780,#54781),
(#54782,#54783),(#54784,#54785),(#54786,#54787),(#54788,#54789),(#54790,
#54791),(#54792,#54793),(#54794,#54795),(#54796,#54797),(#54798,#54799),
(#54800,#54801),(#54802,#54803),(#54804,#54805),(#54806,#54807),(#54808,
#54809),(#54810,#54811),(#54812,#54813),(#54814,#54815),(#54816,#54817),
(#54818,#54819),(#54820,#54821),(#54822,#54823),(#54824,#54825),(#54826,
#54827),(#54828,#54829),(#54830,#54831),(#54832,#54833),(#54834,#54835),
(#54836,#54837),(#54838,#54839),(#54840,#54841),(#54842,#54843),(#54844,
#54845),(#54846,#54847),(#54848,#54849),(#54850,#54851),(#54852,#54853),
(#54854,#54855),(#54856,#54857),(#54858,#54859),(#54860,#54861),(#54862,
#54863),(#54864,#54865),(#54866,#54867),(#54868,#54869),(#54870,#54871),
(#54872,#54873),(#54874,#54875),(#54876,#54877),(#54878,#54879),(#54880,
#54881),(#54882,#54883),(#54884,#54885),(#54886,#54887),(#54888,#54889),
(#54890,#54891),(#54892,#54893),(#54894,#54895),(#54896,#54897),(#54898,
#54899),(#54900,#54901),(#54902,#54903),(#54904,#54905)),.UNSPECIFIED.,
 .F.,.F.,.F.)
B_SPLINE_SURFACE_WITH_KNOTS((6,1,1,1,1,1,1,1,1,1,1,1,1,1,1,1,1,1,1,1,1,
1,1,1,1,1,1,1,1,1,1,1,1,1,1,1,1,1,1,1,1,1,1,1,1,1,1,1,1,1,1,1,1,1,1,1,1,
1,1,1,1,1,1,1,1,6),(2,2),(-1.,-0.984615384615383,-0.969230769230768,-0.953846153846152,
-0.938461538461537,-0.923076923076922,-0.907692307692306,-0.892307692307691,
-0.876923076923076,-0.86153846153846,-0.846153846153845,-0.83076923076923,
-0.815384615384614,-0.799999999999999,-0.784615384615384,-0.769230769230768,
-0.753846153846153,-0.738461538461538,-0.723076923076922,-0.707692307692307,
-0.692307692307692,-0.676923076923076,-0.661538461538461,-0.646153846153846,
-0.63076923076923,-0.615384615384615,-0.6,-0.584615384615384,-0.569230769230769,
-0.553846153846154,-0.538461538461538,-0.523076923076923,-0.507692307692308,
-0.492307692307692,-0.476923076923077,-0.461538461538462,-0.446153846153846,
-0.430769230769231,-0.415384615384615,-0.4,-0.384615384615385,-0.369230769230769,
-0.353846153846154,-0.338461538461538,-0.323076923076923,-0.307692307692308,
-0.292307692307692,-0.276923076923077,-0.261538461538462,-0.246153846153846,
-0.230769230769231,-0.215384615384615,-0.2,-0.184615384615385,-0.169230769230769,
-0.153846153846154,-0.138461538461538,-0.123076923076923,-0.107692307692308,
-0.0923076923076923,-0.0769230769230769,-0.0615384615384615,-0.0461538461538462,
-0.0307692307692308,-0.0153846153846154,0.),(-1.,1.),.UNSPECIFIED.)
GEOMETRIC_REPRESENTATION_ITEM()
RATIONAL_B_SPLINE_SURFACE(((1.,1.),(1.,1.),(1.,1.),(1.,1.),(1.,1.),(1.,
1.),(1.,1.),(1.,1.),(1.,1.),(1.,1.),(1.,1.),(1.,1.),(1.,1.),(1.,1.),(1.,
1.),(1.,1.),(1.,1.),(1.,1.),(1.,1.),(1.,1.),(1.,1.),(1.,1.),(1.,1.),(1.,
1.),(1.,1.),(1.,1.),(1.,1.),(1.,1.),(1.,1.),(1.,1.),(1.,1.),(1.,1.),(1.,
1.),(1.,1.),(1.,1.),(1.,1.),(1.,1.),(1.,1.),(1.,1.),(1.,1.),(1.,1.),(1.,
1.),(1.,1.),(1.,1.),(1.,1.),(1.,1.),(1.,1.),(1.,1.),(1.,1.),(1.,1.),(1.,
1.),(1.,1.),(1.,1.),(1.,1.),(1.,1.),(1.,1.),(1.,1.),(1.,1.),(1.,1.),(1.,
1.),(1.,1.),(1.,1.),(1.,1.),(1.,1.),(1.,1.),(1.,1.),(1.,1.),(1.,1.),(1.,
1.),(1.,1.)))
REPRESENTATION_ITEM('')
SURFACE()
);
#119=(
BOUNDED_SURFACE()
B_SPLINE_SURFACE(5,1,((#54996,#54997),(#54998,#54999),(#55000,#55001),(#55002,
#55003),(#55004,#55005),(#55006,#55007),(#55008,#55009),(#55010,#55011),
(#55012,#55013),(#55014,#55015),(#55016,#55017),(#55018,#55019),(#55020,
#55021),(#55022,#55023),(#55024,#55025),(#55026,#55027),(#55028,#55029),
(#55030,#55031),(#55032,#55033),(#55034,#55035),(#55036,#55037),(#55038,
#55039),(#55040,#55041),(#55042,#55043),(#55044,#55045),(#55046,#55047),
(#55048,#55049),(#55050,#55051),(#55052,#55053),(#55054,#55055),(#55056,
#55057),(#55058,#55059),(#55060,#55061),(#55062,#55063),(#55064,#55065),
(#55066,#55067),(#55068,#55069),(#55070,#55071),(#55072,#55073),(#55074,
#55075),(#55076,#55077),(#55078,#55079),(#55080,#55081),(#55082,#55083),
(#55084,#55085),(#55086,#55087),(#55088,#55089),(#55090,#55091),(#55092,
#55093),(#55094,#55095),(#55096,#55097),(#55098,#55099),(#55100,#55101),
(#55102,#55103),(#55104,#55105),(#55106,#55107),(#55108,#55109),(#55110,
#55111),(#55112,#55113),(#55114,#55115),(#55116,#55117),(#55118,#55119),
(#55120,#55121),(#55122,#55123),(#55124,#55125),(#55126,#55127),(#55128,
#55129),(#55130,#55131),(#55132,#55133),(#55134,#55135)),.UNSPECIFIED.,
 .F.,.F.,.F.)
B_SPLINE_SURFACE_WITH_KNOTS((6,1,1,1,1,1,1,1,1,1,1,1,1,1,1,1,1,1,1,1,1,
1,1,1,1,1,1,1,1,1,1,1,1,1,1,1,1,1,1,1,1,1,1,1,1,1,1,1,1,1,1,1,1,1,1,1,1,
1,1,1,1,1,1,1,1,6),(2,2),(-1.,-0.984615384615383,-0.969230769230768,-0.953846153846152,
-0.938461538461537,-0.923076923076922,-0.907692307692306,-0.892307692307691,
-0.876923076923076,-0.86153846153846,-0.846153846153845,-0.83076923076923,
-0.815384615384614,-0.799999999999999,-0.784615384615384,-0.769230769230768,
-0.753846153846153,-0.738461538461538,-0.723076923076922,-0.707692307692307,
-0.692307692307692,-0.676923076923076,-0.661538461538461,-0.646153846153846,
-0.63076923076923,-0.615384615384615,-0.6,-0.584615384615384,-0.569230769230769,
-0.553846153846154,-0.538461538461538,-0.523076923076923,-0.507692307692308,
-0.492307692307692,-0.476923076923077,-0.461538461538462,-0.446153846153846,
-0.430769230769231,-0.415384615384615,-0.4,-0.384615384615385,-0.369230769230769,
-0.353846153846154,-0.338461538461538,-0.323076923076923,-0.307692307692308,
-0.292307692307692,-0.276923076923077,-0.261538461538462,-0.246153846153846,
-0.230769230769231,-0.215384615384615,-0.2,-0.184615384615385,-0.169230769230769,
-0.153846153846154,-0.138461538461538,-0.123076923076923,-0.107692307692308,
-0.0923076923076923,-0.0769230769230769,-0.0615384615384615,-0.0461538461538462,
-0.0307692307692308,-0.0153846153846154,0.),(-1.,1.),.UNSPECIFIED.)
GEOMETRIC_REPRESENTATION_ITEM()
RATIONAL_B_SPLINE_SURFACE(((1.,1.),(1.,1.),(1.,1.),(1.,1.),(1.,1.),(1.,
1.),(1.,1.),(1.,1.),(1.,1.),(1.,1.),(1.,1.),(1.,1.),(1.,1.),(1.,1.),(1.,
1.),(1.,1.),(1.,1.),(1.,1.),(1.,1.),(1.,1.),(1.,1.),(1.,1.),(1.,1.),(1.,
1.),(1.,1.),(1.,1.),(1.,1.),(1.,1.),(1.,1.),(1.,1.),(1.,1.),(1.,1.),(1.,
1.),(1.,1.),(1.,1.),(1.,1.),(1.,1.),(1.,1.),(1.,1.),(1.,1.),(1.,1.),(1.,
1.),(1.,1.),(1.,1.),(1.,1.),(1.,1.),(1.,1.),(1.,1.),(1.,1.),(1.,1.),(1.,
1.),(1.,1.),(1.,1.),(1.,1.),(1.,1.),(1.,1.),(1.,1.),(1.,1.),(1.,1.),(1.,
1.),(1.,1.),(1.,1.),(1.,1.),(1.,1.),(1.,1.),(1.,1.),(1.,1.),(1.,1.),(1.,
1.),(1.,1.)))
REPRESENTATION_ITEM('')
SURFACE()
);
#120=(
BOUNDED_SURFACE()
B_SPLINE_SURFACE(5,1,((#55208,#55209),(#55210,#55211),(#55212,#55213),(#55214,
#55215),(#55216,#55217),(#55218,#55219),(#55220,#55221),(#55222,#55223),
(#55224,#55225),(#55226,#55227),(#55228,#55229),(#55230,#55231),(#55232,
#55233),(#55234,#55235),(#55236,#55237),(#55238,#55239),(#55240,#55241),
(#55242,#55243),(#55244,#55245),(#55246,#55247),(#55248,#55249),(#55250,
#55251),(#55252,#55253),(#55254,#55255),(#55256,#55257),(#55258,#55259),
(#55260,#55261),(#55262,#55263),(#55264,#55265),(#55266,#55267),(#55268,
#55269),(#55270,#55271),(#55272,#55273),(#55274,#55275),(#55276,#55277),
(#55278,#55279),(#55280,#55281),(#55282,#55283),(#55284,#55285),(#55286,
#55287),(#55288,#55289),(#55290,#55291),(#55292,#55293),(#55294,#55295),
(#55296,#55297),(#55298,#55299),(#55300,#55301),(#55302,#55303),(#55304,
#55305),(#55306,#55307),(#55308,#55309),(#55310,#55311),(#55312,#55313),
(#55314,#55315),(#55316,#55317),(#55318,#55319),(#55320,#55321),(#55322,
#55323),(#55324,#55325),(#55326,#55327),(#55328,#55329),(#55330,#55331),
(#55332,#55333),(#55334,#55335),(#55336,#55337),(#55338,#55339),(#55340,
#55341),(#55342,#55343),(#55344,#55345),(#55346,#55347)),.UNSPECIFIED.,
 .F.,.F.,.F.)
B_SPLINE_SURFACE_WITH_KNOTS((6,1,1,1,1,1,1,1,1,1,1,1,1,1,1,1,1,1,1,1,1,
1,1,1,1,1,1,1,1,1,1,1,1,1,1,1,1,1,1,1,1,1,1,1,1,1,1,1,1,1,1,1,1,1,1,1,1,
1,1,1,1,1,1,1,1,6),(2,2),(-1.,-0.984615384615383,-0.969230769230768,-0.953846153846152,
-0.938461538461537,-0.923076923076922,-0.907692307692306,-0.892307692307691,
-0.876923076923076,-0.86153846153846,-0.846153846153845,-0.83076923076923,
-0.815384615384614,-0.799999999999999,-0.784615384615384,-0.769230769230768,
-0.753846153846153,-0.738461538461538,-0.723076923076922,-0.707692307692307,
-0.692307692307692,-0.676923076923076,-0.661538461538461,-0.646153846153846,
-0.63076923076923,-0.615384615384615,-0.6,-0.584615384615384,-0.569230769230769,
-0.553846153846154,-0.538461538461538,-0.523076923076923,-0.507692307692308,
-0.492307692307692,-0.476923076923077,-0.461538461538462,-0.446153846153846,
-0.430769230769231,-0.415384615384615,-0.4,-0.384615384615385,-0.369230769230769,
-0.353846153846154,-0.338461538461538,-0.323076923076923,-0.307692307692308,
-0.292307692307692,-0.276923076923077,-0.261538461538462,-0.246153846153846,
-0.230769230769231,-0.215384615384615,-0.2,-0.184615384615385,-0.169230769230769,
-0.153846153846154,-0.138461538461538,-0.123076923076923,-0.107692307692308,
-0.0923076923076923,-0.0769230769230769,-0.0615384615384615,-0.0461538461538462,
-0.0307692307692308,-0.0153846153846154,0.),(-1.,1.),.UNSPECIFIED.)
GEOMETRIC_REPRESENTATION_ITEM()
RATIONAL_B_SPLINE_SURFACE(((1.,1.),(1.,1.),(1.,1.),(1.,1.),(1.,1.),(1.,
1.),(1.,1.),(1.,1.),(1.,1.),(1.,1.),(1.,1.),(1.,1.),(1.,1.),(1.,1.),(1.,
1.),(1.,1.),(1.,1.),(1.,1.),(1.,1.),(1.,1.),(1.,1.),(1.,1.),(1.,1.),(1.,
1.),(1.,1.),(1.,1.),(1.,1.),(1.,1.),(1.,1.),(1.,1.),(1.,1.),(1.,1.),(1.,
1.),(1.,1.),(1.,1.),(1.,1.),(1.,1.),(1.,1.),(1.,1.),(1.,1.),(1.,1.),(1.,
1.),(1.,1.),(1.,1.),(1.,1.),(1.,1.),(1.,1.),(1.,1.),(1.,1.),(1.,1.),(1.,
1.),(1.,1.),(1.,1.),(1.,1.),(1.,1.),(1.,1.),(1.,1.),(1.,1.),(1.,1.),(1.,
1.),(1.,1.),(1.,1.),(1.,1.),(1.,1.),(1.,1.),(1.,1.),(1.,1.),(1.,1.),(1.,
1.),(1.,1.)))
REPRESENTATION_ITEM('')
SURFACE()
);
#121=(
BOUNDED_SURFACE()
B_SPLINE_SURFACE(5,1,((#55438,#55439),(#55440,#55441),(#55442,#55443),(#55444,
#55445),(#55446,#55447),(#55448,#55449),(#55450,#55451),(#55452,#55453),
(#55454,#55455),(#55456,#55457),(#55458,#55459),(#55460,#55461),(#55462,
#55463),(#55464,#55465),(#55466,#55467),(#55468,#55469),(#55470,#55471),
(#55472,#55473),(#55474,#55475),(#55476,#55477),(#55478,#55479),(#55480,
#55481),(#55482,#55483),(#55484,#55485),(#55486,#55487),(#55488,#55489),
(#55490,#55491),(#55492,#55493),(#55494,#55495),(#55496,#55497),(#55498,
#55499),(#55500,#55501),(#55502,#55503),(#55504,#55505),(#55506,#55507),
(#55508,#55509),(#55510,#55511),(#55512,#55513),(#55514,#55515),(#55516,
#55517),(#55518,#55519),(#55520,#55521),(#55522,#55523),(#55524,#55525),
(#55526,#55527),(#55528,#55529),(#55530,#55531),(#55532,#55533),(#55534,
#55535),(#55536,#55537),(#55538,#55539),(#55540,#55541),(#55542,#55543),
(#55544,#55545),(#55546,#55547),(#55548,#55549),(#55550,#55551),(#55552,
#55553),(#55554,#55555),(#55556,#55557),(#55558,#55559),(#55560,#55561),
(#55562,#55563),(#55564,#55565),(#55566,#55567),(#55568,#55569),(#55570,
#55571),(#55572,#55573),(#55574,#55575),(#55576,#55577)),.UNSPECIFIED.,
 .F.,.F.,.F.)
B_SPLINE_SURFACE_WITH_KNOTS((6,1,1,1,1,1,1,1,1,1,1,1,1,1,1,1,1,1,1,1,1,
1,1,1,1,1,1,1,1,1,1,1,1,1,1,1,1,1,1,1,1,1,1,1,1,1,1,1,1,1,1,1,1,1,1,1,1,
1,1,1,1,1,1,1,1,6),(2,2),(-1.,-0.984615384615383,-0.969230769230768,-0.953846153846152,
-0.938461538461537,-0.923076923076922,-0.907692307692306,-0.892307692307691,
-0.876923076923076,-0.86153846153846,-0.846153846153845,-0.83076923076923,
-0.815384615384614,-0.799999999999999,-0.784615384615384,-0.769230769230768,
-0.753846153846153,-0.738461538461538,-0.723076923076922,-0.707692307692307,
-0.692307692307692,-0.676923076923076,-0.661538461538461,-0.646153846153846,
-0.63076923076923,-0.615384615384615,-0.6,-0.584615384615384,-0.569230769230769,
-0.553846153846154,-0.538461538461538,-0.523076923076923,-0.507692307692308,
-0.492307692307692,-0.476923076923077,-0.461538461538462,-0.446153846153846,
-0.430769230769231,-0.415384615384615,-0.4,-0.384615384615385,-0.369230769230769,
-0.353846153846154,-0.338461538461538,-0.323076923076923,-0.307692307692308,
-0.292307692307692,-0.276923076923077,-0.261538461538462,-0.246153846153846,
-0.230769230769231,-0.215384615384615,-0.2,-0.184615384615385,-0.169230769230769,
-0.153846153846154,-0.138461538461538,-0.123076923076923,-0.107692307692308,
-0.0923076923076923,-0.0769230769230769,-0.0615384615384615,-0.0461538461538462,
-0.0307692307692308,-0.0153846153846154,0.),(-1.,1.),.UNSPECIFIED.)
GEOMETRIC_REPRESENTATION_ITEM()
RATIONAL_B_SPLINE_SURFACE(((1.,1.),(1.,1.),(1.,1.),(1.,1.),(1.,1.),(1.,
1.),(1.,1.),(1.,1.),(1.,1.),(1.,1.),(1.,1.),(1.,1.),(1.,1.),(1.,1.),(1.,
1.),(1.,1.),(1.,1.),(1.,1.),(1.,1.),(1.,1.),(1.,1.),(1.,1.),(1.,1.),(1.,
1.),(1.,1.),(1.,1.),(1.,1.),(1.,1.),(1.,1.),(1.,1.),(1.,1.),(1.,1.),(1.,
1.),(1.,1.),(1.,1.),(1.,1.),(1.,1.),(1.,1.),(1.,1.),(1.,1.),(1.,1.),(1.,
1.),(1.,1.),(1.,1.),(1.,1.),(1.,1.),(1.,1.),(1.,1.),(1.,1.),(1.,1.),(1.,
1.),(1.,1.),(1.,1.),(1.,1.),(1.,1.),(1.,1.),(1.,1.),(1.,1.),(1.,1.),(1.,
1.),(1.,1.),(1.,1.),(1.,1.),(1.,1.),(1.,1.),(1.,1.),(1.,1.),(1.,1.),(1.,
1.),(1.,1.)))
REPRESENTATION_ITEM('')
SURFACE()
);
#122=(
BOUNDED_SURFACE()
B_SPLINE_SURFACE(5,1,((#55650,#55651),(#55652,#55653),(#55654,#55655),(#55656,
#55657),(#55658,#55659),(#55660,#55661),(#55662,#55663),(#55664,#55665),
(#55666,#55667),(#55668,#55669),(#55670,#55671),(#55672,#55673),(#55674,
#55675),(#55676,#55677),(#55678,#55679),(#55680,#55681),(#55682,#55683),
(#55684,#55685),(#55686,#55687),(#55688,#55689),(#55690,#55691),(#55692,
#55693),(#55694,#55695),(#55696,#55697),(#55698,#55699),(#55700,#55701),
(#55702,#55703),(#55704,#55705),(#55706,#55707),(#55708,#55709),(#55710,
#55711),(#55712,#55713),(#55714,#55715),(#55716,#55717),(#55718,#55719),
(#55720,#55721),(#55722,#55723),(#55724,#55725),(#55726,#55727),(#55728,
#55729),(#55730,#55731),(#55732,#55733),(#55734,#55735),(#55736,#55737),
(#55738,#55739),(#55740,#55741),(#55742,#55743),(#55744,#55745),(#55746,
#55747),(#55748,#55749),(#55750,#55751),(#55752,#55753),(#55754,#55755),
(#55756,#55757),(#55758,#55759),(#55760,#55761),(#55762,#55763),(#55764,
#55765),(#55766,#55767),(#55768,#55769),(#55770,#55771),(#55772,#55773),
(#55774,#55775),(#55776,#55777),(#55778,#55779),(#55780,#55781),(#55782,
#55783),(#55784,#55785),(#55786,#55787),(#55788,#55789)),.UNSPECIFIED.,
 .F.,.F.,.F.)
B_SPLINE_SURFACE_WITH_KNOTS((6,1,1,1,1,1,1,1,1,1,1,1,1,1,1,1,1,1,1,1,1,
1,1,1,1,1,1,1,1,1,1,1,1,1,1,1,1,1,1,1,1,1,1,1,1,1,1,1,1,1,1,1,1,1,1,1,1,
1,1,1,1,1,1,1,1,6),(2,2),(-1.,-0.984615384615383,-0.969230769230768,-0.953846153846152,
-0.938461538461537,-0.923076923076922,-0.907692307692306,-0.892307692307691,
-0.876923076923076,-0.86153846153846,-0.846153846153845,-0.83076923076923,
-0.815384615384614,-0.799999999999999,-0.784615384615384,-0.769230769230768,
-0.753846153846153,-0.738461538461538,-0.723076923076922,-0.707692307692307,
-0.692307692307692,-0.676923076923076,-0.661538461538461,-0.646153846153846,
-0.63076923076923,-0.615384615384615,-0.6,-0.584615384615384,-0.569230769230769,
-0.553846153846154,-0.538461538461538,-0.523076923076923,-0.507692307692308,
-0.492307692307692,-0.476923076923077,-0.461538461538462,-0.446153846153846,
-0.430769230769231,-0.415384615384615,-0.4,-0.384615384615385,-0.369230769230769,
-0.353846153846154,-0.338461538461538,-0.323076923076923,-0.307692307692308,
-0.292307692307692,-0.276923076923077,-0.261538461538462,-0.246153846153846,
-0.230769230769231,-0.215384615384615,-0.2,-0.184615384615385,-0.169230769230769,
-0.153846153846154,-0.138461538461538,-0.123076923076923,-0.107692307692308,
-0.0923076923076923,-0.0769230769230769,-0.0615384615384615,-0.0461538461538462,
-0.0307692307692308,-0.0153846153846154,0.),(-1.,1.),.UNSPECIFIED.)
GEOMETRIC_REPRESENTATION_ITEM()
RATIONAL_B_SPLINE_SURFACE(((1.,1.),(1.,1.),(1.,1.),(1.,1.),(1.,1.),(1.,
1.),(1.,1.),(1.,1.),(1.,1.),(1.,1.),(1.,1.),(1.,1.),(1.,1.),(1.,1.),(1.,
1.),(1.,1.),(1.,1.),(1.,1.),(1.,1.),(1.,1.),(1.,1.),(1.,1.),(1.,1.),(1.,
1.),(1.,1.),(1.,1.),(1.,1.),(1.,1.),(1.,1.),(1.,1.),(1.,1.),(1.,1.),(1.,
1.),(1.,1.),(1.,1.),(1.,1.),(1.,1.),(1.,1.),(1.,1.),(1.,1.),(1.,1.),(1.,
1.),(1.,1.),(1.,1.),(1.,1.),(1.,1.),(1.,1.),(1.,1.),(1.,1.),(1.,1.),(1.,
1.),(1.,1.),(1.,1.),(1.,1.),(1.,1.),(1.,1.),(1.,1.),(1.,1.),(1.,1.),(1.,
1.),(1.,1.),(1.,1.),(1.,1.),(1.,1.),(1.,1.),(1.,1.),(1.,1.),(1.,1.),(1.,
1.),(1.,1.)))
REPRESENTATION_ITEM('')
SURFACE()
);
#123=(
BOUNDED_SURFACE()
B_SPLINE_SURFACE(5,1,((#55880,#55881),(#55882,#55883),(#55884,#55885),(#55886,
#55887),(#55888,#55889),(#55890,#55891),(#55892,#55893),(#55894,#55895),
(#55896,#55897),(#55898,#55899),(#55900,#55901),(#55902,#55903),(#55904,
#55905),(#55906,#55907),(#55908,#55909),(#55910,#55911),(#55912,#55913),
(#55914,#55915),(#55916,#55917),(#55918,#55919),(#55920,#55921),(#55922,
#55923),(#55924,#55925),(#55926,#55927),(#55928,#55929),(#55930,#55931),
(#55932,#55933),(#55934,#55935),(#55936,#55937),(#55938,#55939),(#55940,
#55941),(#55942,#55943),(#55944,#55945),(#55946,#55947),(#55948,#55949),
(#55950,#55951),(#55952,#55953),(#55954,#55955),(#55956,#55957),(#55958,
#55959),(#55960,#55961),(#55962,#55963),(#55964,#55965),(#55966,#55967),
(#55968,#55969),(#55970,#55971),(#55972,#55973),(#55974,#55975),(#55976,
#55977),(#55978,#55979),(#55980,#55981),(#55982,#55983),(#55984,#55985),
(#55986,#55987),(#55988,#55989),(#55990,#55991),(#55992,#55993),(#55994,
#55995),(#55996,#55997),(#55998,#55999),(#56000,#56001),(#56002,#56003),
(#56004,#56005),(#56006,#56007),(#56008,#56009),(#56010,#56011),(#56012,
#56013),(#56014,#56015),(#56016,#56017),(#56018,#56019)),.UNSPECIFIED.,
 .F.,.F.,.F.)
B_SPLINE_SURFACE_WITH_KNOTS((6,1,1,1,1,1,1,1,1,1,1,1,1,1,1,1,1,1,1,1,1,
1,1,1,1,1,1,1,1,1,1,1,1,1,1,1,1,1,1,1,1,1,1,1,1,1,1,1,1,1,1,1,1,1,1,1,1,
1,1,1,1,1,1,1,1,6),(2,2),(-1.,-0.984615384615383,-0.969230769230768,-0.953846153846152,
-0.938461538461537,-0.923076923076922,-0.907692307692306,-0.892307692307691,
-0.876923076923076,-0.86153846153846,-0.846153846153845,-0.83076923076923,
-0.815384615384614,-0.799999999999999,-0.784615384615384,-0.769230769230768,
-0.753846153846153,-0.738461538461538,-0.723076923076922,-0.707692307692307,
-0.692307692307692,-0.676923076923076,-0.661538461538461,-0.646153846153846,
-0.63076923076923,-0.615384615384615,-0.6,-0.584615384615384,-0.569230769230769,
-0.553846153846154,-0.538461538461538,-0.523076923076923,-0.507692307692308,
-0.492307692307692,-0.476923076923077,-0.461538461538462,-0.446153846153846,
-0.430769230769231,-0.415384615384615,-0.4,-0.384615384615385,-0.369230769230769,
-0.353846153846154,-0.338461538461538,-0.323076923076923,-0.307692307692308,
-0.292307692307692,-0.276923076923077,-0.261538461538462,-0.246153846153846,
-0.230769230769231,-0.215384615384615,-0.2,-0.184615384615385,-0.169230769230769,
-0.153846153846154,-0.138461538461538,-0.123076923076923,-0.107692307692308,
-0.0923076923076923,-0.0769230769230769,-0.0615384615384615,-0.0461538461538462,
-0.0307692307692308,-0.0153846153846154,0.),(-1.,1.),.UNSPECIFIED.)
GEOMETRIC_REPRESENTATION_ITEM()
RATIONAL_B_SPLINE_SURFACE(((1.,1.),(1.,1.),(1.,1.),(1.,1.),(1.,1.),(1.,
1.),(1.,1.),(1.,1.),(1.,1.),(1.,1.),(1.,1.),(1.,1.),(1.,1.),(1.,1.),(1.,
1.),(1.,1.),(1.,1.),(1.,1.),(1.,1.),(1.,1.),(1.,1.),(1.,1.),(1.,1.),(1.,
1.),(1.,1.),(1.,1.),(1.,1.),(1.,1.),(1.,1.),(1.,1.),(1.,1.),(1.,1.),(1.,
1.),(1.,1.),(1.,1.),(1.,1.),(1.,1.),(1.,1.),(1.,1.),(1.,1.),(1.,1.),(1.,
1.),(1.,1.),(1.,1.),(1.,1.),(1.,1.),(1.,1.),(1.,1.),(1.,1.),(1.,1.),(1.,
1.),(1.,1.),(1.,1.),(1.,1.),(1.,1.),(1.,1.),(1.,1.),(1.,1.),(1.,1.),(1.,
1.),(1.,1.),(1.,1.),(1.,1.),(1.,1.),(1.,1.),(1.,1.),(1.,1.),(1.,1.),(1.,
1.),(1.,1.)))
REPRESENTATION_ITEM('')
SURFACE()
);
#124=(
BOUNDED_SURFACE()
B_SPLINE_SURFACE(5,1,((#56092,#56093),(#56094,#56095),(#56096,#56097),(#56098,
#56099),(#56100,#56101),(#56102,#56103),(#56104,#56105),(#56106,#56107),
(#56108,#56109),(#56110,#56111),(#56112,#56113),(#56114,#56115),(#56116,
#56117),(#56118,#56119),(#56120,#56121),(#56122,#56123),(#56124,#56125),
(#56126,#56127),(#56128,#56129),(#56130,#56131),(#56132,#56133),(#56134,
#56135),(#56136,#56137),(#56138,#56139),(#56140,#56141),(#56142,#56143),
(#56144,#56145),(#56146,#56147),(#56148,#56149),(#56150,#56151),(#56152,
#56153),(#56154,#56155),(#56156,#56157),(#56158,#56159),(#56160,#56161),
(#56162,#56163),(#56164,#56165),(#56166,#56167),(#56168,#56169),(#56170,
#56171),(#56172,#56173),(#56174,#56175),(#56176,#56177),(#56178,#56179),
(#56180,#56181),(#56182,#56183),(#56184,#56185),(#56186,#56187),(#56188,
#56189),(#56190,#56191),(#56192,#56193),(#56194,#56195),(#56196,#56197),
(#56198,#56199),(#56200,#56201),(#56202,#56203),(#56204,#56205),(#56206,
#56207),(#56208,#56209),(#56210,#56211),(#56212,#56213),(#56214,#56215),
(#56216,#56217),(#56218,#56219),(#56220,#56221),(#56222,#56223),(#56224,
#56225),(#56226,#56227),(#56228,#56229),(#56230,#56231)),.UNSPECIFIED.,
 .F.,.F.,.F.)
B_SPLINE_SURFACE_WITH_KNOTS((6,1,1,1,1,1,1,1,1,1,1,1,1,1,1,1,1,1,1,1,1,
1,1,1,1,1,1,1,1,1,1,1,1,1,1,1,1,1,1,1,1,1,1,1,1,1,1,1,1,1,1,1,1,1,1,1,1,
1,1,1,1,1,1,1,1,6),(2,2),(-1.,-0.984615384615383,-0.969230769230768,-0.953846153846152,
-0.938461538461537,-0.923076923076922,-0.907692307692306,-0.892307692307691,
-0.876923076923076,-0.86153846153846,-0.846153846153845,-0.83076923076923,
-0.815384615384614,-0.799999999999999,-0.784615384615384,-0.769230769230768,
-0.753846153846153,-0.738461538461538,-0.723076923076922,-0.707692307692307,
-0.692307692307692,-0.676923076923076,-0.661538461538461,-0.646153846153846,
-0.63076923076923,-0.615384615384615,-0.6,-0.584615384615384,-0.569230769230769,
-0.553846153846154,-0.538461538461538,-0.523076923076923,-0.507692307692308,
-0.492307692307692,-0.476923076923077,-0.461538461538462,-0.446153846153846,
-0.430769230769231,-0.415384615384615,-0.4,-0.384615384615385,-0.369230769230769,
-0.353846153846154,-0.338461538461538,-0.323076923076923,-0.307692307692308,
-0.292307692307692,-0.276923076923077,-0.261538461538462,-0.246153846153846,
-0.230769230769231,-0.215384615384615,-0.2,-0.184615384615385,-0.169230769230769,
-0.153846153846154,-0.138461538461538,-0.123076923076923,-0.107692307692308,
-0.0923076923076923,-0.0769230769230769,-0.0615384615384615,-0.0461538461538462,
-0.0307692307692308,-0.0153846153846154,0.),(-1.,1.),.UNSPECIFIED.)
GEOMETRIC_REPRESENTATION_ITEM()
RATIONAL_B_SPLINE_SURFACE(((1.,1.),(1.,1.),(1.,1.),(1.,1.),(1.,1.),(1.,
1.),(1.,1.),(1.,1.),(1.,1.),(1.,1.),(1.,1.),(1.,1.),(1.,1.),(1.,1.),(1.,
1.),(1.,1.),(1.,1.),(1.,1.),(1.,1.),(1.,1.),(1.,1.),(1.,1.),(1.,1.),(1.,
1.),(1.,1.),(1.,1.),(1.,1.),(1.,1.),(1.,1.),(1.,1.),(1.,1.),(1.,1.),(1.,
1.),(1.,1.),(1.,1.),(1.,1.),(1.,1.),(1.,1.),(1.,1.),(1.,1.),(1.,1.),(1.,
1.),(1.,1.),(1.,1.),(1.,1.),(1.,1.),(1.,1.),(1.,1.),(1.,1.),(1.,1.),(1.,
1.),(1.,1.),(1.,1.),(1.,1.),(1.,1.),(1.,1.),(1.,1.),(1.,1.),(1.,1.),(1.,
1.),(1.,1.),(1.,1.),(1.,1.),(1.,1.),(1.,1.),(1.,1.),(1.,1.),(1.,1.),(1.,
1.),(1.,1.)))
REPRESENTATION_ITEM('')
SURFACE()
);
#125=(
BOUNDED_SURFACE()
B_SPLINE_SURFACE(5,1,((#56322,#56323),(#56324,#56325),(#56326,#56327),(#56328,
#56329),(#56330,#56331),(#56332,#56333),(#56334,#56335),(#56336,#56337),
(#56338,#56339),(#56340,#56341),(#56342,#56343),(#56344,#56345),(#56346,
#56347),(#56348,#56349),(#56350,#56351),(#56352,#56353),(#56354,#56355),
(#56356,#56357),(#56358,#56359),(#56360,#56361),(#56362,#56363),(#56364,
#56365),(#56366,#56367),(#56368,#56369),(#56370,#56371),(#56372,#56373),
(#56374,#56375),(#56376,#56377),(#56378,#56379),(#56380,#56381),(#56382,
#56383),(#56384,#56385),(#56386,#56387),(#56388,#56389),(#56390,#56391),
(#56392,#56393),(#56394,#56395),(#56396,#56397),(#56398,#56399),(#56400,
#56401),(#56402,#56403),(#56404,#56405),(#56406,#56407),(#56408,#56409),
(#56410,#56411),(#56412,#56413),(#56414,#56415),(#56416,#56417),(#56418,
#56419),(#56420,#56421),(#56422,#56423),(#56424,#56425),(#56426,#56427),
(#56428,#56429),(#56430,#56431),(#56432,#56433),(#56434,#56435),(#56436,
#56437),(#56438,#56439),(#56440,#56441),(#56442,#56443),(#56444,#56445),
(#56446,#56447),(#56448,#56449),(#56450,#56451),(#56452,#56453),(#56454,
#56455),(#56456,#56457),(#56458,#56459),(#56460,#56461)),.UNSPECIFIED.,
 .F.,.F.,.F.)
B_SPLINE_SURFACE_WITH_KNOTS((6,1,1,1,1,1,1,1,1,1,1,1,1,1,1,1,1,1,1,1,1,
1,1,1,1,1,1,1,1,1,1,1,1,1,1,1,1,1,1,1,1,1,1,1,1,1,1,1,1,1,1,1,1,1,1,1,1,
1,1,1,1,1,1,1,1,6),(2,2),(-1.,-0.984615384615383,-0.969230769230768,-0.953846153846152,
-0.938461538461537,-0.923076923076922,-0.907692307692306,-0.892307692307691,
-0.876923076923076,-0.86153846153846,-0.846153846153845,-0.83076923076923,
-0.815384615384614,-0.799999999999999,-0.784615384615384,-0.769230769230768,
-0.753846153846153,-0.738461538461538,-0.723076923076922,-0.707692307692307,
-0.692307692307692,-0.676923076923076,-0.661538461538461,-0.646153846153846,
-0.63076923076923,-0.615384615384615,-0.6,-0.584615384615384,-0.569230769230769,
-0.553846153846154,-0.538461538461538,-0.523076923076923,-0.507692307692308,
-0.492307692307692,-0.476923076923077,-0.461538461538462,-0.446153846153846,
-0.430769230769231,-0.415384615384615,-0.4,-0.384615384615385,-0.369230769230769,
-0.353846153846154,-0.338461538461538,-0.323076923076923,-0.307692307692308,
-0.292307692307692,-0.276923076923077,-0.261538461538462,-0.246153846153846,
-0.230769230769231,-0.215384615384615,-0.2,-0.184615384615385,-0.169230769230769,
-0.153846153846154,-0.138461538461538,-0.123076923076923,-0.107692307692308,
-0.0923076923076923,-0.0769230769230769,-0.0615384615384615,-0.0461538461538462,
-0.0307692307692308,-0.0153846153846154,0.),(-1.,1.),.UNSPECIFIED.)
GEOMETRIC_REPRESENTATION_ITEM()
RATIONAL_B_SPLINE_SURFACE(((1.,1.),(1.,1.),(1.,1.),(1.,1.),(1.,1.),(1.,
1.),(1.,1.),(1.,1.),(1.,1.),(1.,1.),(1.,1.),(1.,1.),(1.,1.),(1.,1.),(1.,
1.),(1.,1.),(1.,1.),(1.,1.),(1.,1.),(1.,1.),(1.,1.),(1.,1.),(1.,1.),(1.,
1.),(1.,1.),(1.,1.),(1.,1.),(1.,1.),(1.,1.),(1.,1.),(1.,1.),(1.,1.),(1.,
1.),(1.,1.),(1.,1.),(1.,1.),(1.,1.),(1.,1.),(1.,1.),(1.,1.),(1.,1.),(1.,
1.),(1.,1.),(1.,1.),(1.,1.),(1.,1.),(1.,1.),(1.,1.),(1.,1.),(1.,1.),(1.,
1.),(1.,1.),(1.,1.),(1.,1.),(1.,1.),(1.,1.),(1.,1.),(1.,1.),(1.,1.),(1.,
1.),(1.,1.),(1.,1.),(1.,1.),(1.,1.),(1.,1.),(1.,1.),(1.,1.),(1.,1.),(1.,
1.),(1.,1.)))
REPRESENTATION_ITEM('')
SURFACE()
);
#126=(
BOUNDED_SURFACE()
B_SPLINE_SURFACE(5,1,((#56534,#56535),(#56536,#56537),(#56538,#56539),(#56540,
#56541),(#56542,#56543),(#56544,#56545),(#56546,#56547),(#56548,#56549),
(#56550,#56551),(#56552,#56553),(#56554,#56555),(#56556,#56557),(#56558,
#56559),(#56560,#56561),(#56562,#56563),(#56564,#56565),(#56566,#56567),
(#56568,#56569),(#56570,#56571),(#56572,#56573),(#56574,#56575),(#56576,
#56577),(#56578,#56579),(#56580,#56581),(#56582,#56583),(#56584,#56585),
(#56586,#56587),(#56588,#56589),(#56590,#56591),(#56592,#56593),(#56594,
#56595),(#56596,#56597),(#56598,#56599),(#56600,#56601),(#56602,#56603),
(#56604,#56605),(#56606,#56607),(#56608,#56609),(#56610,#56611),(#56612,
#56613),(#56614,#56615),(#56616,#56617),(#56618,#56619),(#56620,#56621),
(#56622,#56623),(#56624,#56625),(#56626,#56627),(#56628,#56629),(#56630,
#56631),(#56632,#56633),(#56634,#56635),(#56636,#56637),(#56638,#56639),
(#56640,#56641),(#56642,#56643),(#56644,#56645),(#56646,#56647),(#56648,
#56649),(#56650,#56651),(#56652,#56653),(#56654,#56655),(#56656,#56657),
(#56658,#56659),(#56660,#56661),(#56662,#56663),(#56664,#56665),(#56666,
#56667),(#56668,#56669),(#56670,#56671),(#56672,#56673)),.UNSPECIFIED.,
 .F.,.F.,.F.)
B_SPLINE_SURFACE_WITH_KNOTS((6,1,1,1,1,1,1,1,1,1,1,1,1,1,1,1,1,1,1,1,1,
1,1,1,1,1,1,1,1,1,1,1,1,1,1,1,1,1,1,1,1,1,1,1,1,1,1,1,1,1,1,1,1,1,1,1,1,
1,1,1,1,1,1,1,1,6),(2,2),(-1.,-0.984615384615383,-0.969230769230768,-0.953846153846152,
-0.938461538461537,-0.923076923076922,-0.907692307692306,-0.892307692307691,
-0.876923076923076,-0.86153846153846,-0.846153846153845,-0.83076923076923,
-0.815384615384614,-0.799999999999999,-0.784615384615384,-0.769230769230768,
-0.753846153846153,-0.738461538461538,-0.723076923076922,-0.707692307692307,
-0.692307692307692,-0.676923076923076,-0.661538461538461,-0.646153846153846,
-0.63076923076923,-0.615384615384615,-0.6,-0.584615384615384,-0.569230769230769,
-0.553846153846154,-0.538461538461538,-0.523076923076923,-0.507692307692308,
-0.492307692307692,-0.476923076923077,-0.461538461538462,-0.446153846153846,
-0.430769230769231,-0.415384615384615,-0.4,-0.384615384615385,-0.369230769230769,
-0.353846153846154,-0.338461538461538,-0.323076923076923,-0.307692307692308,
-0.292307692307692,-0.276923076923077,-0.261538461538462,-0.246153846153846,
-0.230769230769231,-0.215384615384615,-0.2,-0.184615384615385,-0.169230769230769,
-0.153846153846154,-0.138461538461538,-0.123076923076923,-0.107692307692308,
-0.0923076923076923,-0.0769230769230769,-0.0615384615384615,-0.0461538461538462,
-0.0307692307692308,-0.0153846153846154,0.),(-1.,1.),.UNSPECIFIED.)
GEOMETRIC_REPRESENTATION_ITEM()
RATIONAL_B_SPLINE_SURFACE(((1.,1.),(1.,1.),(1.,1.),(1.,1.),(1.,1.),(1.,
1.),(1.,1.),(1.,1.),(1.,1.),(1.,1.),(1.,1.),(1.,1.),(1.,1.),(1.,1.),(1.,
1.),(1.,1.),(1.,1.),(1.,1.),(1.,1.),(1.,1.),(1.,1.),(1.,1.),(1.,1.),(1.,
1.),(1.,1.),(1.,1.),(1.,1.),(1.,1.),(1.,1.),(1.,1.),(1.,1.),(1.,1.),(1.,
1.),(1.,1.),(1.,1.),(1.,1.),(1.,1.),(1.,1.),(1.,1.),(1.,1.),(1.,1.),(1.,
1.),(1.,1.),(1.,1.),(1.,1.),(1.,1.),(1.,1.),(1.,1.),(1.,1.),(1.,1.),(1.,
1.),(1.,1.),(1.,1.),(1.,1.),(1.,1.),(1.,1.),(1.,1.),(1.,1.),(1.,1.),(1.,
1.),(1.,1.),(1.,1.),(1.,1.),(1.,1.),(1.,1.),(1.,1.),(1.,1.),(1.,1.),(1.,
1.),(1.,1.)))
REPRESENTATION_ITEM('')
SURFACE()
);
#127=(
BOUNDED_SURFACE()
B_SPLINE_SURFACE(5,1,((#56764,#56765),(#56766,#56767),(#56768,#56769),(#56770,
#56771),(#56772,#56773),(#56774,#56775),(#56776,#56777),(#56778,#56779),
(#56780,#56781),(#56782,#56783),(#56784,#56785),(#56786,#56787),(#56788,
#56789),(#56790,#56791),(#56792,#56793),(#56794,#56795),(#56796,#56797),
(#56798,#56799),(#56800,#56801),(#56802,#56803),(#56804,#56805),(#56806,
#56807),(#56808,#56809),(#56810,#56811),(#56812,#56813),(#56814,#56815),
(#56816,#56817),(#56818,#56819),(#56820,#56821),(#56822,#56823),(#56824,
#56825),(#56826,#56827),(#56828,#56829),(#56830,#56831),(#56832,#56833),
(#56834,#56835),(#56836,#56837),(#56838,#56839),(#56840,#56841),(#56842,
#56843),(#56844,#56845),(#56846,#56847),(#56848,#56849),(#56850,#56851),
(#56852,#56853),(#56854,#56855),(#56856,#56857),(#56858,#56859),(#56860,
#56861),(#56862,#56863),(#56864,#56865),(#56866,#56867),(#56868,#56869),
(#56870,#56871),(#56872,#56873),(#56874,#56875),(#56876,#56877),(#56878,
#56879),(#56880,#56881),(#56882,#56883),(#56884,#56885),(#56886,#56887),
(#56888,#56889),(#56890,#56891),(#56892,#56893),(#56894,#56895),(#56896,
#56897),(#56898,#56899),(#56900,#56901),(#56902,#56903)),.UNSPECIFIED.,
 .F.,.F.,.F.)
B_SPLINE_SURFACE_WITH_KNOTS((6,1,1,1,1,1,1,1,1,1,1,1,1,1,1,1,1,1,1,1,1,
1,1,1,1,1,1,1,1,1,1,1,1,1,1,1,1,1,1,1,1,1,1,1,1,1,1,1,1,1,1,1,1,1,1,1,1,
1,1,1,1,1,1,1,1,6),(2,2),(-1.,-0.984615384615383,-0.969230769230768,-0.953846153846152,
-0.938461538461537,-0.923076923076922,-0.907692307692306,-0.892307692307691,
-0.876923076923076,-0.86153846153846,-0.846153846153845,-0.83076923076923,
-0.815384615384614,-0.799999999999999,-0.784615384615384,-0.769230769230768,
-0.753846153846153,-0.738461538461538,-0.723076923076922,-0.707692307692307,
-0.692307692307692,-0.676923076923076,-0.661538461538461,-0.646153846153846,
-0.63076923076923,-0.615384615384615,-0.6,-0.584615384615384,-0.569230769230769,
-0.553846153846154,-0.538461538461538,-0.523076923076923,-0.507692307692308,
-0.492307692307692,-0.476923076923077,-0.461538461538462,-0.446153846153846,
-0.430769230769231,-0.415384615384615,-0.4,-0.384615384615385,-0.369230769230769,
-0.353846153846154,-0.338461538461538,-0.323076923076923,-0.307692307692308,
-0.292307692307692,-0.276923076923077,-0.261538461538462,-0.246153846153846,
-0.230769230769231,-0.215384615384615,-0.2,-0.184615384615385,-0.169230769230769,
-0.153846153846154,-0.138461538461538,-0.123076923076923,-0.107692307692308,
-0.0923076923076923,-0.0769230769230769,-0.0615384615384615,-0.0461538461538462,
-0.0307692307692308,-0.0153846153846154,0.),(-1.,1.),.UNSPECIFIED.)
GEOMETRIC_REPRESENTATION_ITEM()
RATIONAL_B_SPLINE_SURFACE(((1.,1.),(1.,1.),(1.,1.),(1.,1.),(1.,1.),(1.,
1.),(1.,1.),(1.,1.),(1.,1.),(1.,1.),(1.,1.),(1.,1.),(1.,1.),(1.,1.),(1.,
1.),(1.,1.),(1.,1.),(1.,1.),(1.,1.),(1.,1.),(1.,1.),(1.,1.),(1.,1.),(1.,
1.),(1.,1.),(1.,1.),(1.,1.),(1.,1.),(1.,1.),(1.,1.),(1.,1.),(1.,1.),(1.,
1.),(1.,1.),(1.,1.),(1.,1.),(1.,1.),(1.,1.),(1.,1.),(1.,1.),(1.,1.),(1.,
1.),(1.,1.),(1.,1.),(1.,1.),(1.,1.),(1.,1.),(1.,1.),(1.,1.),(1.,1.),(1.,
1.),(1.,1.),(1.,1.),(1.,1.),(1.,1.),(1.,1.),(1.,1.),(1.,1.),(1.,1.),(1.,
1.),(1.,1.),(1.,1.),(1.,1.),(1.,1.),(1.,1.),(1.,1.),(1.,1.),(1.,1.),(1.,
1.),(1.,1.)))
REPRESENTATION_ITEM('')
SURFACE()
);
#128=(
BOUNDED_SURFACE()
B_SPLINE_SURFACE(5,1,((#56980,#56981),(#56982,#56983),(#56984,#56985),(#56986,
#56987),(#56988,#56989),(#56990,#56991),(#56992,#56993),(#56994,#56995),
(#56996,#56997),(#56998,#56999),(#57000,#57001),(#57002,#57003),(#57004,
#57005),(#57006,#57007),(#57008,#57009),(#57010,#57011),(#57012,#57013),
(#57014,#57015),(#57016,#57017),(#57018,#57019),(#57020,#57021),(#57022,
#57023),(#57024,#57025),(#57026,#57027),(#57028,#57029),(#57030,#57031),
(#57032,#57033),(#57034,#57035),(#57036,#57037),(#57038,#57039),(#57040,
#57041),(#57042,#57043),(#57044,#57045),(#57046,#57047),(#57048,#57049),
(#57050,#57051),(#57052,#57053),(#57054,#57055),(#57056,#57057),(#57058,
#57059),(#57060,#57061),(#57062,#57063),(#57064,#57065),(#57066,#57067),
(#57068,#57069),(#57070,#57071),(#57072,#57073),(#57074,#57075),(#57076,
#57077),(#57078,#57079),(#57080,#57081),(#57082,#57083),(#57084,#57085),
(#57086,#57087),(#57088,#57089),(#57090,#57091),(#57092,#57093),(#57094,
#57095),(#57096,#57097),(#57098,#57099),(#57100,#57101),(#57102,#57103),
(#57104,#57105),(#57106,#57107),(#57108,#57109),(#57110,#57111),(#57112,
#57113),(#57114,#57115),(#57116,#57117),(#57118,#57119)),.UNSPECIFIED.,
 .F.,.F.,.F.)
B_SPLINE_SURFACE_WITH_KNOTS((6,1,1,1,1,1,1,1,1,1,1,1,1,1,1,1,1,1,1,1,1,
1,1,1,1,1,1,1,1,1,1,1,1,1,1,1,1,1,1,1,1,1,1,1,1,1,1,1,1,1,1,1,1,1,1,1,1,
1,1,1,1,1,1,1,1,6),(2,2),(-1.,-0.984615384615383,-0.969230769230768,-0.953846153846152,
-0.938461538461537,-0.923076923076922,-0.907692307692306,-0.892307692307691,
-0.876923076923076,-0.86153846153846,-0.846153846153845,-0.83076923076923,
-0.815384615384614,-0.799999999999999,-0.784615384615384,-0.769230769230768,
-0.753846153846153,-0.738461538461538,-0.723076923076922,-0.707692307692307,
-0.692307692307692,-0.676923076923076,-0.661538461538461,-0.646153846153846,
-0.63076923076923,-0.615384615384615,-0.6,-0.584615384615384,-0.569230769230769,
-0.553846153846154,-0.538461538461538,-0.523076923076923,-0.507692307692308,
-0.492307692307692,-0.476923076923077,-0.461538461538462,-0.446153846153846,
-0.430769230769231,-0.415384615384615,-0.4,-0.384615384615385,-0.369230769230769,
-0.353846153846154,-0.338461538461538,-0.323076923076923,-0.307692307692308,
-0.292307692307692,-0.276923076923077,-0.261538461538462,-0.246153846153846,
-0.230769230769231,-0.215384615384615,-0.2,-0.184615384615385,-0.169230769230769,
-0.153846153846154,-0.138461538461538,-0.123076923076923,-0.107692307692308,
-0.0923076923076923,-0.0769230769230769,-0.0615384615384615,-0.0461538461538462,
-0.0307692307692308,-0.0153846153846154,0.),(-1.,1.),.UNSPECIFIED.)
GEOMETRIC_REPRESENTATION_ITEM()
RATIONAL_B_SPLINE_SURFACE(((1.,1.),(1.,1.),(1.,1.),(1.,1.),(1.,1.),(1.,
1.),(1.,1.),(1.,1.),(1.,1.),(1.,1.),(1.,1.),(1.,1.),(1.,1.),(1.,1.),(1.,
1.),(1.,1.),(1.,1.),(1.,1.),(1.,1.),(1.,1.),(1.,1.),(1.,1.),(1.,1.),(1.,
1.),(1.,1.),(1.,1.),(1.,1.),(1.,1.),(1.,1.),(1.,1.),(1.,1.),(1.,1.),(1.,
1.),(1.,1.),(1.,1.),(1.,1.),(1.,1.),(1.,1.),(1.,1.),(1.,1.),(1.,1.),(1.,
1.),(1.,1.),(1.,1.),(1.,1.),(1.,1.),(1.,1.),(1.,1.),(1.,1.),(1.,1.),(1.,
1.),(1.,1.),(1.,1.),(1.,1.),(1.,1.),(1.,1.),(1.,1.),(1.,1.),(1.,1.),(1.,
1.),(1.,1.),(1.,1.),(1.,1.),(1.,1.),(1.,1.),(1.,1.),(1.,1.),(1.,1.),(1.,
1.),(1.,1.)))
REPRESENTATION_ITEM('')
SURFACE()
);
#129=(
BOUNDED_SURFACE()
B_SPLINE_SURFACE(5,1,((#57206,#57207),(#57208,#57209),(#57210,#57211),(#57212,
#57213),(#57214,#57215),(#57216,#57217),(#57218,#57219),(#57220,#57221),
(#57222,#57223),(#57224,#57225),(#57226,#57227),(#57228,#57229),(#57230,
#57231),(#57232,#57233),(#57234,#57235),(#57236,#57237),(#57238,#57239),
(#57240,#57241),(#57242,#57243),(#57244,#57245),(#57246,#57247),(#57248,
#57249),(#57250,#57251),(#57252,#57253),(#57254,#57255),(#57256,#57257),
(#57258,#57259),(#57260,#57261),(#57262,#57263),(#57264,#57265),(#57266,
#57267),(#57268,#57269),(#57270,#57271),(#57272,#57273),(#57274,#57275),
(#57276,#57277),(#57278,#57279),(#57280,#57281),(#57282,#57283),(#57284,
#57285),(#57286,#57287),(#57288,#57289),(#57290,#57291),(#57292,#57293),
(#57294,#57295),(#57296,#57297),(#57298,#57299),(#57300,#57301),(#57302,
#57303),(#57304,#57305),(#57306,#57307),(#57308,#57309),(#57310,#57311),
(#57312,#57313),(#57314,#57315),(#57316,#57317),(#57318,#57319),(#57320,
#57321),(#57322,#57323),(#57324,#57325),(#57326,#57327),(#57328,#57329),
(#57330,#57331),(#57332,#57333),(#57334,#57335),(#57336,#57337),(#57338,
#57339),(#57340,#57341),(#57342,#57343),(#57344,#57345)),.UNSPECIFIED.,
 .F.,.F.,.F.)
B_SPLINE_SURFACE_WITH_KNOTS((6,1,1,1,1,1,1,1,1,1,1,1,1,1,1,1,1,1,1,1,1,
1,1,1,1,1,1,1,1,1,1,1,1,1,1,1,1,1,1,1,1,1,1,1,1,1,1,1,1,1,1,1,1,1,1,1,1,
1,1,1,1,1,1,1,1,6),(2,2),(-1.,-0.984615384615383,-0.969230769230768,-0.953846153846152,
-0.938461538461537,-0.923076923076922,-0.907692307692306,-0.892307692307691,
-0.876923076923076,-0.86153846153846,-0.846153846153845,-0.83076923076923,
-0.815384615384614,-0.799999999999999,-0.784615384615384,-0.769230769230768,
-0.753846153846153,-0.738461538461538,-0.723076923076922,-0.707692307692307,
-0.692307692307692,-0.676923076923076,-0.661538461538461,-0.646153846153846,
-0.63076923076923,-0.615384615384615,-0.6,-0.584615384615384,-0.569230769230769,
-0.553846153846154,-0.538461538461538,-0.523076923076923,-0.507692307692308,
-0.492307692307692,-0.476923076923077,-0.461538461538462,-0.446153846153846,
-0.430769230769231,-0.415384615384615,-0.4,-0.384615384615385,-0.369230769230769,
-0.353846153846154,-0.338461538461538,-0.323076923076923,-0.307692307692308,
-0.292307692307692,-0.276923076923077,-0.261538461538462,-0.246153846153846,
-0.230769230769231,-0.215384615384615,-0.2,-0.184615384615385,-0.169230769230769,
-0.153846153846154,-0.138461538461538,-0.123076923076923,-0.107692307692308,
-0.0923076923076923,-0.0769230769230769,-0.0615384615384615,-0.0461538461538462,
-0.0307692307692308,-0.0153846153846154,0.),(-1.,1.),.UNSPECIFIED.)
GEOMETRIC_REPRESENTATION_ITEM()
RATIONAL_B_SPLINE_SURFACE(((1.,1.),(1.,1.),(1.,1.),(1.,1.),(1.,1.),(1.,
1.),(1.,1.),(1.,1.),(1.,1.),(1.,1.),(1.,1.),(1.,1.),(1.,1.),(1.,1.),(1.,
1.),(1.,1.),(1.,1.),(1.,1.),(1.,1.),(1.,1.),(1.,1.),(1.,1.),(1.,1.),(1.,
1.),(1.,1.),(1.,1.),(1.,1.),(1.,1.),(1.,1.),(1.,1.),(1.,1.),(1.,1.),(1.,
1.),(1.,1.),(1.,1.),(1.,1.),(1.,1.),(1.,1.),(1.,1.),(1.,1.),(1.,1.),(1.,
1.),(1.,1.),(1.,1.),(1.,1.),(1.,1.),(1.,1.),(1.,1.),(1.,1.),(1.,1.),(1.,
1.),(1.,1.),(1.,1.),(1.,1.),(1.,1.),(1.,1.),(1.,1.),(1.,1.),(1.,1.),(1.,
1.),(1.,1.),(1.,1.),(1.,1.),(1.,1.),(1.,1.),(1.,1.),(1.,1.),(1.,1.),(1.,
1.),(1.,1.)))
REPRESENTATION_ITEM('')
SURFACE()
);
#130=(
BOUNDED_SURFACE()
B_SPLINE_SURFACE(5,1,((#57425,#57426),(#57427,#57428),(#57429,#57430),(#57431,
#57432),(#57433,#57434),(#57435,#57436),(#57437,#57438),(#57439,#57440),
(#57441,#57442),(#57443,#57444),(#57445,#57446),(#57447,#57448),(#57449,
#57450),(#57451,#57452),(#57453,#57454),(#57455,#57456),(#57457,#57458),
(#57459,#57460),(#57461,#57462),(#57463,#57464),(#57465,#57466),(#57467,
#57468),(#57469,#57470),(#57471,#57472),(#57473,#57474),(#57475,#57476),
(#57477,#57478),(#57479,#57480),(#57481,#57482),(#57483,#57484),(#57485,
#57486),(#57487,#57488),(#57489,#57490),(#57491,#57492),(#57493,#57494),
(#57495,#57496),(#57497,#57498),(#57499,#57500),(#57501,#57502),(#57503,
#57504),(#57505,#57506),(#57507,#57508),(#57509,#57510),(#57511,#57512),
(#57513,#57514),(#57515,#57516),(#57517,#57518),(#57519,#57520),(#57521,
#57522),(#57523,#57524),(#57525,#57526),(#57527,#57528),(#57529,#57530),
(#57531,#57532),(#57533,#57534),(#57535,#57536),(#57537,#57538),(#57539,
#57540),(#57541,#57542),(#57543,#57544),(#57545,#57546),(#57547,#57548),
(#57549,#57550),(#57551,#57552),(#57553,#57554),(#57555,#57556),(#57557,
#57558),(#57559,#57560),(#57561,#57562),(#57563,#57564)),.UNSPECIFIED.,
 .F.,.F.,.F.)
B_SPLINE_SURFACE_WITH_KNOTS((6,1,1,1,1,1,1,1,1,1,1,1,1,1,1,1,1,1,1,1,1,
1,1,1,1,1,1,1,1,1,1,1,1,1,1,1,1,1,1,1,1,1,1,1,1,1,1,1,1,1,1,1,1,1,1,1,1,
1,1,1,1,1,1,1,1,6),(2,2),(-1.,-0.984615384615383,-0.969230769230768,-0.953846153846152,
-0.938461538461537,-0.923076923076922,-0.907692307692306,-0.892307692307691,
-0.876923076923076,-0.86153846153846,-0.846153846153845,-0.83076923076923,
-0.815384615384614,-0.799999999999999,-0.784615384615384,-0.769230769230768,
-0.753846153846153,-0.738461538461538,-0.723076923076922,-0.707692307692307,
-0.692307692307692,-0.676923076923076,-0.661538461538461,-0.646153846153846,
-0.63076923076923,-0.615384615384615,-0.6,-0.584615384615384,-0.569230769230769,
-0.553846153846154,-0.538461538461538,-0.523076923076923,-0.507692307692308,
-0.492307692307692,-0.476923076923077,-0.461538461538462,-0.446153846153846,
-0.430769230769231,-0.415384615384615,-0.4,-0.384615384615385,-0.369230769230769,
-0.353846153846154,-0.338461538461538,-0.323076923076923,-0.307692307692308,
-0.292307692307692,-0.276923076923077,-0.261538461538462,-0.246153846153846,
-0.230769230769231,-0.215384615384615,-0.2,-0.184615384615385,-0.169230769230769,
-0.153846153846154,-0.138461538461538,-0.123076923076923,-0.107692307692308,
-0.0923076923076923,-0.0769230769230769,-0.0615384615384615,-0.0461538461538462,
-0.0307692307692308,-0.0153846153846154,0.),(-1.,1.),.UNSPECIFIED.)
GEOMETRIC_REPRESENTATION_ITEM()
RATIONAL_B_SPLINE_SURFACE(((1.,1.),(1.,1.),(1.,1.),(1.,1.),(1.,1.),(1.,
1.),(1.,1.),(1.,1.),(1.,1.),(1.,1.),(1.,1.),(1.,1.),(1.,1.),(1.,1.),(1.,
1.),(1.,1.),(1.,1.),(1.,1.),(1.,1.),(1.,1.),(1.,1.),(1.,1.),(1.,1.),(1.,
1.),(1.,1.),(1.,1.),(1.,1.),(1.,1.),(1.,1.),(1.,1.),(1.,1.),(1.,1.),(1.,
1.),(1.,1.),(1.,1.),(1.,1.),(1.,1.),(1.,1.),(1.,1.),(1.,1.),(1.,1.),(1.,
1.),(1.,1.),(1.,1.),(1.,1.),(1.,1.),(1.,1.),(1.,1.),(1.,1.),(1.,1.),(1.,
1.),(1.,1.),(1.,1.),(1.,1.),(1.,1.),(1.,1.),(1.,1.),(1.,1.),(1.,1.),(1.,
1.),(1.,1.),(1.,1.),(1.,1.),(1.,1.),(1.,1.),(1.,1.),(1.,1.),(1.,1.),(1.,
1.),(1.,1.)))
REPRESENTATION_ITEM('')
SURFACE()
);
#131=(
BOUNDED_CURVE()
B_SPLINE_CURVE(5,(#22250,#22251,#22252,#22253,#22254,#22255,#22256,#22257,
#22258,#22259,#22260,#22261,#22262,#22263,#22264,#22265,#22266,#22267,#22268,
#22269,#22270,#22271,#22272,#22273,#22274,#22275,#22276,#22277,#22278,#22279,
#22280,#22281,#22282,#22283,#22284,#22285,#22286,#22287,#22288,#22289,#22290,
#22291,#22292,#22293,#22294,#22295,#22296,#22297,#22298,#22299,#22300,#22301,
#22302,#22303,#22304,#22305,#22306,#22307,#22308,#22309,#22310,#22311,#22312,
#22313,#22314,#22315,#22316,#22317,#22318,#22319),.UNSPECIFIED.,.F.,.F.)
B_SPLINE_CURVE_WITH_KNOTS((6,1,1,1,1,1,1,1,1,1,1,1,1,1,1,1,1,1,1,1,1,1,
1,1,1,1,1,1,1,1,1,1,1,1,1,1,1,1,1,1,1,1,1,1,1,1,1,1,1,1,1,1,1,1,1,1,1,1,
1,1,1,1,1,1,1,6),(0.,0.0153846153846154,0.0307692307692308,0.0461538461538462,
0.0615384615384615,0.0769230769230769,0.0923076923076923,0.107692307692308,
0.123076923076923,0.138461538461538,0.153846153846154,0.169230769230769,
0.184615384615385,0.2,0.215384615384615,0.230769230769231,0.246153846153846,
0.261538461538462,0.276923076923077,0.292307692307692,0.307692307692308,
0.323076923076923,0.338461538461538,0.353846153846154,0.369230769230769,
0.384615384615385,0.4,0.415384615384615,0.430769230769231,0.446153846153846,
0.461538461538462,0.476923076923077,0.492307692307692,0.507692307692308,
0.523076923076923,0.538461538461538,0.553846153846154,0.569230769230769,
0.584615384615384,0.6,0.615384615384615,0.63076923076923,0.646153846153846,
0.661538461538461,0.676923076923076,0.692307692307692,0.707692307692307,
0.723076923076922,0.738461538461538,0.753846153846153,0.769230769230768,
0.784615384615384,0.799999999999999,0.815384615384614,0.83076923076923,
0.846153846153845,0.86153846153846,0.876923076923076,0.892307692307691,
0.907692307692306,0.923076923076922,0.938461538461537,0.953846153846152,
0.969230769230768,0.984615384615383,1.),.UNSPECIFIED.)
CURVE()
GEOMETRIC_REPRESENTATION_ITEM()
RATIONAL_B_SPLINE_CURVE((1.,1.,1.,1.,1.,1.,1.,1.,1.,1.,1.,1.,1.,1.,1.,1.,
1.,1.,1.,1.,1.,1.,1.,1.,1.,1.,1.,1.,1.,1.,1.,1.,1.,1.,1.,1.,1.,1.,1.,1.,
1.,1.,1.,1.,1.,1.,1.,1.,1.,1.,1.,1.,1.,1.,1.,1.,1.,1.,1.,1.,1.,1.,1.,1.,
1.,1.,1.,1.,1.,1.))
REPRESENTATION_ITEM('')
);
#132=(
BOUNDED_CURVE()
B_SPLINE_CURVE(5,(#22323,#22324,#22325,#22326,#22327,#22328,#22329,#22330,
#22331,#22332,#22333,#22334,#22335,#22336,#22337,#22338,#22339,#22340,#22341,
#22342,#22343,#22344,#22345,#22346,#22347,#22348,#22349,#22350,#22351,#22352,
#22353,#22354,#22355,#22356,#22357,#22358,#22359,#22360,#22361,#22362,#22363,
#22364,#22365,#22366,#22367,#22368,#22369,#22370,#22371,#22372,#22373,#22374,
#22375,#22376,#22377,#22378,#22379,#22380,#22381,#22382,#22383,#22384,#22385,
#22386,#22387,#22388,#22389,#22390,#22391,#22392),.UNSPECIFIED.,.F.,.F.)
B_SPLINE_CURVE_WITH_KNOTS((6,1,1,1,1,1,1,1,1,1,1,1,1,1,1,1,1,1,1,1,1,1,
1,1,1,1,1,1,1,1,1,1,1,1,1,1,1,1,1,1,1,1,1,1,1,1,1,1,1,1,1,1,1,1,1,1,1,1,
1,1,1,1,1,1,1,6),(0.,0.0153846153846154,0.0307692307692308,0.0461538461538462,
0.0615384615384615,0.0769230769230769,0.0923076923076923,0.107692307692308,
0.123076923076923,0.138461538461538,0.153846153846154,0.169230769230769,
0.184615384615385,0.2,0.215384615384615,0.230769230769231,0.246153846153846,
0.261538461538462,0.276923076923077,0.292307692307692,0.307692307692308,
0.323076923076923,0.338461538461538,0.353846153846154,0.369230769230769,
0.384615384615385,0.4,0.415384615384615,0.430769230769231,0.446153846153846,
0.461538461538462,0.476923076923077,0.492307692307692,0.507692307692308,
0.523076923076923,0.538461538461538,0.553846153846154,0.569230769230769,
0.584615384615384,0.6,0.615384615384615,0.63076923076923,0.646153846153846,
0.661538461538461,0.676923076923076,0.692307692307692,0.707692307692307,
0.723076923076922,0.738461538461538,0.753846153846153,0.769230769230768,
0.784615384615384,0.799999999999999,0.815384615384614,0.83076923076923,
0.846153846153845,0.86153846153846,0.876923076923076,0.892307692307691,
0.907692307692306,0.923076923076922,0.938461538461537,0.953846153846152,
0.969230769230768,0.984615384615383,1.),.UNSPECIFIED.)
CURVE()
GEOMETRIC_REPRESENTATION_ITEM()
RATIONAL_B_SPLINE_CURVE((1.,1.,1.,1.,1.,1.,1.,1.,1.,1.,1.,1.,1.,1.,1.,1.,
1.,1.,1.,1.,1.,1.,1.,1.,1.,1.,1.,1.,1.,1.,1.,1.,1.,1.,1.,1.,1.,1.,1.,1.,
1.,1.,1.,1.,1.,1.,1.,1.,1.,1.,1.,1.,1.,1.,1.,1.,1.,1.,1.,1.,1.,1.,1.,1.,
1.,1.,1.,1.,1.,1.))
REPRESENTATION_ITEM('')
);
#133=(
BOUNDED_CURVE()
B_SPLINE_CURVE(5,(#22396,#22397,#22398,#22399,#22400,#22401,#22402,#22403,
#22404,#22405,#22406,#22407,#22408,#22409,#22410,#22411,#22412,#22413,#22414,
#22415,#22416,#22417,#22418,#22419,#22420,#22421,#22422,#22423,#22424,#22425,
#22426,#22427,#22428,#22429,#22430,#22431,#22432,#22433,#22434,#22435,#22436,
#22437,#22438,#22439,#22440,#22441,#22442,#22443,#22444,#22445,#22446,#22447,
#22448,#22449,#22450,#22451,#22452,#22453,#22454,#22455,#22456,#22457,#22458,
#22459,#22460,#22461,#22462,#22463,#22464,#22465),.UNSPECIFIED.,.F.,.F.)
B_SPLINE_CURVE_WITH_KNOTS((6,1,1,1,1,1,1,1,1,1,1,1,1,1,1,1,1,1,1,1,1,1,
1,1,1,1,1,1,1,1,1,1,1,1,1,1,1,1,1,1,1,1,1,1,1,1,1,1,1,1,1,1,1,1,1,1,1,1,
1,1,1,1,1,1,1,6),(0.,0.0153846153846154,0.0307692307692308,0.0461538461538462,
0.0615384615384615,0.0769230769230769,0.0923076923076923,0.107692307692308,
0.123076923076923,0.138461538461538,0.153846153846154,0.169230769230769,
0.184615384615385,0.2,0.215384615384615,0.230769230769231,0.246153846153846,
0.261538461538462,0.276923076923077,0.292307692307692,0.307692307692308,
0.323076923076923,0.338461538461538,0.353846153846154,0.369230769230769,
0.384615384615385,0.4,0.415384615384615,0.430769230769231,0.446153846153846,
0.461538461538462,0.476923076923077,0.492307692307692,0.507692307692308,
0.523076923076923,0.538461538461538,0.553846153846154,0.569230769230769,
0.584615384615384,0.6,0.615384615384615,0.63076923076923,0.646153846153846,
0.661538461538461,0.676923076923076,0.692307692307692,0.707692307692307,
0.723076923076922,0.738461538461538,0.753846153846153,0.769230769230768,
0.784615384615384,0.799999999999999,0.815384615384614,0.83076923076923,
0.846153846153845,0.86153846153846,0.876923076923076,0.892307692307691,
0.907692307692306,0.923076923076922,0.938461538461537,0.953846153846152,
0.969230769230768,0.984615384615383,1.),.UNSPECIFIED.)
CURVE()
GEOMETRIC_REPRESENTATION_ITEM()
RATIONAL_B_SPLINE_CURVE((1.,1.,1.,1.,1.,1.,1.,1.,1.,1.,1.,1.,1.,1.,1.,1.,
1.,1.,1.,1.,1.,1.,1.,1.,1.,1.,1.,1.,1.,1.,1.,1.,1.,1.,1.,1.,1.,1.,1.,1.,
1.,1.,1.,1.,1.,1.,1.,1.,1.,1.,1.,1.,1.,1.,1.,1.,1.,1.,1.,1.,1.,1.,1.,1.,
1.,1.,1.,1.,1.,1.))
REPRESENTATION_ITEM('')
);
#134=(
BOUNDED_CURVE()
B_SPLINE_CURVE(5,(#22469,#22470,#22471,#22472,#22473,#22474,#22475,#22476,
#22477,#22478,#22479,#22480,#22481,#22482,#22483,#22484,#22485,#22486,#22487,
#22488,#22489,#22490,#22491,#22492,#22493,#22494,#22495,#22496,#22497,#22498,
#22499,#22500,#22501,#22502,#22503,#22504,#22505,#22506,#22507,#22508,#22509,
#22510,#22511,#22512,#22513,#22514,#22515,#22516,#22517,#22518,#22519,#22520,
#22521,#22522,#22523,#22524,#22525,#22526,#22527,#22528,#22529,#22530,#22531,
#22532,#22533,#22534,#22535,#22536,#22537,#22538),.UNSPECIFIED.,.F.,.F.)
B_SPLINE_CURVE_WITH_KNOTS((6,1,1,1,1,1,1,1,1,1,1,1,1,1,1,1,1,1,1,1,1,1,
1,1,1,1,1,1,1,1,1,1,1,1,1,1,1,1,1,1,1,1,1,1,1,1,1,1,1,1,1,1,1,1,1,1,1,1,
1,1,1,1,1,1,1,6),(0.,0.0153846153846154,0.0307692307692308,0.0461538461538462,
0.0615384615384615,0.0769230769230769,0.0923076923076923,0.107692307692308,
0.123076923076923,0.138461538461538,0.153846153846154,0.169230769230769,
0.184615384615385,0.2,0.215384615384615,0.230769230769231,0.246153846153846,
0.261538461538462,0.276923076923077,0.292307692307692,0.307692307692308,
0.323076923076923,0.338461538461538,0.353846153846154,0.369230769230769,
0.384615384615385,0.4,0.415384615384615,0.430769230769231,0.446153846153846,
0.461538461538462,0.476923076923077,0.492307692307692,0.507692307692308,
0.523076923076923,0.538461538461538,0.553846153846154,0.569230769230769,
0.584615384615384,0.6,0.615384615384615,0.63076923076923,0.646153846153846,
0.661538461538461,0.676923076923076,0.692307692307692,0.707692307692307,
0.723076923076922,0.738461538461538,0.753846153846153,0.769230769230768,
0.784615384615384,0.799999999999999,0.815384615384614,0.83076923076923,
0.846153846153845,0.86153846153846,0.876923076923076,0.892307692307691,
0.907692307692306,0.923076923076922,0.938461538461537,0.953846153846152,
0.969230769230768,0.984615384615383,1.),.UNSPECIFIED.)
CURVE()
GEOMETRIC_REPRESENTATION_ITEM()
RATIONAL_B_SPLINE_CURVE((1.,1.,1.,1.,1.,1.,1.,1.,1.,1.,1.,1.,1.,1.,1.,1.,
1.,1.,1.,1.,1.,1.,1.,1.,1.,1.,1.,1.,1.,1.,1.,1.,1.,1.,1.,1.,1.,1.,1.,1.,
1.,1.,1.,1.,1.,1.,1.,1.,1.,1.,1.,1.,1.,1.,1.,1.,1.,1.,1.,1.,1.,1.,1.,1.,
1.,1.,1.,1.,1.,1.))
REPRESENTATION_ITEM('')
);
#135=(
BOUNDED_CURVE()
B_SPLINE_CURVE(5,(#22542,#22543,#22544,#22545,#22546,#22547,#22548,#22549,
#22550,#22551,#22552,#22553,#22554,#22555,#22556,#22557,#22558,#22559,#22560,
#22561,#22562,#22563,#22564,#22565,#22566,#22567,#22568,#22569,#22570,#22571,
#22572,#22573,#22574,#22575,#22576,#22577,#22578,#22579,#22580,#22581,#22582,
#22583,#22584,#22585,#22586,#22587,#22588,#22589,#22590,#22591,#22592,#22593,
#22594,#22595,#22596,#22597,#22598,#22599,#22600,#22601,#22602,#22603,#22604,
#22605,#22606,#22607,#22608,#22609,#22610,#22611),.UNSPECIFIED.,.F.,.F.)
B_SPLINE_CURVE_WITH_KNOTS((6,1,1,1,1,1,1,1,1,1,1,1,1,1,1,1,1,1,1,1,1,1,
1,1,1,1,1,1,1,1,1,1,1,1,1,1,1,1,1,1,1,1,1,1,1,1,1,1,1,1,1,1,1,1,1,1,1,1,
1,1,1,1,1,1,1,6),(0.,0.0153846153846154,0.0307692307692308,0.0461538461538462,
0.0615384615384615,0.0769230769230769,0.0923076923076923,0.107692307692308,
0.123076923076923,0.138461538461538,0.153846153846154,0.169230769230769,
0.184615384615385,0.2,0.215384615384615,0.230769230769231,0.246153846153846,
0.261538461538462,0.276923076923077,0.292307692307692,0.307692307692308,
0.323076923076923,0.338461538461538,0.353846153846154,0.369230769230769,
0.384615384615385,0.4,0.415384615384615,0.430769230769231,0.446153846153846,
0.461538461538462,0.476923076923077,0.492307692307692,0.507692307692308,
0.523076923076923,0.538461538461538,0.553846153846154,0.569230769230769,
0.584615384615384,0.6,0.615384615384615,0.63076923076923,0.646153846153846,
0.661538461538461,0.676923076923076,0.692307692307692,0.707692307692307,
0.723076923076922,0.738461538461538,0.753846153846153,0.769230769230768,
0.784615384615384,0.799999999999999,0.815384615384614,0.83076923076923,
0.846153846153845,0.86153846153846,0.876923076923076,0.892307692307691,
0.907692307692306,0.923076923076922,0.938461538461537,0.953846153846152,
0.969230769230768,0.984615384615383,1.),.UNSPECIFIED.)
CURVE()
GEOMETRIC_REPRESENTATION_ITEM()
RATIONAL_B_SPLINE_CURVE((1.,1.,1.,1.,1.,1.,1.,1.,1.,1.,1.,1.,1.,1.,1.,1.,
1.,1.,1.,1.,1.,1.,1.,1.,1.,1.,1.,1.,1.,1.,1.,1.,1.,1.,1.,1.,1.,1.,1.,1.,
1.,1.,1.,1.,1.,1.,1.,1.,1.,1.,1.,1.,1.,1.,1.,1.,1.,1.,1.,1.,1.,1.,1.,1.,
1.,1.,1.,1.,1.,1.))
REPRESENTATION_ITEM('')
);
#136=(
BOUNDED_CURVE()
B_SPLINE_CURVE(5,(#22615,#22616,#22617,#22618,#22619,#22620,#22621,#22622,
#22623,#22624,#22625,#22626,#22627,#22628,#22629,#22630,#22631,#22632,#22633,
#22634,#22635,#22636,#22637,#22638,#22639,#22640,#22641,#22642,#22643,#22644,
#22645,#22646,#22647,#22648,#22649,#22650,#22651,#22652,#22653,#22654,#22655,
#22656,#22657,#22658,#22659,#22660,#22661,#22662,#22663,#22664,#22665,#22666,
#22667,#22668,#22669,#22670,#22671,#22672,#22673,#22674,#22675,#22676,#22677,
#22678,#22679,#22680,#22681,#22682,#22683,#22684),.UNSPECIFIED.,.F.,.F.)
B_SPLINE_CURVE_WITH_KNOTS((6,1,1,1,1,1,1,1,1,1,1,1,1,1,1,1,1,1,1,1,1,1,
1,1,1,1,1,1,1,1,1,1,1,1,1,1,1,1,1,1,1,1,1,1,1,1,1,1,1,1,1,1,1,1,1,1,1,1,
1,1,1,1,1,1,1,6),(0.,0.0153846153846154,0.0307692307692308,0.0461538461538462,
0.0615384615384615,0.0769230769230769,0.0923076923076923,0.107692307692308,
0.123076923076923,0.138461538461538,0.153846153846154,0.169230769230769,
0.184615384615385,0.2,0.215384615384615,0.230769230769231,0.246153846153846,
0.261538461538462,0.276923076923077,0.292307692307692,0.307692307692308,
0.323076923076923,0.338461538461538,0.353846153846154,0.369230769230769,
0.384615384615385,0.4,0.415384615384615,0.430769230769231,0.446153846153846,
0.461538461538462,0.476923076923077,0.492307692307692,0.507692307692308,
0.523076923076923,0.538461538461538,0.553846153846154,0.569230769230769,
0.584615384615384,0.6,0.615384615384615,0.63076923076923,0.646153846153846,
0.661538461538461,0.676923076923076,0.692307692307692,0.707692307692307,
0.723076923076922,0.738461538461538,0.753846153846153,0.769230769230768,
0.784615384615384,0.799999999999999,0.815384615384614,0.83076923076923,
0.846153846153845,0.86153846153846,0.876923076923076,0.892307692307691,
0.907692307692306,0.923076923076922,0.938461538461537,0.953846153846152,
0.969230769230768,0.984615384615383,1.),.UNSPECIFIED.)
CURVE()
GEOMETRIC_REPRESENTATION_ITEM()
RATIONAL_B_SPLINE_CURVE((1.,1.,1.,1.,1.,1.,1.,1.,1.,1.,1.,1.,1.,1.,1.,1.,
1.,1.,1.,1.,1.,1.,1.,1.,1.,1.,1.,1.,1.,1.,1.,1.,1.,1.,1.,1.,1.,1.,1.,1.,
1.,1.,1.,1.,1.,1.,1.,1.,1.,1.,1.,1.,1.,1.,1.,1.,1.,1.,1.,1.,1.,1.,1.,1.,
1.,1.,1.,1.,1.,1.))
REPRESENTATION_ITEM('')
);
#137=(
BOUNDED_CURVE()
B_SPLINE_CURVE(5,(#22688,#22689,#22690,#22691,#22692,#22693,#22694,#22695,
#22696,#22697,#22698,#22699,#22700,#22701,#22702,#22703,#22704,#22705,#22706,
#22707,#22708,#22709,#22710,#22711,#22712,#22713,#22714,#22715,#22716,#22717,
#22718,#22719,#22720,#22721,#22722,#22723,#22724,#22725,#22726,#22727,#22728,
#22729,#22730,#22731,#22732,#22733,#22734,#22735,#22736,#22737,#22738,#22739,
#22740,#22741,#22742,#22743,#22744,#22745,#22746,#22747,#22748,#22749,#22750,
#22751,#22752,#22753,#22754,#22755,#22756,#22757),.UNSPECIFIED.,.F.,.F.)
B_SPLINE_CURVE_WITH_KNOTS((6,1,1,1,1,1,1,1,1,1,1,1,1,1,1,1,1,1,1,1,1,1,
1,1,1,1,1,1,1,1,1,1,1,1,1,1,1,1,1,1,1,1,1,1,1,1,1,1,1,1,1,1,1,1,1,1,1,1,
1,1,1,1,1,1,1,6),(0.,0.0153846153846154,0.0307692307692308,0.0461538461538462,
0.0615384615384615,0.0769230769230769,0.0923076923076923,0.107692307692308,
0.123076923076923,0.138461538461538,0.153846153846154,0.169230769230769,
0.184615384615385,0.2,0.215384615384615,0.230769230769231,0.246153846153846,
0.261538461538462,0.276923076923077,0.292307692307692,0.307692307692308,
0.323076923076923,0.338461538461538,0.353846153846154,0.369230769230769,
0.384615384615385,0.4,0.415384615384615,0.430769230769231,0.446153846153846,
0.461538461538462,0.476923076923077,0.492307692307692,0.507692307692308,
0.523076923076923,0.538461538461538,0.553846153846154,0.569230769230769,
0.584615384615384,0.6,0.615384615384615,0.63076923076923,0.646153846153846,
0.661538461538461,0.676923076923076,0.692307692307692,0.707692307692307,
0.723076923076922,0.738461538461538,0.753846153846153,0.769230769230768,
0.784615384615384,0.799999999999999,0.815384615384614,0.83076923076923,
0.846153846153845,0.86153846153846,0.876923076923076,0.892307692307691,
0.907692307692306,0.923076923076922,0.938461538461537,0.953846153846152,
0.969230769230768,0.984615384615383,1.),.UNSPECIFIED.)
CURVE()
GEOMETRIC_REPRESENTATION_ITEM()
RATIONAL_B_SPLINE_CURVE((1.,1.,1.,1.,1.,1.,1.,1.,1.,1.,1.,1.,1.,1.,1.,1.,
1.,1.,1.,1.,1.,1.,1.,1.,1.,1.,1.,1.,1.,1.,1.,1.,1.,1.,1.,1.,1.,1.,1.,1.,
1.,1.,1.,1.,1.,1.,1.,1.,1.,1.,1.,1.,1.,1.,1.,1.,1.,1.,1.,1.,1.,1.,1.,1.,
1.,1.,1.,1.,1.,1.))
REPRESENTATION_ITEM('')
);
#138=(
BOUNDED_CURVE()
B_SPLINE_CURVE(5,(#22761,#22762,#22763,#22764,#22765,#22766,#22767,#22768,
#22769,#22770,#22771,#22772,#22773,#22774,#22775,#22776,#22777,#22778,#22779,
#22780,#22781,#22782,#22783,#22784,#22785,#22786,#22787,#22788,#22789,#22790,
#22791,#22792,#22793,#22794,#22795,#22796,#22797,#22798,#22799,#22800,#22801,
#22802,#22803,#22804,#22805,#22806,#22807,#22808,#22809,#22810,#22811,#22812,
#22813,#22814,#22815,#22816,#22817,#22818,#22819,#22820,#22821,#22822,#22823,
#22824,#22825,#22826,#22827,#22828,#22829,#22830),.UNSPECIFIED.,.F.,.F.)
B_SPLINE_CURVE_WITH_KNOTS((6,1,1,1,1,1,1,1,1,1,1,1,1,1,1,1,1,1,1,1,1,1,
1,1,1,1,1,1,1,1,1,1,1,1,1,1,1,1,1,1,1,1,1,1,1,1,1,1,1,1,1,1,1,1,1,1,1,1,
1,1,1,1,1,1,1,6),(0.,0.0153846153846154,0.0307692307692308,0.0461538461538462,
0.0615384615384615,0.0769230769230769,0.0923076923076923,0.107692307692308,
0.123076923076923,0.138461538461538,0.153846153846154,0.169230769230769,
0.184615384615385,0.2,0.215384615384615,0.230769230769231,0.246153846153846,
0.261538461538462,0.276923076923077,0.292307692307692,0.307692307692308,
0.323076923076923,0.338461538461538,0.353846153846154,0.369230769230769,
0.384615384615385,0.4,0.415384615384615,0.430769230769231,0.446153846153846,
0.461538461538462,0.476923076923077,0.492307692307692,0.507692307692308,
0.523076923076923,0.538461538461538,0.553846153846154,0.569230769230769,
0.584615384615384,0.6,0.615384615384615,0.63076923076923,0.646153846153846,
0.661538461538461,0.676923076923076,0.692307692307692,0.707692307692307,
0.723076923076922,0.738461538461538,0.753846153846153,0.769230769230768,
0.784615384615384,0.799999999999999,0.815384615384614,0.83076923076923,
0.846153846153845,0.86153846153846,0.876923076923076,0.892307692307691,
0.907692307692306,0.923076923076922,0.938461538461537,0.953846153846152,
0.969230769230768,0.984615384615383,1.),.UNSPECIFIED.)
CURVE()
GEOMETRIC_REPRESENTATION_ITEM()
RATIONAL_B_SPLINE_CURVE((1.,1.,1.,1.,1.,1.,1.,1.,1.,1.,1.,1.,1.,1.,1.,1.,
1.,1.,1.,1.,1.,1.,1.,1.,1.,1.,1.,1.,1.,1.,1.,1.,1.,1.,1.,1.,1.,1.,1.,1.,
1.,1.,1.,1.,1.,1.,1.,1.,1.,1.,1.,1.,1.,1.,1.,1.,1.,1.,1.,1.,1.,1.,1.,1.,
1.,1.,1.,1.,1.,1.))
REPRESENTATION_ITEM('')
);
#139=(
BOUNDED_CURVE()
B_SPLINE_CURVE(5,(#22834,#22835,#22836,#22837,#22838,#22839,#22840,#22841,
#22842,#22843,#22844,#22845,#22846,#22847,#22848,#22849,#22850,#22851,#22852,
#22853,#22854,#22855,#22856,#22857,#22858,#22859,#22860,#22861,#22862,#22863,
#22864,#22865,#22866,#22867,#22868,#22869,#22870,#22871,#22872,#22873,#22874,
#22875,#22876,#22877,#22878,#22879,#22880,#22881,#22882,#22883,#22884,#22885,
#22886,#22887,#22888,#22889,#22890,#22891,#22892,#22893,#22894,#22895,#22896,
#22897,#22898,#22899,#22900,#22901,#22902,#22903),.UNSPECIFIED.,.F.,.F.)
B_SPLINE_CURVE_WITH_KNOTS((6,1,1,1,1,1,1,1,1,1,1,1,1,1,1,1,1,1,1,1,1,1,
1,1,1,1,1,1,1,1,1,1,1,1,1,1,1,1,1,1,1,1,1,1,1,1,1,1,1,1,1,1,1,1,1,1,1,1,
1,1,1,1,1,1,1,6),(0.,0.0153846153846154,0.0307692307692308,0.0461538461538462,
0.0615384615384615,0.0769230769230769,0.0923076923076923,0.107692307692308,
0.123076923076923,0.138461538461538,0.153846153846154,0.169230769230769,
0.184615384615385,0.2,0.215384615384615,0.230769230769231,0.246153846153846,
0.261538461538462,0.276923076923077,0.292307692307692,0.307692307692308,
0.323076923076923,0.338461538461538,0.353846153846154,0.369230769230769,
0.384615384615385,0.4,0.415384615384615,0.430769230769231,0.446153846153846,
0.461538461538462,0.476923076923077,0.492307692307692,0.507692307692308,
0.523076923076923,0.538461538461538,0.553846153846154,0.569230769230769,
0.584615384615384,0.6,0.615384615384615,0.63076923076923,0.646153846153846,
0.661538461538461,0.676923076923076,0.692307692307692,0.707692307692307,
0.723076923076922,0.738461538461538,0.753846153846153,0.769230769230768,
0.784615384615384,0.799999999999999,0.815384615384614,0.83076923076923,
0.846153846153845,0.86153846153846,0.876923076923076,0.892307692307691,
0.907692307692306,0.923076923076922,0.938461538461537,0.953846153846152,
0.969230769230768,0.984615384615383,1.),.UNSPECIFIED.)
CURVE()
GEOMETRIC_REPRESENTATION_ITEM()
RATIONAL_B_SPLINE_CURVE((1.,1.,1.,1.,1.,1.,1.,1.,1.,1.,1.,1.,1.,1.,1.,1.,
1.,1.,1.,1.,1.,1.,1.,1.,1.,1.,1.,1.,1.,1.,1.,1.,1.,1.,1.,1.,1.,1.,1.,1.,
1.,1.,1.,1.,1.,1.,1.,1.,1.,1.,1.,1.,1.,1.,1.,1.,1.,1.,1.,1.,1.,1.,1.,1.,
1.,1.,1.,1.,1.,1.))
REPRESENTATION_ITEM('')
);
#140=(
BOUNDED_CURVE()
B_SPLINE_CURVE(5,(#22907,#22908,#22909,#22910,#22911,#22912,#22913,#22914,
#22915,#22916,#22917,#22918,#22919,#22920,#22921,#22922,#22923,#22924,#22925,
#22926,#22927,#22928,#22929,#22930,#22931,#22932,#22933,#22934,#22935,#22936,
#22937,#22938,#22939,#22940,#22941,#22942,#22943,#22944,#22945,#22946,#22947,
#22948,#22949,#22950,#22951,#22952,#22953,#22954,#22955,#22956,#22957,#22958,
#22959,#22960,#22961,#22962,#22963,#22964,#22965,#22966,#22967,#22968,#22969,
#22970,#22971,#22972,#22973,#22974,#22975,#22976),.UNSPECIFIED.,.F.,.F.)
B_SPLINE_CURVE_WITH_KNOTS((6,1,1,1,1,1,1,1,1,1,1,1,1,1,1,1,1,1,1,1,1,1,
1,1,1,1,1,1,1,1,1,1,1,1,1,1,1,1,1,1,1,1,1,1,1,1,1,1,1,1,1,1,1,1,1,1,1,1,
1,1,1,1,1,1,1,6),(0.,0.0153846153846154,0.0307692307692308,0.0461538461538462,
0.0615384615384615,0.0769230769230769,0.0923076923076923,0.107692307692308,
0.123076923076923,0.138461538461538,0.153846153846154,0.169230769230769,
0.184615384615385,0.2,0.215384615384615,0.230769230769231,0.246153846153846,
0.261538461538462,0.276923076923077,0.292307692307692,0.307692307692308,
0.323076923076923,0.338461538461538,0.353846153846154,0.369230769230769,
0.384615384615385,0.4,0.415384615384615,0.430769230769231,0.446153846153846,
0.461538461538462,0.476923076923077,0.492307692307692,0.507692307692308,
0.523076923076923,0.538461538461538,0.553846153846154,0.569230769230769,
0.584615384615384,0.6,0.615384615384615,0.63076923076923,0.646153846153846,
0.661538461538461,0.676923076923076,0.692307692307692,0.707692307692307,
0.723076923076922,0.738461538461538,0.753846153846153,0.769230769230768,
0.784615384615384,0.799999999999999,0.815384615384614,0.83076923076923,
0.846153846153845,0.86153846153846,0.876923076923076,0.892307692307691,
0.907692307692306,0.923076923076922,0.938461538461537,0.953846153846152,
0.969230769230768,0.984615384615383,1.),.UNSPECIFIED.)
CURVE()
GEOMETRIC_REPRESENTATION_ITEM()
RATIONAL_B_SPLINE_CURVE((1.,1.,1.,1.,1.,1.,1.,1.,1.,1.,1.,1.,1.,1.,1.,1.,
1.,1.,1.,1.,1.,1.,1.,1.,1.,1.,1.,1.,1.,1.,1.,1.,1.,1.,1.,1.,1.,1.,1.,1.,
1.,1.,1.,1.,1.,1.,1.,1.,1.,1.,1.,1.,1.,1.,1.,1.,1.,1.,1.,1.,1.,1.,1.,1.,
1.,1.,1.,1.,1.,1.))
REPRESENTATION_ITEM('')
);
#141=(
BOUNDED_CURVE()
B_SPLINE_CURVE(5,(#22980,#22981,#22982,#22983,#22984,#22985,#22986,#22987,
#22988,#22989,#22990,#22991,#22992,#22993,#22994,#22995,#22996,#22997,#22998,
#22999,#23000,#23001,#23002,#23003,#23004,#23005,#23006,#23007,#23008,#23009,
#23010,#23011,#23012,#23013,#23014,#23015,#23016,#23017,#23018,#23019,#23020,
#23021,#23022,#23023,#23024,#23025,#23026,#23027,#23028,#23029,#23030,#23031,
#23032,#23033,#23034,#23035,#23036,#23037,#23038,#23039,#23040,#23041,#23042,
#23043,#23044,#23045,#23046,#23047,#23048,#23049),.UNSPECIFIED.,.F.,.F.)
B_SPLINE_CURVE_WITH_KNOTS((6,1,1,1,1,1,1,1,1,1,1,1,1,1,1,1,1,1,1,1,1,1,
1,1,1,1,1,1,1,1,1,1,1,1,1,1,1,1,1,1,1,1,1,1,1,1,1,1,1,1,1,1,1,1,1,1,1,1,
1,1,1,1,1,1,1,6),(0.,0.0153846153846154,0.0307692307692308,0.0461538461538462,
0.0615384615384615,0.0769230769230769,0.0923076923076923,0.107692307692308,
0.123076923076923,0.138461538461538,0.153846153846154,0.169230769230769,
0.184615384615385,0.2,0.215384615384615,0.230769230769231,0.246153846153846,
0.261538461538462,0.276923076923077,0.292307692307692,0.307692307692308,
0.323076923076923,0.338461538461538,0.353846153846154,0.369230769230769,
0.384615384615385,0.4,0.415384615384615,0.430769230769231,0.446153846153846,
0.461538461538462,0.476923076923077,0.492307692307692,0.507692307692308,
0.523076923076923,0.538461538461538,0.553846153846154,0.569230769230769,
0.584615384615384,0.6,0.615384615384615,0.63076923076923,0.646153846153846,
0.661538461538461,0.676923076923076,0.692307692307692,0.707692307692307,
0.723076923076922,0.738461538461538,0.753846153846153,0.769230769230768,
0.784615384615384,0.799999999999999,0.815384615384614,0.83076923076923,
0.846153846153845,0.86153846153846,0.876923076923076,0.892307692307691,
0.907692307692306,0.923076923076922,0.938461538461537,0.953846153846152,
0.969230769230768,0.984615384615383,1.),.UNSPECIFIED.)
CURVE()
GEOMETRIC_REPRESENTATION_ITEM()
RATIONAL_B_SPLINE_CURVE((1.,1.,1.,1.,1.,1.,1.,1.,1.,1.,1.,1.,1.,1.,1.,1.,
1.,1.,1.,1.,1.,1.,1.,1.,1.,1.,1.,1.,1.,1.,1.,1.,1.,1.,1.,1.,1.,1.,1.,1.,
1.,1.,1.,1.,1.,1.,1.,1.,1.,1.,1.,1.,1.,1.,1.,1.,1.,1.,1.,1.,1.,1.,1.,1.,
1.,1.,1.,1.,1.,1.))
REPRESENTATION_ITEM('')
);
#142=(
BOUNDED_CURVE()
B_SPLINE_CURVE(5,(#23053,#23054,#23055,#23056,#23057,#23058,#23059,#23060,
#23061,#23062,#23063,#23064,#23065,#23066,#23067,#23068,#23069,#23070,#23071,
#23072,#23073,#23074,#23075,#23076,#23077,#23078,#23079,#23080,#23081,#23082,
#23083,#23084,#23085,#23086,#23087,#23088,#23089,#23090,#23091,#23092,#23093,
#23094,#23095,#23096,#23097,#23098,#23099,#23100,#23101,#23102,#23103,#23104,
#23105,#23106,#23107,#23108,#23109,#23110,#23111,#23112,#23113,#23114,#23115,
#23116,#23117,#23118,#23119,#23120,#23121,#23122),.UNSPECIFIED.,.F.,.F.)
B_SPLINE_CURVE_WITH_KNOTS((6,1,1,1,1,1,1,1,1,1,1,1,1,1,1,1,1,1,1,1,1,1,
1,1,1,1,1,1,1,1,1,1,1,1,1,1,1,1,1,1,1,1,1,1,1,1,1,1,1,1,1,1,1,1,1,1,1,1,
1,1,1,1,1,1,1,6),(0.,0.0153846153846154,0.0307692307692308,0.0461538461538462,
0.0615384615384615,0.0769230769230769,0.0923076923076923,0.107692307692308,
0.123076923076923,0.138461538461538,0.153846153846154,0.169230769230769,
0.184615384615385,0.2,0.215384615384615,0.230769230769231,0.246153846153846,
0.261538461538462,0.276923076923077,0.292307692307692,0.307692307692308,
0.323076923076923,0.338461538461538,0.353846153846154,0.369230769230769,
0.384615384615385,0.4,0.415384615384615,0.430769230769231,0.446153846153846,
0.461538461538462,0.476923076923077,0.492307692307692,0.507692307692308,
0.523076923076923,0.538461538461538,0.553846153846154,0.569230769230769,
0.584615384615384,0.6,0.615384615384615,0.63076923076923,0.646153846153846,
0.661538461538461,0.676923076923076,0.692307692307692,0.707692307692307,
0.723076923076922,0.738461538461538,0.753846153846153,0.769230769230768,
0.784615384615384,0.799999999999999,0.815384615384614,0.83076923076923,
0.846153846153845,0.86153846153846,0.876923076923076,0.892307692307691,
0.907692307692306,0.923076923076922,0.938461538461537,0.953846153846152,
0.969230769230768,0.984615384615383,1.),.UNSPECIFIED.)
CURVE()
GEOMETRIC_REPRESENTATION_ITEM()
RATIONAL_B_SPLINE_CURVE((1.,1.,1.,1.,1.,1.,1.,1.,1.,1.,1.,1.,1.,1.,1.,1.,
1.,1.,1.,1.,1.,1.,1.,1.,1.,1.,1.,1.,1.,1.,1.,1.,1.,1.,1.,1.,1.,1.,1.,1.,
1.,1.,1.,1.,1.,1.,1.,1.,1.,1.,1.,1.,1.,1.,1.,1.,1.,1.,1.,1.,1.,1.,1.,1.,
1.,1.,1.,1.,1.,1.))
REPRESENTATION_ITEM('')
);
#143=(
BOUNDED_CURVE()
B_SPLINE_CURVE(5,(#23126,#23127,#23128,#23129,#23130,#23131,#23132,#23133,
#23134,#23135,#23136,#23137,#23138,#23139,#23140,#23141,#23142,#23143,#23144,
#23145,#23146,#23147,#23148,#23149,#23150,#23151,#23152,#23153,#23154,#23155,
#23156,#23157,#23158,#23159,#23160,#23161,#23162,#23163,#23164,#23165,#23166,
#23167,#23168,#23169,#23170,#23171,#23172,#23173,#23174,#23175,#23176,#23177,
#23178,#23179,#23180,#23181,#23182,#23183,#23184,#23185,#23186,#23187,#23188,
#23189,#23190,#23191,#23192,#23193,#23194,#23195),.UNSPECIFIED.,.F.,.F.)
B_SPLINE_CURVE_WITH_KNOTS((6,1,1,1,1,1,1,1,1,1,1,1,1,1,1,1,1,1,1,1,1,1,
1,1,1,1,1,1,1,1,1,1,1,1,1,1,1,1,1,1,1,1,1,1,1,1,1,1,1,1,1,1,1,1,1,1,1,1,
1,1,1,1,1,1,1,6),(0.,0.0153846153846154,0.0307692307692308,0.0461538461538462,
0.0615384615384615,0.0769230769230769,0.0923076923076923,0.107692307692308,
0.123076923076923,0.138461538461538,0.153846153846154,0.169230769230769,
0.184615384615385,0.2,0.215384615384615,0.230769230769231,0.246153846153846,
0.261538461538462,0.276923076923077,0.292307692307692,0.307692307692308,
0.323076923076923,0.338461538461538,0.353846153846154,0.369230769230769,
0.384615384615385,0.4,0.415384615384615,0.430769230769231,0.446153846153846,
0.461538461538462,0.476923076923077,0.492307692307692,0.507692307692308,
0.523076923076923,0.538461538461538,0.553846153846154,0.569230769230769,
0.584615384615384,0.6,0.615384615384615,0.63076923076923,0.646153846153846,
0.661538461538461,0.676923076923076,0.692307692307692,0.707692307692307,
0.723076923076922,0.738461538461538,0.753846153846153,0.769230769230768,
0.784615384615384,0.799999999999999,0.815384615384614,0.83076923076923,
0.846153846153845,0.86153846153846,0.876923076923076,0.892307692307691,
0.907692307692306,0.923076923076922,0.938461538461537,0.953846153846152,
0.969230769230768,0.984615384615383,1.),.UNSPECIFIED.)
CURVE()
GEOMETRIC_REPRESENTATION_ITEM()
RATIONAL_B_SPLINE_CURVE((1.,1.,1.,1.,1.,1.,1.,1.,1.,1.,1.,1.,1.,1.,1.,1.,
1.,1.,1.,1.,1.,1.,1.,1.,1.,1.,1.,1.,1.,1.,1.,1.,1.,1.,1.,1.,1.,1.,1.,1.,
1.,1.,1.,1.,1.,1.,1.,1.,1.,1.,1.,1.,1.,1.,1.,1.,1.,1.,1.,1.,1.,1.,1.,1.,
1.,1.,1.,1.,1.,1.))
REPRESENTATION_ITEM('')
);
#144=(
BOUNDED_CURVE()
B_SPLINE_CURVE(5,(#23199,#23200,#23201,#23202,#23203,#23204,#23205,#23206,
#23207,#23208,#23209,#23210,#23211,#23212,#23213,#23214,#23215,#23216,#23217,
#23218,#23219,#23220,#23221,#23222,#23223,#23224,#23225,#23226,#23227,#23228,
#23229,#23230,#23231,#23232,#23233,#23234,#23235,#23236,#23237,#23238,#23239,
#23240,#23241,#23242,#23243,#23244,#23245,#23246,#23247,#23248,#23249,#23250,
#23251,#23252,#23253,#23254,#23255,#23256,#23257,#23258,#23259,#23260,#23261,
#23262,#23263,#23264,#23265,#23266,#23267,#23268),.UNSPECIFIED.,.F.,.F.)
B_SPLINE_CURVE_WITH_KNOTS((6,1,1,1,1,1,1,1,1,1,1,1,1,1,1,1,1,1,1,1,1,1,
1,1,1,1,1,1,1,1,1,1,1,1,1,1,1,1,1,1,1,1,1,1,1,1,1,1,1,1,1,1,1,1,1,1,1,1,
1,1,1,1,1,1,1,6),(0.,0.0153846153846154,0.0307692307692308,0.0461538461538462,
0.0615384615384615,0.0769230769230769,0.0923076923076923,0.107692307692308,
0.123076923076923,0.138461538461538,0.153846153846154,0.169230769230769,
0.184615384615385,0.2,0.215384615384615,0.230769230769231,0.246153846153846,
0.261538461538462,0.276923076923077,0.292307692307692,0.307692307692308,
0.323076923076923,0.338461538461538,0.353846153846154,0.369230769230769,
0.384615384615385,0.4,0.415384615384615,0.430769230769231,0.446153846153846,
0.461538461538462,0.476923076923077,0.492307692307692,0.507692307692308,
0.523076923076923,0.538461538461538,0.553846153846154,0.569230769230769,
0.584615384615384,0.6,0.615384615384615,0.63076923076923,0.646153846153846,
0.661538461538461,0.676923076923076,0.692307692307692,0.707692307692307,
0.723076923076922,0.738461538461538,0.753846153846153,0.769230769230768,
0.784615384615384,0.799999999999999,0.815384615384614,0.83076923076923,
0.846153846153845,0.86153846153846,0.876923076923076,0.892307692307691,
0.907692307692306,0.923076923076922,0.938461538461537,0.953846153846152,
0.969230769230768,0.984615384615383,1.),.UNSPECIFIED.)
CURVE()
GEOMETRIC_REPRESENTATION_ITEM()
RATIONAL_B_SPLINE_CURVE((1.,1.,1.,1.,1.,1.,1.,1.,1.,1.,1.,1.,1.,1.,1.,1.,
1.,1.,1.,1.,1.,1.,1.,1.,1.,1.,1.,1.,1.,1.,1.,1.,1.,1.,1.,1.,1.,1.,1.,1.,
1.,1.,1.,1.,1.,1.,1.,1.,1.,1.,1.,1.,1.,1.,1.,1.,1.,1.,1.,1.,1.,1.,1.,1.,
1.,1.,1.,1.,1.,1.))
REPRESENTATION_ITEM('')
);
#145=(
BOUNDED_CURVE()
B_SPLINE_CURVE(5,(#23272,#23273,#23274,#23275,#23276,#23277,#23278,#23279,
#23280,#23281,#23282,#23283,#23284,#23285,#23286,#23287,#23288,#23289,#23290,
#23291,#23292,#23293,#23294,#23295,#23296,#23297,#23298,#23299,#23300,#23301,
#23302,#23303,#23304,#23305,#23306,#23307,#23308,#23309,#23310,#23311,#23312,
#23313,#23314,#23315,#23316,#23317,#23318,#23319,#23320,#23321,#23322,#23323,
#23324,#23325,#23326,#23327,#23328,#23329,#23330,#23331,#23332,#23333,#23334,
#23335,#23336,#23337,#23338,#23339,#23340,#23341),.UNSPECIFIED.,.F.,.F.)
B_SPLINE_CURVE_WITH_KNOTS((6,1,1,1,1,1,1,1,1,1,1,1,1,1,1,1,1,1,1,1,1,1,
1,1,1,1,1,1,1,1,1,1,1,1,1,1,1,1,1,1,1,1,1,1,1,1,1,1,1,1,1,1,1,1,1,1,1,1,
1,1,1,1,1,1,1,6),(0.,0.0153846153846154,0.0307692307692308,0.0461538461538462,
0.0615384615384615,0.0769230769230769,0.0923076923076923,0.107692307692308,
0.123076923076923,0.138461538461538,0.153846153846154,0.169230769230769,
0.184615384615385,0.2,0.215384615384615,0.230769230769231,0.246153846153846,
0.261538461538462,0.276923076923077,0.292307692307692,0.307692307692308,
0.323076923076923,0.338461538461538,0.353846153846154,0.369230769230769,
0.384615384615385,0.4,0.415384615384615,0.430769230769231,0.446153846153846,
0.461538461538462,0.476923076923077,0.492307692307692,0.507692307692308,
0.523076923076923,0.538461538461538,0.553846153846154,0.569230769230769,
0.584615384615384,0.6,0.615384615384615,0.63076923076923,0.646153846153846,
0.661538461538461,0.676923076923076,0.692307692307692,0.707692307692307,
0.723076923076922,0.738461538461538,0.753846153846153,0.769230769230768,
0.784615384615384,0.799999999999999,0.815384615384614,0.83076923076923,
0.846153846153845,0.86153846153846,0.876923076923076,0.892307692307691,
0.907692307692306,0.923076923076922,0.938461538461537,0.953846153846152,
0.969230769230768,0.984615384615383,1.),.UNSPECIFIED.)
CURVE()
GEOMETRIC_REPRESENTATION_ITEM()
RATIONAL_B_SPLINE_CURVE((1.,1.,1.,1.,1.,1.,1.,1.,1.,1.,1.,1.,1.,1.,1.,1.,
1.,1.,1.,1.,1.,1.,1.,1.,1.,1.,1.,1.,1.,1.,1.,1.,1.,1.,1.,1.,1.,1.,1.,1.,
1.,1.,1.,1.,1.,1.,1.,1.,1.,1.,1.,1.,1.,1.,1.,1.,1.,1.,1.,1.,1.,1.,1.,1.,
1.,1.,1.,1.,1.,1.))
REPRESENTATION_ITEM('')
);
#146=(
BOUNDED_CURVE()
B_SPLINE_CURVE(5,(#23345,#23346,#23347,#23348,#23349,#23350,#23351,#23352,
#23353,#23354,#23355,#23356,#23357,#23358,#23359,#23360,#23361,#23362,#23363,
#23364,#23365,#23366,#23367,#23368,#23369,#23370,#23371,#23372,#23373,#23374,
#23375,#23376,#23377,#23378,#23379,#23380,#23381,#23382,#23383,#23384,#23385,
#23386,#23387,#23388,#23389,#23390,#23391,#23392,#23393,#23394,#23395,#23396,
#23397,#23398,#23399,#23400,#23401,#23402,#23403,#23404,#23405,#23406,#23407,
#23408,#23409,#23410,#23411,#23412,#23413,#23414),.UNSPECIFIED.,.F.,.F.)
B_SPLINE_CURVE_WITH_KNOTS((6,1,1,1,1,1,1,1,1,1,1,1,1,1,1,1,1,1,1,1,1,1,
1,1,1,1,1,1,1,1,1,1,1,1,1,1,1,1,1,1,1,1,1,1,1,1,1,1,1,1,1,1,1,1,1,1,1,1,
1,1,1,1,1,1,1,6),(0.,0.0153846153846154,0.0307692307692308,0.0461538461538462,
0.0615384615384615,0.0769230769230769,0.0923076923076923,0.107692307692308,
0.123076923076923,0.138461538461538,0.153846153846154,0.169230769230769,
0.184615384615385,0.2,0.215384615384615,0.230769230769231,0.246153846153846,
0.261538461538462,0.276923076923077,0.292307692307692,0.307692307692308,
0.323076923076923,0.338461538461538,0.353846153846154,0.369230769230769,
0.384615384615385,0.4,0.415384615384615,0.430769230769231,0.446153846153846,
0.461538461538462,0.476923076923077,0.492307692307692,0.507692307692308,
0.523076923076923,0.538461538461538,0.553846153846154,0.569230769230769,
0.584615384615384,0.6,0.615384615384615,0.63076923076923,0.646153846153846,
0.661538461538461,0.676923076923076,0.692307692307692,0.707692307692307,
0.723076923076922,0.738461538461538,0.753846153846153,0.769230769230768,
0.784615384615384,0.799999999999999,0.815384615384614,0.83076923076923,
0.846153846153845,0.86153846153846,0.876923076923076,0.892307692307691,
0.907692307692306,0.923076923076922,0.938461538461537,0.953846153846152,
0.969230769230768,0.984615384615383,1.),.UNSPECIFIED.)
CURVE()
GEOMETRIC_REPRESENTATION_ITEM()
RATIONAL_B_SPLINE_CURVE((1.,1.,1.,1.,1.,1.,1.,1.,1.,1.,1.,1.,1.,1.,1.,1.,
1.,1.,1.,1.,1.,1.,1.,1.,1.,1.,1.,1.,1.,1.,1.,1.,1.,1.,1.,1.,1.,1.,1.,1.,
1.,1.,1.,1.,1.,1.,1.,1.,1.,1.,1.,1.,1.,1.,1.,1.,1.,1.,1.,1.,1.,1.,1.,1.,
1.,1.,1.,1.,1.,1.))
REPRESENTATION_ITEM('')
);
#147=(
BOUNDED_CURVE()
B_SPLINE_CURVE(5,(#23418,#23419,#23420,#23421,#23422,#23423,#23424,#23425,
#23426,#23427,#23428,#23429,#23430,#23431,#23432,#23433,#23434,#23435,#23436,
#23437,#23438,#23439,#23440,#23441,#23442,#23443,#23444,#23445,#23446,#23447,
#23448,#23449,#23450,#23451,#23452,#23453,#23454,#23455,#23456,#23457,#23458,
#23459,#23460,#23461,#23462,#23463,#23464,#23465,#23466,#23467,#23468,#23469,
#23470,#23471,#23472,#23473,#23474,#23475,#23476,#23477,#23478,#23479,#23480,
#23481,#23482,#23483,#23484,#23485,#23486,#23487),.UNSPECIFIED.,.F.,.F.)
B_SPLINE_CURVE_WITH_KNOTS((6,1,1,1,1,1,1,1,1,1,1,1,1,1,1,1,1,1,1,1,1,1,
1,1,1,1,1,1,1,1,1,1,1,1,1,1,1,1,1,1,1,1,1,1,1,1,1,1,1,1,1,1,1,1,1,1,1,1,
1,1,1,1,1,1,1,6),(0.,0.0153846153846154,0.0307692307692308,0.0461538461538462,
0.0615384615384615,0.0769230769230769,0.0923076923076923,0.107692307692308,
0.123076923076923,0.138461538461538,0.153846153846154,0.169230769230769,
0.184615384615385,0.2,0.215384615384615,0.230769230769231,0.246153846153846,
0.261538461538462,0.276923076923077,0.292307692307692,0.307692307692308,
0.323076923076923,0.338461538461538,0.353846153846154,0.369230769230769,
0.384615384615385,0.4,0.415384615384615,0.430769230769231,0.446153846153846,
0.461538461538462,0.476923076923077,0.492307692307692,0.507692307692308,
0.523076923076923,0.538461538461538,0.553846153846154,0.569230769230769,
0.584615384615384,0.6,0.615384615384615,0.63076923076923,0.646153846153846,
0.661538461538461,0.676923076923076,0.692307692307692,0.707692307692307,
0.723076923076922,0.738461538461538,0.753846153846153,0.769230769230768,
0.784615384615384,0.799999999999999,0.815384615384614,0.83076923076923,
0.846153846153845,0.86153846153846,0.876923076923076,0.892307692307691,
0.907692307692306,0.923076923076922,0.938461538461537,0.953846153846152,
0.969230769230768,0.984615384615383,1.),.UNSPECIFIED.)
CURVE()
GEOMETRIC_REPRESENTATION_ITEM()
RATIONAL_B_SPLINE_CURVE((1.,1.,1.,1.,1.,1.,1.,1.,1.,1.,1.,1.,1.,1.,1.,1.,
1.,1.,1.,1.,1.,1.,1.,1.,1.,1.,1.,1.,1.,1.,1.,1.,1.,1.,1.,1.,1.,1.,1.,1.,
1.,1.,1.,1.,1.,1.,1.,1.,1.,1.,1.,1.,1.,1.,1.,1.,1.,1.,1.,1.,1.,1.,1.,1.,
1.,1.,1.,1.,1.,1.))
REPRESENTATION_ITEM('')
);
#148=(
BOUNDED_CURVE()
B_SPLINE_CURVE(5,(#23491,#23492,#23493,#23494,#23495,#23496,#23497,#23498,
#23499,#23500,#23501,#23502,#23503,#23504,#23505,#23506,#23507,#23508,#23509,
#23510,#23511,#23512,#23513,#23514,#23515,#23516,#23517,#23518,#23519,#23520,
#23521,#23522,#23523,#23524,#23525,#23526,#23527,#23528,#23529,#23530,#23531,
#23532,#23533,#23534,#23535,#23536,#23537,#23538,#23539,#23540,#23541,#23542,
#23543,#23544,#23545,#23546,#23547,#23548,#23549,#23550,#23551,#23552,#23553,
#23554,#23555,#23556,#23557,#23558,#23559,#23560),.UNSPECIFIED.,.F.,.F.)
B_SPLINE_CURVE_WITH_KNOTS((6,1,1,1,1,1,1,1,1,1,1,1,1,1,1,1,1,1,1,1,1,1,
1,1,1,1,1,1,1,1,1,1,1,1,1,1,1,1,1,1,1,1,1,1,1,1,1,1,1,1,1,1,1,1,1,1,1,1,
1,1,1,1,1,1,1,6),(0.,0.0153846153846154,0.0307692307692308,0.0461538461538462,
0.0615384615384615,0.0769230769230769,0.0923076923076923,0.107692307692308,
0.123076923076923,0.138461538461538,0.153846153846154,0.169230769230769,
0.184615384615385,0.2,0.215384615384615,0.230769230769231,0.246153846153846,
0.261538461538462,0.276923076923077,0.292307692307692,0.307692307692308,
0.323076923076923,0.338461538461538,0.353846153846154,0.369230769230769,
0.384615384615385,0.4,0.415384615384615,0.430769230769231,0.446153846153846,
0.461538461538462,0.476923076923077,0.492307692307692,0.507692307692308,
0.523076923076923,0.538461538461538,0.553846153846154,0.569230769230769,
0.584615384615384,0.6,0.615384615384615,0.63076923076923,0.646153846153846,
0.661538461538461,0.676923076923076,0.692307692307692,0.707692307692307,
0.723076923076922,0.738461538461538,0.753846153846153,0.769230769230768,
0.784615384615384,0.799999999999999,0.815384615384614,0.83076923076923,
0.846153846153845,0.86153846153846,0.876923076923076,0.892307692307691,
0.907692307692306,0.923076923076922,0.938461538461537,0.953846153846152,
0.969230769230768,0.984615384615383,1.),.UNSPECIFIED.)
CURVE()
GEOMETRIC_REPRESENTATION_ITEM()
RATIONAL_B_SPLINE_CURVE((1.,1.,1.,1.,1.,1.,1.,1.,1.,1.,1.,1.,1.,1.,1.,1.,
1.,1.,1.,1.,1.,1.,1.,1.,1.,1.,1.,1.,1.,1.,1.,1.,1.,1.,1.,1.,1.,1.,1.,1.,
1.,1.,1.,1.,1.,1.,1.,1.,1.,1.,1.,1.,1.,1.,1.,1.,1.,1.,1.,1.,1.,1.,1.,1.,
1.,1.,1.,1.,1.,1.))
REPRESENTATION_ITEM('')
);
#149=(
BOUNDED_CURVE()
B_SPLINE_CURVE(5,(#23564,#23565,#23566,#23567,#23568,#23569,#23570,#23571,
#23572,#23573,#23574,#23575,#23576,#23577,#23578,#23579,#23580,#23581,#23582,
#23583,#23584,#23585,#23586,#23587,#23588,#23589,#23590,#23591,#23592,#23593,
#23594,#23595,#23596,#23597,#23598,#23599,#23600,#23601,#23602,#23603,#23604,
#23605,#23606,#23607,#23608,#23609,#23610,#23611,#23612,#23613,#23614,#23615,
#23616,#23617,#23618,#23619,#23620,#23621,#23622,#23623,#23624,#23625,#23626,
#23627,#23628,#23629,#23630,#23631,#23632,#23633),.UNSPECIFIED.,.F.,.F.)
B_SPLINE_CURVE_WITH_KNOTS((6,1,1,1,1,1,1,1,1,1,1,1,1,1,1,1,1,1,1,1,1,1,
1,1,1,1,1,1,1,1,1,1,1,1,1,1,1,1,1,1,1,1,1,1,1,1,1,1,1,1,1,1,1,1,1,1,1,1,
1,1,1,1,1,1,1,6),(0.,0.0153846153846154,0.0307692307692308,0.0461538461538462,
0.0615384615384615,0.0769230769230769,0.0923076923076923,0.107692307692308,
0.123076923076923,0.138461538461538,0.153846153846154,0.169230769230769,
0.184615384615385,0.2,0.215384615384615,0.230769230769231,0.246153846153846,
0.261538461538462,0.276923076923077,0.292307692307692,0.307692307692308,
0.323076923076923,0.338461538461538,0.353846153846154,0.369230769230769,
0.384615384615385,0.4,0.415384615384615,0.430769230769231,0.446153846153846,
0.461538461538462,0.476923076923077,0.492307692307692,0.507692307692308,
0.523076923076923,0.538461538461538,0.553846153846154,0.569230769230769,
0.584615384615384,0.6,0.615384615384615,0.63076923076923,0.646153846153846,
0.661538461538461,0.676923076923076,0.692307692307692,0.707692307692307,
0.723076923076922,0.738461538461538,0.753846153846153,0.769230769230768,
0.784615384615384,0.799999999999999,0.815384615384614,0.83076923076923,
0.846153846153845,0.86153846153846,0.876923076923076,0.892307692307691,
0.907692307692306,0.923076923076922,0.938461538461537,0.953846153846152,
0.969230769230768,0.984615384615383,1.),.UNSPECIFIED.)
CURVE()
GEOMETRIC_REPRESENTATION_ITEM()
RATIONAL_B_SPLINE_CURVE((1.,1.,1.,1.,1.,1.,1.,1.,1.,1.,1.,1.,1.,1.,1.,1.,
1.,1.,1.,1.,1.,1.,1.,1.,1.,1.,1.,1.,1.,1.,1.,1.,1.,1.,1.,1.,1.,1.,1.,1.,
1.,1.,1.,1.,1.,1.,1.,1.,1.,1.,1.,1.,1.,1.,1.,1.,1.,1.,1.,1.,1.,1.,1.,1.,
1.,1.,1.,1.,1.,1.))
REPRESENTATION_ITEM('')
);
#150=(
BOUNDED_CURVE()
B_SPLINE_CURVE(5,(#23637,#23638,#23639,#23640,#23641,#23642,#23643,#23644,
#23645,#23646,#23647,#23648,#23649,#23650,#23651,#23652,#23653,#23654,#23655,
#23656,#23657,#23658,#23659,#23660,#23661,#23662,#23663,#23664,#23665,#23666,
#23667,#23668,#23669,#23670,#23671,#23672,#23673,#23674,#23675,#23676,#23677,
#23678,#23679,#23680,#23681,#23682,#23683,#23684,#23685,#23686,#23687,#23688,
#23689,#23690,#23691,#23692,#23693,#23694,#23695,#23696,#23697,#23698,#23699,
#23700,#23701,#23702,#23703,#23704,#23705,#23706),.UNSPECIFIED.,.F.,.F.)
B_SPLINE_CURVE_WITH_KNOTS((6,1,1,1,1,1,1,1,1,1,1,1,1,1,1,1,1,1,1,1,1,1,
1,1,1,1,1,1,1,1,1,1,1,1,1,1,1,1,1,1,1,1,1,1,1,1,1,1,1,1,1,1,1,1,1,1,1,1,
1,1,1,1,1,1,1,6),(0.,0.0153846153846154,0.0307692307692308,0.0461538461538462,
0.0615384615384615,0.0769230769230769,0.0923076923076923,0.107692307692308,
0.123076923076923,0.138461538461538,0.153846153846154,0.169230769230769,
0.184615384615385,0.2,0.215384615384615,0.230769230769231,0.246153846153846,
0.261538461538462,0.276923076923077,0.292307692307692,0.307692307692308,
0.323076923076923,0.338461538461538,0.353846153846154,0.369230769230769,
0.384615384615385,0.4,0.415384615384615,0.430769230769231,0.446153846153846,
0.461538461538462,0.476923076923077,0.492307692307692,0.507692307692308,
0.523076923076923,0.538461538461538,0.553846153846154,0.569230769230769,
0.584615384615384,0.6,0.615384615384615,0.63076923076923,0.646153846153846,
0.661538461538461,0.676923076923076,0.692307692307692,0.707692307692307,
0.723076923076922,0.738461538461538,0.753846153846153,0.769230769230768,
0.784615384615384,0.799999999999999,0.815384615384614,0.83076923076923,
0.846153846153845,0.86153846153846,0.876923076923076,0.892307692307691,
0.907692307692306,0.923076923076922,0.938461538461537,0.953846153846152,
0.969230769230768,0.984615384615383,1.),.UNSPECIFIED.)
CURVE()
GEOMETRIC_REPRESENTATION_ITEM()
RATIONAL_B_SPLINE_CURVE((1.,1.,1.,1.,1.,1.,1.,1.,1.,1.,1.,1.,1.,1.,1.,1.,
1.,1.,1.,1.,1.,1.,1.,1.,1.,1.,1.,1.,1.,1.,1.,1.,1.,1.,1.,1.,1.,1.,1.,1.,
1.,1.,1.,1.,1.,1.,1.,1.,1.,1.,1.,1.,1.,1.,1.,1.,1.,1.,1.,1.,1.,1.,1.,1.,
1.,1.,1.,1.,1.,1.))
REPRESENTATION_ITEM('')
);
#151=(
BOUNDED_CURVE()
B_SPLINE_CURVE(5,(#23710,#23711,#23712,#23713,#23714,#23715,#23716,#23717,
#23718,#23719,#23720,#23721,#23722,#23723,#23724,#23725,#23726,#23727,#23728,
#23729,#23730,#23731,#23732,#23733,#23734,#23735,#23736,#23737,#23738,#23739,
#23740,#23741,#23742,#23743,#23744,#23745,#23746,#23747,#23748,#23749,#23750,
#23751,#23752,#23753,#23754,#23755,#23756,#23757,#23758,#23759,#23760,#23761,
#23762,#23763,#23764,#23765,#23766,#23767,#23768,#23769,#23770,#23771,#23772,
#23773,#23774,#23775,#23776,#23777,#23778,#23779),.UNSPECIFIED.,.F.,.F.)
B_SPLINE_CURVE_WITH_KNOTS((6,1,1,1,1,1,1,1,1,1,1,1,1,1,1,1,1,1,1,1,1,1,
1,1,1,1,1,1,1,1,1,1,1,1,1,1,1,1,1,1,1,1,1,1,1,1,1,1,1,1,1,1,1,1,1,1,1,1,
1,1,1,1,1,1,1,6),(0.,0.0153846153846154,0.0307692307692308,0.0461538461538462,
0.0615384615384615,0.0769230769230769,0.0923076923076923,0.107692307692308,
0.123076923076923,0.138461538461538,0.153846153846154,0.169230769230769,
0.184615384615385,0.2,0.215384615384615,0.230769230769231,0.246153846153846,
0.261538461538462,0.276923076923077,0.292307692307692,0.307692307692308,
0.323076923076923,0.338461538461538,0.353846153846154,0.369230769230769,
0.384615384615385,0.4,0.415384615384615,0.430769230769231,0.446153846153846,
0.461538461538462,0.476923076923077,0.492307692307692,0.507692307692308,
0.523076923076923,0.538461538461538,0.553846153846154,0.569230769230769,
0.584615384615384,0.6,0.615384615384615,0.63076923076923,0.646153846153846,
0.661538461538461,0.676923076923076,0.692307692307692,0.707692307692307,
0.723076923076922,0.738461538461538,0.753846153846153,0.769230769230768,
0.784615384615384,0.799999999999999,0.815384615384614,0.83076923076923,
0.846153846153845,0.86153846153846,0.876923076923076,0.892307692307691,
0.907692307692306,0.923076923076922,0.938461538461537,0.953846153846152,
0.969230769230768,0.984615384615383,1.),.UNSPECIFIED.)
CURVE()
GEOMETRIC_REPRESENTATION_ITEM()
RATIONAL_B_SPLINE_CURVE((1.,1.,1.,1.,1.,1.,1.,1.,1.,1.,1.,1.,1.,1.,1.,1.,
1.,1.,1.,1.,1.,1.,1.,1.,1.,1.,1.,1.,1.,1.,1.,1.,1.,1.,1.,1.,1.,1.,1.,1.,
1.,1.,1.,1.,1.,1.,1.,1.,1.,1.,1.,1.,1.,1.,1.,1.,1.,1.,1.,1.,1.,1.,1.,1.,
1.,1.,1.,1.,1.,1.))
REPRESENTATION_ITEM('')
);
#152=(
BOUNDED_CURVE()
B_SPLINE_CURVE(5,(#23783,#23784,#23785,#23786,#23787,#23788,#23789,#23790,
#23791,#23792,#23793,#23794,#23795,#23796,#23797,#23798,#23799,#23800,#23801,
#23802,#23803,#23804,#23805,#23806,#23807,#23808,#23809,#23810,#23811,#23812,
#23813,#23814,#23815,#23816,#23817,#23818,#23819,#23820,#23821,#23822,#23823,
#23824,#23825,#23826,#23827,#23828,#23829,#23830,#23831,#23832,#23833,#23834,
#23835,#23836,#23837,#23838,#23839,#23840,#23841,#23842,#23843,#23844,#23845,
#23846,#23847,#23848,#23849,#23850,#23851,#23852),.UNSPECIFIED.,.F.,.F.)
B_SPLINE_CURVE_WITH_KNOTS((6,1,1,1,1,1,1,1,1,1,1,1,1,1,1,1,1,1,1,1,1,1,
1,1,1,1,1,1,1,1,1,1,1,1,1,1,1,1,1,1,1,1,1,1,1,1,1,1,1,1,1,1,1,1,1,1,1,1,
1,1,1,1,1,1,1,6),(0.,0.0153846153846154,0.0307692307692308,0.0461538461538462,
0.0615384615384615,0.0769230769230769,0.0923076923076923,0.107692307692308,
0.123076923076923,0.138461538461538,0.153846153846154,0.169230769230769,
0.184615384615385,0.2,0.215384615384615,0.230769230769231,0.246153846153846,
0.261538461538462,0.276923076923077,0.292307692307692,0.307692307692308,
0.323076923076923,0.338461538461538,0.353846153846154,0.369230769230769,
0.384615384615385,0.4,0.415384615384615,0.430769230769231,0.446153846153846,
0.461538461538462,0.476923076923077,0.492307692307692,0.507692307692308,
0.523076923076923,0.538461538461538,0.553846153846154,0.569230769230769,
0.584615384615384,0.6,0.615384615384615,0.63076923076923,0.646153846153846,
0.661538461538461,0.676923076923076,0.692307692307692,0.707692307692307,
0.723076923076922,0.738461538461538,0.753846153846153,0.769230769230768,
0.784615384615384,0.799999999999999,0.815384615384614,0.83076923076923,
0.846153846153845,0.86153846153846,0.876923076923076,0.892307692307691,
0.907692307692306,0.923076923076922,0.938461538461537,0.953846153846152,
0.969230769230768,0.984615384615383,1.),.UNSPECIFIED.)
CURVE()
GEOMETRIC_REPRESENTATION_ITEM()
RATIONAL_B_SPLINE_CURVE((1.,1.,1.,1.,1.,1.,1.,1.,1.,1.,1.,1.,1.,1.,1.,1.,
1.,1.,1.,1.,1.,1.,1.,1.,1.,1.,1.,1.,1.,1.,1.,1.,1.,1.,1.,1.,1.,1.,1.,1.,
1.,1.,1.,1.,1.,1.,1.,1.,1.,1.,1.,1.,1.,1.,1.,1.,1.,1.,1.,1.,1.,1.,1.,1.,
1.,1.,1.,1.,1.,1.))
REPRESENTATION_ITEM('')
);
#153=(
BOUNDED_CURVE()
B_SPLINE_CURVE(5,(#23856,#23857,#23858,#23859,#23860,#23861,#23862,#23863,
#23864,#23865,#23866,#23867,#23868,#23869,#23870,#23871,#23872,#23873,#23874,
#23875,#23876,#23877,#23878,#23879,#23880,#23881,#23882,#23883,#23884,#23885,
#23886,#23887,#23888,#23889,#23890,#23891,#23892,#23893,#23894,#23895,#23896,
#23897,#23898,#23899,#23900,#23901,#23902,#23903,#23904,#23905,#23906,#23907,
#23908,#23909,#23910,#23911,#23912,#23913,#23914,#23915,#23916,#23917,#23918,
#23919,#23920,#23921,#23922,#23923,#23924,#23925),.UNSPECIFIED.,.F.,.F.)
B_SPLINE_CURVE_WITH_KNOTS((6,1,1,1,1,1,1,1,1,1,1,1,1,1,1,1,1,1,1,1,1,1,
1,1,1,1,1,1,1,1,1,1,1,1,1,1,1,1,1,1,1,1,1,1,1,1,1,1,1,1,1,1,1,1,1,1,1,1,
1,1,1,1,1,1,1,6),(0.,0.0153846153846154,0.0307692307692308,0.0461538461538462,
0.0615384615384615,0.0769230769230769,0.0923076923076923,0.107692307692308,
0.123076923076923,0.138461538461538,0.153846153846154,0.169230769230769,
0.184615384615385,0.2,0.215384615384615,0.230769230769231,0.246153846153846,
0.261538461538462,0.276923076923077,0.292307692307692,0.307692307692308,
0.323076923076923,0.338461538461538,0.353846153846154,0.369230769230769,
0.384615384615385,0.4,0.415384615384615,0.430769230769231,0.446153846153846,
0.461538461538462,0.476923076923077,0.492307692307692,0.507692307692308,
0.523076923076923,0.538461538461538,0.553846153846154,0.569230769230769,
0.584615384615384,0.6,0.615384615384615,0.63076923076923,0.646153846153846,
0.661538461538461,0.676923076923076,0.692307692307692,0.707692307692307,
0.723076923076922,0.738461538461538,0.753846153846153,0.769230769230768,
0.784615384615384,0.799999999999999,0.815384615384614,0.83076923076923,
0.846153846153845,0.86153846153846,0.876923076923076,0.892307692307691,
0.907692307692306,0.923076923076922,0.938461538461537,0.953846153846152,
0.969230769230768,0.984615384615383,1.),.UNSPECIFIED.)
CURVE()
GEOMETRIC_REPRESENTATION_ITEM()
RATIONAL_B_SPLINE_CURVE((1.,1.,1.,1.,1.,1.,1.,1.,1.,1.,1.,1.,1.,1.,1.,1.,
1.,1.,1.,1.,1.,1.,1.,1.,1.,1.,1.,1.,1.,1.,1.,1.,1.,1.,1.,1.,1.,1.,1.,1.,
1.,1.,1.,1.,1.,1.,1.,1.,1.,1.,1.,1.,1.,1.,1.,1.,1.,1.,1.,1.,1.,1.,1.,1.,
1.,1.,1.,1.,1.,1.))
REPRESENTATION_ITEM('')
);
#154=(
BOUNDED_CURVE()
B_SPLINE_CURVE(5,(#23929,#23930,#23931,#23932,#23933,#23934,#23935,#23936,
#23937,#23938,#23939,#23940,#23941,#23942,#23943,#23944,#23945,#23946,#23947,
#23948,#23949,#23950,#23951,#23952,#23953,#23954,#23955,#23956,#23957,#23958,
#23959,#23960,#23961,#23962,#23963,#23964,#23965,#23966,#23967,#23968,#23969,
#23970,#23971,#23972,#23973,#23974,#23975,#23976,#23977,#23978,#23979,#23980,
#23981,#23982,#23983,#23984,#23985,#23986,#23987,#23988,#23989,#23990,#23991,
#23992,#23993,#23994,#23995,#23996,#23997,#23998),.UNSPECIFIED.,.F.,.F.)
B_SPLINE_CURVE_WITH_KNOTS((6,1,1,1,1,1,1,1,1,1,1,1,1,1,1,1,1,1,1,1,1,1,
1,1,1,1,1,1,1,1,1,1,1,1,1,1,1,1,1,1,1,1,1,1,1,1,1,1,1,1,1,1,1,1,1,1,1,1,
1,1,1,1,1,1,1,6),(0.,0.0153846153846154,0.0307692307692308,0.0461538461538462,
0.0615384615384615,0.0769230769230769,0.0923076923076923,0.107692307692308,
0.123076923076923,0.138461538461538,0.153846153846154,0.169230769230769,
0.184615384615385,0.2,0.215384615384615,0.230769230769231,0.246153846153846,
0.261538461538462,0.276923076923077,0.292307692307692,0.307692307692308,
0.323076923076923,0.338461538461538,0.353846153846154,0.369230769230769,
0.384615384615385,0.4,0.415384615384615,0.430769230769231,0.446153846153846,
0.461538461538462,0.476923076923077,0.492307692307692,0.507692307692308,
0.523076923076923,0.538461538461538,0.553846153846154,0.569230769230769,
0.584615384615384,0.6,0.615384615384615,0.63076923076923,0.646153846153846,
0.661538461538461,0.676923076923076,0.692307692307692,0.707692307692307,
0.723076923076922,0.738461538461538,0.753846153846153,0.769230769230768,
0.784615384615384,0.799999999999999,0.815384615384614,0.83076923076923,
0.846153846153845,0.86153846153846,0.876923076923076,0.892307692307691,
0.907692307692306,0.923076923076922,0.938461538461537,0.953846153846152,
0.969230769230768,0.984615384615383,1.),.UNSPECIFIED.)
CURVE()
GEOMETRIC_REPRESENTATION_ITEM()
RATIONAL_B_SPLINE_CURVE((1.,1.,1.,1.,1.,1.,1.,1.,1.,1.,1.,1.,1.,1.,1.,1.,
1.,1.,1.,1.,1.,1.,1.,1.,1.,1.,1.,1.,1.,1.,1.,1.,1.,1.,1.,1.,1.,1.,1.,1.,
1.,1.,1.,1.,1.,1.,1.,1.,1.,1.,1.,1.,1.,1.,1.,1.,1.,1.,1.,1.,1.,1.,1.,1.,
1.,1.,1.,1.,1.,1.))
REPRESENTATION_ITEM('')
);
#155=(
BOUNDED_CURVE()
B_SPLINE_CURVE(5,(#24002,#24003,#24004,#24005,#24006,#24007,#24008,#24009,
#24010,#24011,#24012,#24013,#24014,#24015,#24016,#24017,#24018,#24019,#24020,
#24021,#24022,#24023,#24024,#24025,#24026,#24027,#24028,#24029,#24030,#24031,
#24032,#24033,#24034,#24035,#24036,#24037,#24038,#24039,#24040,#24041,#24042,
#24043,#24044,#24045,#24046,#24047,#24048,#24049,#24050,#24051,#24052,#24053,
#24054,#24055,#24056,#24057,#24058,#24059,#24060,#24061,#24062,#24063,#24064,
#24065,#24066,#24067,#24068,#24069,#24070,#24071),.UNSPECIFIED.,.F.,.F.)
B_SPLINE_CURVE_WITH_KNOTS((6,1,1,1,1,1,1,1,1,1,1,1,1,1,1,1,1,1,1,1,1,1,
1,1,1,1,1,1,1,1,1,1,1,1,1,1,1,1,1,1,1,1,1,1,1,1,1,1,1,1,1,1,1,1,1,1,1,1,
1,1,1,1,1,1,1,6),(0.,0.0153846153846154,0.0307692307692308,0.0461538461538462,
0.0615384615384615,0.0769230769230769,0.0923076923076923,0.107692307692308,
0.123076923076923,0.138461538461538,0.153846153846154,0.169230769230769,
0.184615384615385,0.2,0.215384615384615,0.230769230769231,0.246153846153846,
0.261538461538462,0.276923076923077,0.292307692307692,0.307692307692308,
0.323076923076923,0.338461538461538,0.353846153846154,0.369230769230769,
0.384615384615385,0.4,0.415384615384615,0.430769230769231,0.446153846153846,
0.461538461538462,0.476923076923077,0.492307692307692,0.507692307692308,
0.523076923076923,0.538461538461538,0.553846153846154,0.569230769230769,
0.584615384615384,0.6,0.615384615384615,0.63076923076923,0.646153846153846,
0.661538461538461,0.676923076923076,0.692307692307692,0.707692307692307,
0.723076923076922,0.738461538461538,0.753846153846153,0.769230769230768,
0.784615384615384,0.799999999999999,0.815384615384614,0.83076923076923,
0.846153846153845,0.86153846153846,0.876923076923076,0.892307692307691,
0.907692307692306,0.923076923076922,0.938461538461537,0.953846153846152,
0.969230769230768,0.984615384615383,1.),.UNSPECIFIED.)
CURVE()
GEOMETRIC_REPRESENTATION_ITEM()
RATIONAL_B_SPLINE_CURVE((1.,1.,1.,1.,1.,1.,1.,1.,1.,1.,1.,1.,1.,1.,1.,1.,
1.,1.,1.,1.,1.,1.,1.,1.,1.,1.,1.,1.,1.,1.,1.,1.,1.,1.,1.,1.,1.,1.,1.,1.,
1.,1.,1.,1.,1.,1.,1.,1.,1.,1.,1.,1.,1.,1.,1.,1.,1.,1.,1.,1.,1.,1.,1.,1.,
1.,1.,1.,1.,1.,1.))
REPRESENTATION_ITEM('')
);
#156=(
BOUNDED_CURVE()
B_SPLINE_CURVE(5,(#24075,#24076,#24077,#24078,#24079,#24080,#24081,#24082,
#24083,#24084,#24085,#24086,#24087,#24088,#24089,#24090,#24091,#24092,#24093,
#24094,#24095,#24096,#24097,#24098,#24099,#24100,#24101,#24102,#24103,#24104,
#24105,#24106,#24107,#24108,#24109,#24110,#24111,#24112,#24113,#24114,#24115,
#24116,#24117,#24118,#24119,#24120,#24121,#24122,#24123,#24124,#24125,#24126,
#24127,#24128,#24129,#24130,#24131,#24132,#24133,#24134,#24135,#24136,#24137,
#24138,#24139,#24140,#24141,#24142,#24143,#24144),.UNSPECIFIED.,.F.,.F.)
B_SPLINE_CURVE_WITH_KNOTS((6,1,1,1,1,1,1,1,1,1,1,1,1,1,1,1,1,1,1,1,1,1,
1,1,1,1,1,1,1,1,1,1,1,1,1,1,1,1,1,1,1,1,1,1,1,1,1,1,1,1,1,1,1,1,1,1,1,1,
1,1,1,1,1,1,1,6),(0.,0.0153846153846154,0.0307692307692308,0.0461538461538462,
0.0615384615384615,0.0769230769230769,0.0923076923076923,0.107692307692308,
0.123076923076923,0.138461538461538,0.153846153846154,0.169230769230769,
0.184615384615385,0.2,0.215384615384615,0.230769230769231,0.246153846153846,
0.261538461538462,0.276923076923077,0.292307692307692,0.307692307692308,
0.323076923076923,0.338461538461538,0.353846153846154,0.369230769230769,
0.384615384615385,0.4,0.415384615384615,0.430769230769231,0.446153846153846,
0.461538461538462,0.476923076923077,0.492307692307692,0.507692307692308,
0.523076923076923,0.538461538461538,0.553846153846154,0.569230769230769,
0.584615384615384,0.6,0.615384615384615,0.63076923076923,0.646153846153846,
0.661538461538461,0.676923076923076,0.692307692307692,0.707692307692307,
0.723076923076922,0.738461538461538,0.753846153846153,0.769230769230768,
0.784615384615384,0.799999999999999,0.815384615384614,0.83076923076923,
0.846153846153845,0.86153846153846,0.876923076923076,0.892307692307691,
0.907692307692306,0.923076923076922,0.938461538461537,0.953846153846152,
0.969230769230768,0.984615384615383,1.),.UNSPECIFIED.)
CURVE()
GEOMETRIC_REPRESENTATION_ITEM()
RATIONAL_B_SPLINE_CURVE((1.,1.,1.,1.,1.,1.,1.,1.,1.,1.,1.,1.,1.,1.,1.,1.,
1.,1.,1.,1.,1.,1.,1.,1.,1.,1.,1.,1.,1.,1.,1.,1.,1.,1.,1.,1.,1.,1.,1.,1.,
1.,1.,1.,1.,1.,1.,1.,1.,1.,1.,1.,1.,1.,1.,1.,1.,1.,1.,1.,1.,1.,1.,1.,1.,
1.,1.,1.,1.,1.,1.))
REPRESENTATION_ITEM('')
);
#157=(
BOUNDED_CURVE()
B_SPLINE_CURVE(5,(#24148,#24149,#24150,#24151,#24152,#24153,#24154,#24155,
#24156,#24157,#24158,#24159,#24160,#24161,#24162,#24163,#24164,#24165,#24166,
#24167,#24168,#24169,#24170,#24171,#24172,#24173,#24174,#24175,#24176,#24177,
#24178,#24179,#24180,#24181,#24182,#24183,#24184,#24185,#24186,#24187,#24188,
#24189,#24190,#24191,#24192,#24193,#24194,#24195,#24196,#24197,#24198,#24199,
#24200,#24201,#24202,#24203,#24204,#24205,#24206,#24207,#24208,#24209,#24210,
#24211,#24212,#24213,#24214,#24215,#24216,#24217),.UNSPECIFIED.,.F.,.F.)
B_SPLINE_CURVE_WITH_KNOTS((6,1,1,1,1,1,1,1,1,1,1,1,1,1,1,1,1,1,1,1,1,1,
1,1,1,1,1,1,1,1,1,1,1,1,1,1,1,1,1,1,1,1,1,1,1,1,1,1,1,1,1,1,1,1,1,1,1,1,
1,1,1,1,1,1,1,6),(0.,0.0153846153846154,0.0307692307692308,0.0461538461538462,
0.0615384615384615,0.0769230769230769,0.0923076923076923,0.107692307692308,
0.123076923076923,0.138461538461538,0.153846153846154,0.169230769230769,
0.184615384615385,0.2,0.215384615384615,0.230769230769231,0.246153846153846,
0.261538461538462,0.276923076923077,0.292307692307692,0.307692307692308,
0.323076923076923,0.338461538461538,0.353846153846154,0.369230769230769,
0.384615384615385,0.4,0.415384615384615,0.430769230769231,0.446153846153846,
0.461538461538462,0.476923076923077,0.492307692307692,0.507692307692308,
0.523076923076923,0.538461538461538,0.553846153846154,0.569230769230769,
0.584615384615384,0.6,0.615384615384615,0.63076923076923,0.646153846153846,
0.661538461538461,0.676923076923076,0.692307692307692,0.707692307692307,
0.723076923076922,0.738461538461538,0.753846153846153,0.769230769230768,
0.784615384615384,0.799999999999999,0.815384615384614,0.83076923076923,
0.846153846153845,0.86153846153846,0.876923076923076,0.892307692307691,
0.907692307692306,0.923076923076922,0.938461538461537,0.953846153846152,
0.969230769230768,0.984615384615383,1.),.UNSPECIFIED.)
CURVE()
GEOMETRIC_REPRESENTATION_ITEM()
RATIONAL_B_SPLINE_CURVE((1.,1.,1.,1.,1.,1.,1.,1.,1.,1.,1.,1.,1.,1.,1.,1.,
1.,1.,1.,1.,1.,1.,1.,1.,1.,1.,1.,1.,1.,1.,1.,1.,1.,1.,1.,1.,1.,1.,1.,1.,
1.,1.,1.,1.,1.,1.,1.,1.,1.,1.,1.,1.,1.,1.,1.,1.,1.,1.,1.,1.,1.,1.,1.,1.,
1.,1.,1.,1.,1.,1.))
REPRESENTATION_ITEM('')
);
#158=(
BOUNDED_CURVE()
B_SPLINE_CURVE(5,(#24221,#24222,#24223,#24224,#24225,#24226,#24227,#24228,
#24229,#24230,#24231,#24232,#24233,#24234,#24235,#24236,#24237,#24238,#24239,
#24240,#24241,#24242,#24243,#24244,#24245,#24246,#24247,#24248,#24249,#24250,
#24251,#24252,#24253,#24254,#24255,#24256,#24257,#24258,#24259,#24260,#24261,
#24262,#24263,#24264,#24265,#24266,#24267,#24268,#24269,#24270,#24271,#24272,
#24273,#24274,#24275,#24276,#24277,#24278,#24279,#24280,#24281,#24282,#24283,
#24284,#24285,#24286,#24287,#24288,#24289,#24290),.UNSPECIFIED.,.F.,.F.)
B_SPLINE_CURVE_WITH_KNOTS((6,1,1,1,1,1,1,1,1,1,1,1,1,1,1,1,1,1,1,1,1,1,
1,1,1,1,1,1,1,1,1,1,1,1,1,1,1,1,1,1,1,1,1,1,1,1,1,1,1,1,1,1,1,1,1,1,1,1,
1,1,1,1,1,1,1,6),(0.,0.0153846153846154,0.0307692307692308,0.0461538461538462,
0.0615384615384615,0.0769230769230769,0.0923076923076923,0.107692307692308,
0.123076923076923,0.138461538461538,0.153846153846154,0.169230769230769,
0.184615384615385,0.2,0.215384615384615,0.230769230769231,0.246153846153846,
0.261538461538462,0.276923076923077,0.292307692307692,0.307692307692308,
0.323076923076923,0.338461538461538,0.353846153846154,0.369230769230769,
0.384615384615385,0.4,0.415384615384615,0.430769230769231,0.446153846153846,
0.461538461538462,0.476923076923077,0.492307692307692,0.507692307692308,
0.523076923076923,0.538461538461538,0.553846153846154,0.569230769230769,
0.584615384615384,0.6,0.615384615384615,0.63076923076923,0.646153846153846,
0.661538461538461,0.676923076923076,0.692307692307692,0.707692307692307,
0.723076923076922,0.738461538461538,0.753846153846153,0.769230769230768,
0.784615384615384,0.799999999999999,0.815384615384614,0.83076923076923,
0.846153846153845,0.86153846153846,0.876923076923076,0.892307692307691,
0.907692307692306,0.923076923076922,0.938461538461537,0.953846153846152,
0.969230769230768,0.984615384615383,1.),.UNSPECIFIED.)
CURVE()
GEOMETRIC_REPRESENTATION_ITEM()
RATIONAL_B_SPLINE_CURVE((1.,1.,1.,1.,1.,1.,1.,1.,1.,1.,1.,1.,1.,1.,1.,1.,
1.,1.,1.,1.,1.,1.,1.,1.,1.,1.,1.,1.,1.,1.,1.,1.,1.,1.,1.,1.,1.,1.,1.,1.,
1.,1.,1.,1.,1.,1.,1.,1.,1.,1.,1.,1.,1.,1.,1.,1.,1.,1.,1.,1.,1.,1.,1.,1.,
1.,1.,1.,1.,1.,1.))
REPRESENTATION_ITEM('')
);
#159=(
BOUNDED_CURVE()
B_SPLINE_CURVE(5,(#24294,#24295,#24296,#24297,#24298,#24299,#24300,#24301,
#24302,#24303,#24304,#24305,#24306,#24307,#24308,#24309,#24310,#24311,#24312,
#24313,#24314,#24315,#24316,#24317,#24318,#24319,#24320,#24321,#24322,#24323,
#24324,#24325,#24326,#24327,#24328,#24329,#24330,#24331,#24332,#24333,#24334,
#24335,#24336,#24337,#24338,#24339,#24340,#24341,#24342,#24343,#24344,#24345,
#24346,#24347,#24348,#24349,#24350,#24351,#24352,#24353,#24354,#24355,#24356,
#24357,#24358,#24359,#24360,#24361,#24362,#24363),.UNSPECIFIED.,.F.,.F.)
B_SPLINE_CURVE_WITH_KNOTS((6,1,1,1,1,1,1,1,1,1,1,1,1,1,1,1,1,1,1,1,1,1,
1,1,1,1,1,1,1,1,1,1,1,1,1,1,1,1,1,1,1,1,1,1,1,1,1,1,1,1,1,1,1,1,1,1,1,1,
1,1,1,1,1,1,1,6),(0.,0.0153846153846154,0.0307692307692308,0.0461538461538462,
0.0615384615384615,0.0769230769230769,0.0923076923076923,0.107692307692308,
0.123076923076923,0.138461538461538,0.153846153846154,0.169230769230769,
0.184615384615385,0.2,0.215384615384615,0.230769230769231,0.246153846153846,
0.261538461538462,0.276923076923077,0.292307692307692,0.307692307692308,
0.323076923076923,0.338461538461538,0.353846153846154,0.369230769230769,
0.384615384615385,0.4,0.415384615384615,0.430769230769231,0.446153846153846,
0.461538461538462,0.476923076923077,0.492307692307692,0.507692307692308,
0.523076923076923,0.538461538461538,0.553846153846154,0.569230769230769,
0.584615384615384,0.6,0.615384615384615,0.63076923076923,0.646153846153846,
0.661538461538461,0.676923076923076,0.692307692307692,0.707692307692307,
0.723076923076922,0.738461538461538,0.753846153846153,0.769230769230768,
0.784615384615384,0.799999999999999,0.815384615384614,0.83076923076923,
0.846153846153845,0.86153846153846,0.876923076923076,0.892307692307691,
0.907692307692306,0.923076923076922,0.938461538461537,0.953846153846152,
0.969230769230768,0.984615384615383,1.),.UNSPECIFIED.)
CURVE()
GEOMETRIC_REPRESENTATION_ITEM()
RATIONAL_B_SPLINE_CURVE((1.,1.,1.,1.,1.,1.,1.,1.,1.,1.,1.,1.,1.,1.,1.,1.,
1.,1.,1.,1.,1.,1.,1.,1.,1.,1.,1.,1.,1.,1.,1.,1.,1.,1.,1.,1.,1.,1.,1.,1.,
1.,1.,1.,1.,1.,1.,1.,1.,1.,1.,1.,1.,1.,1.,1.,1.,1.,1.,1.,1.,1.,1.,1.,1.,
1.,1.,1.,1.,1.,1.))
REPRESENTATION_ITEM('')
);
#160=(
BOUNDED_CURVE()
B_SPLINE_CURVE(5,(#24367,#24368,#24369,#24370,#24371,#24372,#24373,#24374,
#24375,#24376,#24377,#24378,#24379,#24380,#24381,#24382,#24383,#24384,#24385,
#24386,#24387,#24388,#24389,#24390,#24391,#24392,#24393,#24394,#24395,#24396,
#24397,#24398,#24399,#24400,#24401,#24402,#24403,#24404,#24405,#24406,#24407,
#24408,#24409,#24410,#24411,#24412,#24413,#24414,#24415,#24416,#24417,#24418,
#24419,#24420,#24421,#24422,#24423,#24424,#24425,#24426,#24427,#24428,#24429,
#24430,#24431,#24432,#24433,#24434,#24435,#24436),.UNSPECIFIED.,.F.,.F.)
B_SPLINE_CURVE_WITH_KNOTS((6,1,1,1,1,1,1,1,1,1,1,1,1,1,1,1,1,1,1,1,1,1,
1,1,1,1,1,1,1,1,1,1,1,1,1,1,1,1,1,1,1,1,1,1,1,1,1,1,1,1,1,1,1,1,1,1,1,1,
1,1,1,1,1,1,1,6),(0.,0.0153846153846154,0.0307692307692308,0.0461538461538462,
0.0615384615384615,0.0769230769230769,0.0923076923076923,0.107692307692308,
0.123076923076923,0.138461538461538,0.153846153846154,0.169230769230769,
0.184615384615385,0.2,0.215384615384615,0.230769230769231,0.246153846153846,
0.261538461538462,0.276923076923077,0.292307692307692,0.307692307692308,
0.323076923076923,0.338461538461538,0.353846153846154,0.369230769230769,
0.384615384615385,0.4,0.415384615384615,0.430769230769231,0.446153846153846,
0.461538461538462,0.476923076923077,0.492307692307692,0.507692307692308,
0.523076923076923,0.538461538461538,0.553846153846154,0.569230769230769,
0.584615384615384,0.6,0.615384615384615,0.63076923076923,0.646153846153846,
0.661538461538461,0.676923076923076,0.692307692307692,0.707692307692307,
0.723076923076922,0.738461538461538,0.753846153846153,0.769230769230768,
0.784615384615384,0.799999999999999,0.815384615384614,0.83076923076923,
0.846153846153845,0.86153846153846,0.876923076923076,0.892307692307691,
0.907692307692306,0.923076923076922,0.938461538461537,0.953846153846152,
0.969230769230768,0.984615384615383,1.),.UNSPECIFIED.)
CURVE()
GEOMETRIC_REPRESENTATION_ITEM()
RATIONAL_B_SPLINE_CURVE((1.,1.,1.,1.,1.,1.,1.,1.,1.,1.,1.,1.,1.,1.,1.,1.,
1.,1.,1.,1.,1.,1.,1.,1.,1.,1.,1.,1.,1.,1.,1.,1.,1.,1.,1.,1.,1.,1.,1.,1.,
1.,1.,1.,1.,1.,1.,1.,1.,1.,1.,1.,1.,1.,1.,1.,1.,1.,1.,1.,1.,1.,1.,1.,1.,
1.,1.,1.,1.,1.,1.))
REPRESENTATION_ITEM('')
);
#161=(
BOUNDED_CURVE()
B_SPLINE_CURVE(5,(#24440,#24441,#24442,#24443,#24444,#24445,#24446,#24447,
#24448,#24449,#24450,#24451,#24452,#24453,#24454,#24455,#24456,#24457,#24458,
#24459,#24460,#24461,#24462,#24463,#24464,#24465,#24466,#24467,#24468,#24469,
#24470,#24471,#24472,#24473,#24474,#24475,#24476,#24477,#24478,#24479,#24480,
#24481,#24482,#24483,#24484,#24485,#24486,#24487,#24488,#24489,#24490,#24491,
#24492,#24493,#24494,#24495,#24496,#24497,#24498,#24499,#24500,#24501,#24502,
#24503,#24504,#24505,#24506,#24507,#24508,#24509),.UNSPECIFIED.,.F.,.F.)
B_SPLINE_CURVE_WITH_KNOTS((6,1,1,1,1,1,1,1,1,1,1,1,1,1,1,1,1,1,1,1,1,1,
1,1,1,1,1,1,1,1,1,1,1,1,1,1,1,1,1,1,1,1,1,1,1,1,1,1,1,1,1,1,1,1,1,1,1,1,
1,1,1,1,1,1,1,6),(0.,0.0153846153846154,0.0307692307692308,0.0461538461538462,
0.0615384615384615,0.0769230769230769,0.0923076923076923,0.107692307692308,
0.123076923076923,0.138461538461538,0.153846153846154,0.169230769230769,
0.184615384615385,0.2,0.215384615384615,0.230769230769231,0.246153846153846,
0.261538461538462,0.276923076923077,0.292307692307692,0.307692307692308,
0.323076923076923,0.338461538461538,0.353846153846154,0.369230769230769,
0.384615384615385,0.4,0.415384615384615,0.430769230769231,0.446153846153846,
0.461538461538462,0.476923076923077,0.492307692307692,0.507692307692308,
0.523076923076923,0.538461538461538,0.553846153846154,0.569230769230769,
0.584615384615384,0.6,0.615384615384615,0.63076923076923,0.646153846153846,
0.661538461538461,0.676923076923076,0.692307692307692,0.707692307692307,
0.723076923076922,0.738461538461538,0.753846153846153,0.769230769230768,
0.784615384615384,0.799999999999999,0.815384615384614,0.83076923076923,
0.846153846153845,0.86153846153846,0.876923076923076,0.892307692307691,
0.907692307692306,0.923076923076922,0.938461538461537,0.953846153846152,
0.969230769230768,0.984615384615383,1.),.UNSPECIFIED.)
CURVE()
GEOMETRIC_REPRESENTATION_ITEM()
RATIONAL_B_SPLINE_CURVE((1.,1.,1.,1.,1.,1.,1.,1.,1.,1.,1.,1.,1.,1.,1.,1.,
1.,1.,1.,1.,1.,1.,1.,1.,1.,1.,1.,1.,1.,1.,1.,1.,1.,1.,1.,1.,1.,1.,1.,1.,
1.,1.,1.,1.,1.,1.,1.,1.,1.,1.,1.,1.,1.,1.,1.,1.,1.,1.,1.,1.,1.,1.,1.,1.,
1.,1.,1.,1.,1.,1.))
REPRESENTATION_ITEM('')
);
#162=(
BOUNDED_CURVE()
B_SPLINE_CURVE(5,(#24513,#24514,#24515,#24516,#24517,#24518,#24519,#24520,
#24521,#24522,#24523,#24524,#24525,#24526,#24527,#24528,#24529,#24530,#24531,
#24532,#24533,#24534,#24535,#24536,#24537,#24538,#24539,#24540,#24541,#24542,
#24543,#24544,#24545,#24546,#24547,#24548,#24549,#24550,#24551,#24552,#24553,
#24554,#24555,#24556,#24557,#24558,#24559,#24560,#24561,#24562,#24563,#24564,
#24565,#24566,#24567,#24568,#24569,#24570,#24571,#24572,#24573,#24574,#24575,
#24576,#24577,#24578,#24579,#24580,#24581,#24582),.UNSPECIFIED.,.F.,.F.)
B_SPLINE_CURVE_WITH_KNOTS((6,1,1,1,1,1,1,1,1,1,1,1,1,1,1,1,1,1,1,1,1,1,
1,1,1,1,1,1,1,1,1,1,1,1,1,1,1,1,1,1,1,1,1,1,1,1,1,1,1,1,1,1,1,1,1,1,1,1,
1,1,1,1,1,1,1,6),(0.,0.0153846153846154,0.0307692307692308,0.0461538461538462,
0.0615384615384615,0.0769230769230769,0.0923076923076923,0.107692307692308,
0.123076923076923,0.138461538461538,0.153846153846154,0.169230769230769,
0.184615384615385,0.2,0.215384615384615,0.230769230769231,0.246153846153846,
0.261538461538462,0.276923076923077,0.292307692307692,0.307692307692308,
0.323076923076923,0.338461538461538,0.353846153846154,0.369230769230769,
0.384615384615385,0.4,0.415384615384615,0.430769230769231,0.446153846153846,
0.461538461538462,0.476923076923077,0.492307692307692,0.507692307692308,
0.523076923076923,0.538461538461538,0.553846153846154,0.569230769230769,
0.584615384615384,0.6,0.615384615384615,0.63076923076923,0.646153846153846,
0.661538461538461,0.676923076923076,0.692307692307692,0.707692307692307,
0.723076923076922,0.738461538461538,0.753846153846153,0.769230769230768,
0.784615384615384,0.799999999999999,0.815384615384614,0.83076923076923,
0.846153846153845,0.86153846153846,0.876923076923076,0.892307692307691,
0.907692307692306,0.923076923076922,0.938461538461537,0.953846153846152,
0.969230769230768,0.984615384615383,1.),.UNSPECIFIED.)
CURVE()
GEOMETRIC_REPRESENTATION_ITEM()
RATIONAL_B_SPLINE_CURVE((1.,1.,1.,1.,1.,1.,1.,1.,1.,1.,1.,1.,1.,1.,1.,1.,
1.,1.,1.,1.,1.,1.,1.,1.,1.,1.,1.,1.,1.,1.,1.,1.,1.,1.,1.,1.,1.,1.,1.,1.,
1.,1.,1.,1.,1.,1.,1.,1.,1.,1.,1.,1.,1.,1.,1.,1.,1.,1.,1.,1.,1.,1.,1.,1.,
1.,1.,1.,1.,1.,1.))
REPRESENTATION_ITEM('')
);
#163=(
BOUNDED_CURVE()
B_SPLINE_CURVE(5,(#24586,#24587,#24588,#24589,#24590,#24591,#24592,#24593,
#24594,#24595,#24596,#24597,#24598,#24599,#24600,#24601,#24602,#24603,#24604,
#24605,#24606,#24607,#24608,#24609,#24610,#24611,#24612,#24613,#24614,#24615,
#24616,#24617,#24618,#24619,#24620,#24621,#24622,#24623,#24624,#24625,#24626,
#24627,#24628,#24629,#24630,#24631,#24632,#24633,#24634,#24635,#24636,#24637,
#24638,#24639,#24640,#24641,#24642,#24643,#24644,#24645,#24646,#24647,#24648,
#24649,#24650,#24651,#24652,#24653,#24654,#24655),.UNSPECIFIED.,.F.,.F.)
B_SPLINE_CURVE_WITH_KNOTS((6,1,1,1,1,1,1,1,1,1,1,1,1,1,1,1,1,1,1,1,1,1,
1,1,1,1,1,1,1,1,1,1,1,1,1,1,1,1,1,1,1,1,1,1,1,1,1,1,1,1,1,1,1,1,1,1,1,1,
1,1,1,1,1,1,1,6),(0.,0.0153846153846154,0.0307692307692308,0.0461538461538462,
0.0615384615384615,0.0769230769230769,0.0923076923076923,0.107692307692308,
0.123076923076923,0.138461538461538,0.153846153846154,0.169230769230769,
0.184615384615385,0.2,0.215384615384615,0.230769230769231,0.246153846153846,
0.261538461538462,0.276923076923077,0.292307692307692,0.307692307692308,
0.323076923076923,0.338461538461538,0.353846153846154,0.369230769230769,
0.384615384615385,0.4,0.415384615384615,0.430769230769231,0.446153846153846,
0.461538461538462,0.476923076923077,0.492307692307692,0.507692307692308,
0.523076923076923,0.538461538461538,0.553846153846154,0.569230769230769,
0.584615384615384,0.6,0.615384615384615,0.63076923076923,0.646153846153846,
0.661538461538461,0.676923076923076,0.692307692307692,0.707692307692307,
0.723076923076922,0.738461538461538,0.753846153846153,0.769230769230768,
0.784615384615384,0.799999999999999,0.815384615384614,0.83076923076923,
0.846153846153845,0.86153846153846,0.876923076923076,0.892307692307691,
0.907692307692306,0.923076923076922,0.938461538461537,0.953846153846152,
0.969230769230768,0.984615384615383,1.),.UNSPECIFIED.)
CURVE()
GEOMETRIC_REPRESENTATION_ITEM()
RATIONAL_B_SPLINE_CURVE((1.,1.,1.,1.,1.,1.,1.,1.,1.,1.,1.,1.,1.,1.,1.,1.,
1.,1.,1.,1.,1.,1.,1.,1.,1.,1.,1.,1.,1.,1.,1.,1.,1.,1.,1.,1.,1.,1.,1.,1.,
1.,1.,1.,1.,1.,1.,1.,1.,1.,1.,1.,1.,1.,1.,1.,1.,1.,1.,1.,1.,1.,1.,1.,1.,
1.,1.,1.,1.,1.,1.))
REPRESENTATION_ITEM('')
);
#164=(
BOUNDED_CURVE()
B_SPLINE_CURVE(5,(#24659,#24660,#24661,#24662,#24663,#24664,#24665,#24666,
#24667,#24668,#24669,#24670,#24671,#24672,#24673,#24674,#24675,#24676,#24677,
#24678,#24679,#24680,#24681,#24682,#24683,#24684,#24685,#24686,#24687,#24688,
#24689,#24690,#24691,#24692,#24693,#24694,#24695,#24696,#24697,#24698,#24699,
#24700,#24701,#24702,#24703,#24704,#24705,#24706,#24707,#24708,#24709,#24710,
#24711,#24712,#24713,#24714,#24715,#24716,#24717,#24718,#24719,#24720,#24721,
#24722,#24723,#24724,#24725,#24726,#24727,#24728),.UNSPECIFIED.,.F.,.F.)
B_SPLINE_CURVE_WITH_KNOTS((6,1,1,1,1,1,1,1,1,1,1,1,1,1,1,1,1,1,1,1,1,1,
1,1,1,1,1,1,1,1,1,1,1,1,1,1,1,1,1,1,1,1,1,1,1,1,1,1,1,1,1,1,1,1,1,1,1,1,
1,1,1,1,1,1,1,6),(0.,0.0153846153846154,0.0307692307692308,0.0461538461538462,
0.0615384615384615,0.0769230769230769,0.0923076923076923,0.107692307692308,
0.123076923076923,0.138461538461538,0.153846153846154,0.169230769230769,
0.184615384615385,0.2,0.215384615384615,0.230769230769231,0.246153846153846,
0.261538461538462,0.276923076923077,0.292307692307692,0.307692307692308,
0.323076923076923,0.338461538461538,0.353846153846154,0.369230769230769,
0.384615384615385,0.4,0.415384615384615,0.430769230769231,0.446153846153846,
0.461538461538462,0.476923076923077,0.492307692307692,0.507692307692308,
0.523076923076923,0.538461538461538,0.553846153846154,0.569230769230769,
0.584615384615384,0.6,0.615384615384615,0.63076923076923,0.646153846153846,
0.661538461538461,0.676923076923076,0.692307692307692,0.707692307692307,
0.723076923076922,0.738461538461538,0.753846153846153,0.769230769230768,
0.784615384615384,0.799999999999999,0.815384615384614,0.83076923076923,
0.846153846153845,0.86153846153846,0.876923076923076,0.892307692307691,
0.907692307692306,0.923076923076922,0.938461538461537,0.953846153846152,
0.969230769230768,0.984615384615383,1.),.UNSPECIFIED.)
CURVE()
GEOMETRIC_REPRESENTATION_ITEM()
RATIONAL_B_SPLINE_CURVE((1.,1.,1.,1.,1.,1.,1.,1.,1.,1.,1.,1.,1.,1.,1.,1.,
1.,1.,1.,1.,1.,1.,1.,1.,1.,1.,1.,1.,1.,1.,1.,1.,1.,1.,1.,1.,1.,1.,1.,1.,
1.,1.,1.,1.,1.,1.,1.,1.,1.,1.,1.,1.,1.,1.,1.,1.,1.,1.,1.,1.,1.,1.,1.,1.,
1.,1.,1.,1.,1.,1.))
REPRESENTATION_ITEM('')
);
#165=(
BOUNDED_CURVE()
B_SPLINE_CURVE(5,(#24732,#24733,#24734,#24735,#24736,#24737,#24738,#24739,
#24740,#24741,#24742,#24743,#24744,#24745,#24746,#24747,#24748,#24749,#24750,
#24751,#24752,#24753,#24754,#24755,#24756,#24757,#24758,#24759,#24760,#24761,
#24762,#24763,#24764,#24765,#24766,#24767,#24768,#24769,#24770,#24771,#24772,
#24773,#24774,#24775,#24776,#24777,#24778,#24779,#24780,#24781,#24782,#24783,
#24784,#24785,#24786,#24787,#24788,#24789,#24790,#24791,#24792,#24793,#24794,
#24795,#24796,#24797,#24798,#24799,#24800,#24801),.UNSPECIFIED.,.F.,.F.)
B_SPLINE_CURVE_WITH_KNOTS((6,1,1,1,1,1,1,1,1,1,1,1,1,1,1,1,1,1,1,1,1,1,
1,1,1,1,1,1,1,1,1,1,1,1,1,1,1,1,1,1,1,1,1,1,1,1,1,1,1,1,1,1,1,1,1,1,1,1,
1,1,1,1,1,1,1,6),(0.,0.0153846153846154,0.0307692307692308,0.0461538461538462,
0.0615384615384615,0.0769230769230769,0.0923076923076923,0.107692307692308,
0.123076923076923,0.138461538461538,0.153846153846154,0.169230769230769,
0.184615384615385,0.2,0.215384615384615,0.230769230769231,0.246153846153846,
0.261538461538462,0.276923076923077,0.292307692307692,0.307692307692308,
0.323076923076923,0.338461538461538,0.353846153846154,0.369230769230769,
0.384615384615385,0.4,0.415384615384615,0.430769230769231,0.446153846153846,
0.461538461538462,0.476923076923077,0.492307692307692,0.507692307692308,
0.523076923076923,0.538461538461538,0.553846153846154,0.569230769230769,
0.584615384615384,0.6,0.615384615384615,0.63076923076923,0.646153846153846,
0.661538461538461,0.676923076923076,0.692307692307692,0.707692307692307,
0.723076923076922,0.738461538461538,0.753846153846153,0.769230769230768,
0.784615384615384,0.799999999999999,0.815384615384614,0.83076923076923,
0.846153846153845,0.86153846153846,0.876923076923076,0.892307692307691,
0.907692307692306,0.923076923076922,0.938461538461537,0.953846153846152,
0.969230769230768,0.984615384615383,1.),.UNSPECIFIED.)
CURVE()
GEOMETRIC_REPRESENTATION_ITEM()
RATIONAL_B_SPLINE_CURVE((1.,1.,1.,1.,1.,1.,1.,1.,1.,1.,1.,1.,1.,1.,1.,1.,
1.,1.,1.,1.,1.,1.,1.,1.,1.,1.,1.,1.,1.,1.,1.,1.,1.,1.,1.,1.,1.,1.,1.,1.,
1.,1.,1.,1.,1.,1.,1.,1.,1.,1.,1.,1.,1.,1.,1.,1.,1.,1.,1.,1.,1.,1.,1.,1.,
1.,1.,1.,1.,1.,1.))
REPRESENTATION_ITEM('')
);
#166=(
BOUNDED_CURVE()
B_SPLINE_CURVE(5,(#24805,#24806,#24807,#24808,#24809,#24810,#24811,#24812,
#24813,#24814,#24815,#24816,#24817,#24818,#24819,#24820,#24821,#24822,#24823,
#24824,#24825,#24826,#24827,#24828,#24829,#24830,#24831,#24832,#24833,#24834,
#24835,#24836,#24837,#24838,#24839,#24840,#24841,#24842,#24843,#24844,#24845,
#24846,#24847,#24848,#24849,#24850,#24851,#24852,#24853,#24854,#24855,#24856,
#24857,#24858,#24859,#24860,#24861,#24862,#24863,#24864,#24865,#24866,#24867,
#24868,#24869,#24870,#24871,#24872,#24873,#24874),.UNSPECIFIED.,.F.,.F.)
B_SPLINE_CURVE_WITH_KNOTS((6,1,1,1,1,1,1,1,1,1,1,1,1,1,1,1,1,1,1,1,1,1,
1,1,1,1,1,1,1,1,1,1,1,1,1,1,1,1,1,1,1,1,1,1,1,1,1,1,1,1,1,1,1,1,1,1,1,1,
1,1,1,1,1,1,1,6),(0.,0.0153846153846154,0.0307692307692308,0.0461538461538462,
0.0615384615384615,0.0769230769230769,0.0923076923076923,0.107692307692308,
0.123076923076923,0.138461538461538,0.153846153846154,0.169230769230769,
0.184615384615385,0.2,0.215384615384615,0.230769230769231,0.246153846153846,
0.261538461538462,0.276923076923077,0.292307692307692,0.307692307692308,
0.323076923076923,0.338461538461538,0.353846153846154,0.369230769230769,
0.384615384615385,0.4,0.415384615384615,0.430769230769231,0.446153846153846,
0.461538461538462,0.476923076923077,0.492307692307692,0.507692307692308,
0.523076923076923,0.538461538461538,0.553846153846154,0.569230769230769,
0.584615384615384,0.6,0.615384615384615,0.63076923076923,0.646153846153846,
0.661538461538461,0.676923076923076,0.692307692307692,0.707692307692307,
0.723076923076922,0.738461538461538,0.753846153846153,0.769230769230768,
0.784615384615384,0.799999999999999,0.815384615384614,0.83076923076923,
0.846153846153845,0.86153846153846,0.876923076923076,0.892307692307691,
0.907692307692306,0.923076923076922,0.938461538461537,0.953846153846152,
0.969230769230768,0.984615384615383,1.),.UNSPECIFIED.)
CURVE()
GEOMETRIC_REPRESENTATION_ITEM()
RATIONAL_B_SPLINE_CURVE((1.,1.,1.,1.,1.,1.,1.,1.,1.,1.,1.,1.,1.,1.,1.,1.,
1.,1.,1.,1.,1.,1.,1.,1.,1.,1.,1.,1.,1.,1.,1.,1.,1.,1.,1.,1.,1.,1.,1.,1.,
1.,1.,1.,1.,1.,1.,1.,1.,1.,1.,1.,1.,1.,1.,1.,1.,1.,1.,1.,1.,1.,1.,1.,1.,
1.,1.,1.,1.,1.,1.))
REPRESENTATION_ITEM('')
);
#167=(
BOUNDED_CURVE()
B_SPLINE_CURVE(5,(#24878,#24879,#24880,#24881,#24882,#24883,#24884,#24885,
#24886,#24887,#24888,#24889,#24890,#24891,#24892,#24893,#24894,#24895,#24896,
#24897,#24898,#24899,#24900,#24901,#24902,#24903,#24904,#24905,#24906,#24907,
#24908,#24909,#24910,#24911,#24912,#24913,#24914,#24915,#24916,#24917,#24918,
#24919,#24920,#24921,#24922,#24923,#24924,#24925,#24926,#24927,#24928,#24929,
#24930,#24931,#24932,#24933,#24934,#24935,#24936,#24937,#24938,#24939,#24940,
#24941,#24942,#24943,#24944,#24945,#24946,#24947),.UNSPECIFIED.,.F.,.F.)
B_SPLINE_CURVE_WITH_KNOTS((6,1,1,1,1,1,1,1,1,1,1,1,1,1,1,1,1,1,1,1,1,1,
1,1,1,1,1,1,1,1,1,1,1,1,1,1,1,1,1,1,1,1,1,1,1,1,1,1,1,1,1,1,1,1,1,1,1,1,
1,1,1,1,1,1,1,6),(0.,0.0153846153846154,0.0307692307692308,0.0461538461538462,
0.0615384615384615,0.0769230769230769,0.0923076923076923,0.107692307692308,
0.123076923076923,0.138461538461538,0.153846153846154,0.169230769230769,
0.184615384615385,0.2,0.215384615384615,0.230769230769231,0.246153846153846,
0.261538461538462,0.276923076923077,0.292307692307692,0.307692307692308,
0.323076923076923,0.338461538461538,0.353846153846154,0.369230769230769,
0.384615384615385,0.4,0.415384615384615,0.430769230769231,0.446153846153846,
0.461538461538462,0.476923076923077,0.492307692307692,0.507692307692308,
0.523076923076923,0.538461538461538,0.553846153846154,0.569230769230769,
0.584615384615384,0.6,0.615384615384615,0.63076923076923,0.646153846153846,
0.661538461538461,0.676923076923076,0.692307692307692,0.707692307692307,
0.723076923076922,0.738461538461538,0.753846153846153,0.769230769230768,
0.784615384615384,0.799999999999999,0.815384615384614,0.83076923076923,
0.846153846153845,0.86153846153846,0.876923076923076,0.892307692307691,
0.907692307692306,0.923076923076922,0.938461538461537,0.953846153846152,
0.969230769230768,0.984615384615383,1.),.UNSPECIFIED.)
CURVE()
GEOMETRIC_REPRESENTATION_ITEM()
RATIONAL_B_SPLINE_CURVE((1.,1.,1.,1.,1.,1.,1.,1.,1.,1.,1.,1.,1.,1.,1.,1.,
1.,1.,1.,1.,1.,1.,1.,1.,1.,1.,1.,1.,1.,1.,1.,1.,1.,1.,1.,1.,1.,1.,1.,1.,
1.,1.,1.,1.,1.,1.,1.,1.,1.,1.,1.,1.,1.,1.,1.,1.,1.,1.,1.,1.,1.,1.,1.,1.,
1.,1.,1.,1.,1.,1.))
REPRESENTATION_ITEM('')
);
#168=(
BOUNDED_CURVE()
B_SPLINE_CURVE(5,(#24951,#24952,#24953,#24954,#24955,#24956,#24957,#24958,
#24959,#24960,#24961,#24962,#24963,#24964,#24965,#24966,#24967,#24968,#24969,
#24970,#24971,#24972,#24973,#24974,#24975,#24976,#24977,#24978,#24979,#24980,
#24981,#24982,#24983,#24984,#24985,#24986,#24987,#24988,#24989,#24990,#24991,
#24992,#24993,#24994,#24995,#24996,#24997,#24998,#24999,#25000,#25001,#25002,
#25003,#25004,#25005,#25006,#25007,#25008,#25009,#25010,#25011,#25012,#25013,
#25014,#25015,#25016,#25017,#25018,#25019,#25020),.UNSPECIFIED.,.F.,.F.)
B_SPLINE_CURVE_WITH_KNOTS((6,1,1,1,1,1,1,1,1,1,1,1,1,1,1,1,1,1,1,1,1,1,
1,1,1,1,1,1,1,1,1,1,1,1,1,1,1,1,1,1,1,1,1,1,1,1,1,1,1,1,1,1,1,1,1,1,1,1,
1,1,1,1,1,1,1,6),(0.,0.0153846153846154,0.0307692307692308,0.0461538461538462,
0.0615384615384615,0.0769230769230769,0.0923076923076923,0.107692307692308,
0.123076923076923,0.138461538461538,0.153846153846154,0.169230769230769,
0.184615384615385,0.2,0.215384615384615,0.230769230769231,0.246153846153846,
0.261538461538462,0.276923076923077,0.292307692307692,0.307692307692308,
0.323076923076923,0.338461538461538,0.353846153846154,0.369230769230769,
0.384615384615385,0.4,0.415384615384615,0.430769230769231,0.446153846153846,
0.461538461538462,0.476923076923077,0.492307692307692,0.507692307692308,
0.523076923076923,0.538461538461538,0.553846153846154,0.569230769230769,
0.584615384615384,0.6,0.615384615384615,0.63076923076923,0.646153846153846,
0.661538461538461,0.676923076923076,0.692307692307692,0.707692307692307,
0.723076923076922,0.738461538461538,0.753846153846153,0.769230769230768,
0.784615384615384,0.799999999999999,0.815384615384614,0.83076923076923,
0.846153846153845,0.86153846153846,0.876923076923076,0.892307692307691,
0.907692307692306,0.923076923076922,0.938461538461537,0.953846153846152,
0.969230769230768,0.984615384615383,1.),.UNSPECIFIED.)
CURVE()
GEOMETRIC_REPRESENTATION_ITEM()
RATIONAL_B_SPLINE_CURVE((1.,1.,1.,1.,1.,1.,1.,1.,1.,1.,1.,1.,1.,1.,1.,1.,
1.,1.,1.,1.,1.,1.,1.,1.,1.,1.,1.,1.,1.,1.,1.,1.,1.,1.,1.,1.,1.,1.,1.,1.,
1.,1.,1.,1.,1.,1.,1.,1.,1.,1.,1.,1.,1.,1.,1.,1.,1.,1.,1.,1.,1.,1.,1.,1.,
1.,1.,1.,1.,1.,1.))
REPRESENTATION_ITEM('')
);
#169=(
BOUNDED_CURVE()
B_SPLINE_CURVE(5,(#25024,#25025,#25026,#25027,#25028,#25029,#25030,#25031,
#25032,#25033,#25034,#25035,#25036,#25037,#25038,#25039,#25040,#25041,#25042,
#25043,#25044,#25045,#25046,#25047,#25048,#25049,#25050,#25051,#25052,#25053,
#25054,#25055,#25056,#25057,#25058,#25059,#25060,#25061,#25062,#25063,#25064,
#25065,#25066,#25067,#25068,#25069,#25070,#25071,#25072,#25073,#25074,#25075,
#25076,#25077,#25078,#25079,#25080,#25081,#25082,#25083,#25084,#25085,#25086,
#25087,#25088,#25089,#25090,#25091,#25092,#25093),.UNSPECIFIED.,.F.,.F.)
B_SPLINE_CURVE_WITH_KNOTS((6,1,1,1,1,1,1,1,1,1,1,1,1,1,1,1,1,1,1,1,1,1,
1,1,1,1,1,1,1,1,1,1,1,1,1,1,1,1,1,1,1,1,1,1,1,1,1,1,1,1,1,1,1,1,1,1,1,1,
1,1,1,1,1,1,1,6),(0.,0.0153846153846154,0.0307692307692308,0.0461538461538462,
0.0615384615384615,0.0769230769230769,0.0923076923076923,0.107692307692308,
0.123076923076923,0.138461538461538,0.153846153846154,0.169230769230769,
0.184615384615385,0.2,0.215384615384615,0.230769230769231,0.246153846153846,
0.261538461538462,0.276923076923077,0.292307692307692,0.307692307692308,
0.323076923076923,0.338461538461538,0.353846153846154,0.369230769230769,
0.384615384615385,0.4,0.415384615384615,0.430769230769231,0.446153846153846,
0.461538461538462,0.476923076923077,0.492307692307692,0.507692307692308,
0.523076923076923,0.538461538461538,0.553846153846154,0.569230769230769,
0.584615384615384,0.6,0.615384615384615,0.63076923076923,0.646153846153846,
0.661538461538461,0.676923076923076,0.692307692307692,0.707692307692307,
0.723076923076922,0.738461538461538,0.753846153846153,0.769230769230768,
0.784615384615384,0.799999999999999,0.815384615384614,0.83076923076923,
0.846153846153845,0.86153846153846,0.876923076923076,0.892307692307691,
0.907692307692306,0.923076923076922,0.938461538461537,0.953846153846152,
0.969230769230768,0.984615384615383,1.),.UNSPECIFIED.)
CURVE()
GEOMETRIC_REPRESENTATION_ITEM()
RATIONAL_B_SPLINE_CURVE((1.,1.,1.,1.,1.,1.,1.,1.,1.,1.,1.,1.,1.,1.,1.,1.,
1.,1.,1.,1.,1.,1.,1.,1.,1.,1.,1.,1.,1.,1.,1.,1.,1.,1.,1.,1.,1.,1.,1.,1.,
1.,1.,1.,1.,1.,1.,1.,1.,1.,1.,1.,1.,1.,1.,1.,1.,1.,1.,1.,1.,1.,1.,1.,1.,
1.,1.,1.,1.,1.,1.))
REPRESENTATION_ITEM('')
);
#170=(
BOUNDED_CURVE()
B_SPLINE_CURVE(5,(#25096,#25097,#25098,#25099,#25100,#25101,#25102,#25103,
#25104,#25105,#25106,#25107,#25108,#25109,#25110,#25111,#25112,#25113,#25114,
#25115,#25116,#25117,#25118,#25119,#25120,#25121,#25122,#25123,#25124,#25125,
#25126,#25127,#25128,#25129,#25130,#25131,#25132,#25133,#25134,#25135,#25136,
#25137,#25138,#25139,#25140,#25141,#25142,#25143,#25144,#25145,#25146,#25147,
#25148,#25149,#25150,#25151,#25152,#25153,#25154,#25155,#25156,#25157,#25158,
#25159,#25160,#25161,#25162,#25163,#25164,#25165),.UNSPECIFIED.,.F.,.F.)
B_SPLINE_CURVE_WITH_KNOTS((6,1,1,1,1,1,1,1,1,1,1,1,1,1,1,1,1,1,1,1,1,1,
1,1,1,1,1,1,1,1,1,1,1,1,1,1,1,1,1,1,1,1,1,1,1,1,1,1,1,1,1,1,1,1,1,1,1,1,
1,1,1,1,1,1,1,6),(0.,0.0153846153846154,0.0307692307692308,0.0461538461538462,
0.0615384615384615,0.0769230769230769,0.0923076923076923,0.107692307692308,
0.123076923076923,0.138461538461538,0.153846153846154,0.169230769230769,
0.184615384615385,0.2,0.215384615384615,0.230769230769231,0.246153846153846,
0.261538461538462,0.276923076923077,0.292307692307692,0.307692307692308,
0.323076923076923,0.338461538461538,0.353846153846154,0.369230769230769,
0.384615384615385,0.4,0.415384615384615,0.430769230769231,0.446153846153846,
0.461538461538462,0.476923076923077,0.492307692307692,0.507692307692308,
0.523076923076923,0.538461538461538,0.553846153846154,0.569230769230769,
0.584615384615384,0.6,0.615384615384615,0.63076923076923,0.646153846153846,
0.661538461538461,0.676923076923076,0.692307692307692,0.707692307692307,
0.723076923076922,0.738461538461538,0.753846153846153,0.769230769230768,
0.784615384615384,0.799999999999999,0.815384615384614,0.83076923076923,
0.846153846153845,0.86153846153846,0.876923076923076,0.892307692307691,
0.907692307692306,0.923076923076922,0.938461538461537,0.953846153846152,
0.969230769230768,0.984615384615383,1.),.UNSPECIFIED.)
CURVE()
GEOMETRIC_REPRESENTATION_ITEM()
RATIONAL_B_SPLINE_CURVE((1.,1.,1.,1.,1.,1.,1.,1.,1.,1.,1.,1.,1.,1.,1.,1.,
1.,1.,1.,1.,1.,1.,1.,1.,1.,1.,1.,1.,1.,1.,1.,1.,1.,1.,1.,1.,1.,1.,1.,1.,
1.,1.,1.,1.,1.,1.,1.,1.,1.,1.,1.,1.,1.,1.,1.,1.,1.,1.,1.,1.,1.,1.,1.,1.,
1.,1.,1.,1.,1.,1.))
REPRESENTATION_ITEM('')
);
#171=(
BOUNDED_CURVE()
B_SPLINE_CURVE(5,(#25319,#25320,#25321,#25322,#25323,#25324,#25325,#25326,
#25327,#25328,#25329,#25330,#25331,#25332,#25333,#25334,#25335,#25336,#25337,
#25338,#25339,#25340,#25341,#25342,#25343,#25344,#25345,#25346,#25347,#25348,
#25349,#25350,#25351,#25352,#25353,#25354,#25355,#25356,#25357,#25358,#25359,
#25360,#25361,#25362,#25363,#25364,#25365,#25366,#25367,#25368,#25369,#25370,
#25371,#25372,#25373,#25374,#25375,#25376,#25377,#25378,#25379,#25380,#25381,
#25382,#25383,#25384,#25385,#25386,#25387,#25388),.UNSPECIFIED.,.F.,.F.)
B_SPLINE_CURVE_WITH_KNOTS((6,1,1,1,1,1,1,1,1,1,1,1,1,1,1,1,1,1,1,1,1,1,
1,1,1,1,1,1,1,1,1,1,1,1,1,1,1,1,1,1,1,1,1,1,1,1,1,1,1,1,1,1,1,1,1,1,1,1,
1,1,1,1,1,1,1,6),(-1.,-0.984615384615383,-0.969230769230768,-0.953846153846152,
-0.938461538461537,-0.923076923076922,-0.907692307692306,-0.892307692307691,
-0.876923076923076,-0.86153846153846,-0.846153846153845,-0.83076923076923,
-0.815384615384614,-0.799999999999999,-0.784615384615384,-0.769230769230768,
-0.753846153846153,-0.738461538461538,-0.723076923076922,-0.707692307692307,
-0.692307692307692,-0.676923076923076,-0.661538461538461,-0.646153846153846,
-0.63076923076923,-0.615384615384615,-0.6,-0.584615384615384,-0.569230769230769,
-0.553846153846154,-0.538461538461538,-0.523076923076923,-0.507692307692308,
-0.492307692307692,-0.476923076923077,-0.461538461538462,-0.446153846153846,
-0.430769230769231,-0.415384615384615,-0.4,-0.384615384615385,-0.369230769230769,
-0.353846153846154,-0.338461538461538,-0.323076923076923,-0.307692307692308,
-0.292307692307692,-0.276923076923077,-0.261538461538462,-0.246153846153846,
-0.230769230769231,-0.215384615384615,-0.2,-0.184615384615385,-0.169230769230769,
-0.153846153846154,-0.138461538461538,-0.123076923076923,-0.107692307692308,
-0.0923076923076923,-0.0769230769230769,-0.0615384615384615,-0.0461538461538462,
-0.0307692307692308,-0.0153846153846154,0.),.UNSPECIFIED.)
CURVE()
GEOMETRIC_REPRESENTATION_ITEM()
RATIONAL_B_SPLINE_CURVE((1.,1.,1.,1.,1.,1.,1.,1.,1.,1.,1.,1.,1.,1.,1.,1.,
1.,1.,1.,1.,1.,1.,1.,1.,1.,1.,1.,1.,1.,1.,1.,1.,1.,1.,1.,1.,1.,1.,1.,1.,
1.,1.,1.,1.,1.,1.,1.,1.,1.,1.,1.,1.,1.,1.,1.,1.,1.,1.,1.,1.,1.,1.,1.,1.,
1.,1.,1.,1.,1.,1.))
REPRESENTATION_ITEM('')
);
#172=(
BOUNDED_CURVE()
B_SPLINE_CURVE(5,(#25535,#25536,#25537,#25538,#25539,#25540,#25541,#25542,
#25543,#25544,#25545,#25546,#25547,#25548,#25549,#25550,#25551,#25552,#25553,
#25554,#25555,#25556,#25557,#25558,#25559,#25560,#25561,#25562,#25563,#25564,
#25565,#25566,#25567,#25568,#25569,#25570,#25571,#25572,#25573,#25574,#25575,
#25576,#25577,#25578,#25579,#25580,#25581,#25582,#25583,#25584,#25585,#25586,
#25587,#25588,#25589,#25590,#25591,#25592,#25593,#25594,#25595,#25596,#25597,
#25598,#25599,#25600,#25601,#25602,#25603,#25604),.UNSPECIFIED.,.F.,.F.)
B_SPLINE_CURVE_WITH_KNOTS((6,1,1,1,1,1,1,1,1,1,1,1,1,1,1,1,1,1,1,1,1,1,
1,1,1,1,1,1,1,1,1,1,1,1,1,1,1,1,1,1,1,1,1,1,1,1,1,1,1,1,1,1,1,1,1,1,1,1,
1,1,1,1,1,1,1,6),(-1.,-0.984615384615383,-0.969230769230768,-0.953846153846152,
-0.938461538461537,-0.923076923076922,-0.907692307692306,-0.892307692307691,
-0.876923076923076,-0.86153846153846,-0.846153846153845,-0.83076923076923,
-0.815384615384614,-0.799999999999999,-0.784615384615384,-0.769230769230768,
-0.753846153846153,-0.738461538461538,-0.723076923076922,-0.707692307692307,
-0.692307692307692,-0.676923076923076,-0.661538461538461,-0.646153846153846,
-0.63076923076923,-0.615384615384615,-0.6,-0.584615384615384,-0.569230769230769,
-0.553846153846154,-0.538461538461538,-0.523076923076923,-0.507692307692308,
-0.492307692307692,-0.476923076923077,-0.461538461538462,-0.446153846153846,
-0.430769230769231,-0.415384615384615,-0.4,-0.384615384615385,-0.369230769230769,
-0.353846153846154,-0.338461538461538,-0.323076923076923,-0.307692307692308,
-0.292307692307692,-0.276923076923077,-0.261538461538462,-0.246153846153846,
-0.230769230769231,-0.215384615384615,-0.2,-0.184615384615385,-0.169230769230769,
-0.153846153846154,-0.138461538461538,-0.123076923076923,-0.107692307692308,
-0.0923076923076923,-0.0769230769230769,-0.0615384615384615,-0.0461538461538462,
-0.0307692307692308,-0.0153846153846154,0.),.UNSPECIFIED.)
CURVE()
GEOMETRIC_REPRESENTATION_ITEM()
RATIONAL_B_SPLINE_CURVE((1.,1.,1.,1.,1.,1.,1.,1.,1.,1.,1.,1.,1.,1.,1.,1.,
1.,1.,1.,1.,1.,1.,1.,1.,1.,1.,1.,1.,1.,1.,1.,1.,1.,1.,1.,1.,1.,1.,1.,1.,
1.,1.,1.,1.,1.,1.,1.,1.,1.,1.,1.,1.,1.,1.,1.,1.,1.,1.,1.,1.,1.,1.,1.,1.,
1.,1.,1.,1.,1.,1.))
REPRESENTATION_ITEM('')
);
#173=(
BOUNDED_CURVE()
B_SPLINE_CURVE(5,(#25751,#25752,#25753,#25754,#25755,#25756,#25757,#25758,
#25759,#25760,#25761,#25762,#25763,#25764,#25765,#25766,#25767,#25768,#25769,
#25770,#25771,#25772,#25773,#25774,#25775,#25776,#25777,#25778,#25779,#25780,
#25781,#25782,#25783,#25784,#25785,#25786,#25787,#25788,#25789,#25790,#25791,
#25792,#25793,#25794,#25795,#25796,#25797,#25798,#25799,#25800,#25801,#25802,
#25803,#25804,#25805,#25806,#25807,#25808,#25809,#25810,#25811,#25812,#25813,
#25814,#25815,#25816,#25817,#25818,#25819,#25820),.UNSPECIFIED.,.F.,.F.)
B_SPLINE_CURVE_WITH_KNOTS((6,1,1,1,1,1,1,1,1,1,1,1,1,1,1,1,1,1,1,1,1,1,
1,1,1,1,1,1,1,1,1,1,1,1,1,1,1,1,1,1,1,1,1,1,1,1,1,1,1,1,1,1,1,1,1,1,1,1,
1,1,1,1,1,1,1,6),(-1.,-0.984615384615383,-0.969230769230768,-0.953846153846152,
-0.938461538461537,-0.923076923076922,-0.907692307692306,-0.892307692307691,
-0.876923076923076,-0.86153846153846,-0.846153846153845,-0.83076923076923,
-0.815384615384614,-0.799999999999999,-0.784615384615384,-0.769230769230768,
-0.753846153846153,-0.738461538461538,-0.723076923076922,-0.707692307692307,
-0.692307692307692,-0.676923076923076,-0.661538461538461,-0.646153846153846,
-0.63076923076923,-0.615384615384615,-0.6,-0.584615384615384,-0.569230769230769,
-0.553846153846154,-0.538461538461538,-0.523076923076923,-0.507692307692308,
-0.492307692307692,-0.476923076923077,-0.461538461538462,-0.446153846153846,
-0.430769230769231,-0.415384615384615,-0.4,-0.384615384615385,-0.369230769230769,
-0.353846153846154,-0.338461538461538,-0.323076923076923,-0.307692307692308,
-0.292307692307692,-0.276923076923077,-0.261538461538462,-0.246153846153846,
-0.230769230769231,-0.215384615384615,-0.2,-0.184615384615385,-0.169230769230769,
-0.153846153846154,-0.138461538461538,-0.123076923076923,-0.107692307692308,
-0.0923076923076923,-0.0769230769230769,-0.0615384615384615,-0.0461538461538462,
-0.0307692307692308,-0.0153846153846154,0.),.UNSPECIFIED.)
CURVE()
GEOMETRIC_REPRESENTATION_ITEM()
RATIONAL_B_SPLINE_CURVE((1.,1.,1.,1.,1.,1.,1.,1.,1.,1.,1.,1.,1.,1.,1.,1.,
1.,1.,1.,1.,1.,1.,1.,1.,1.,1.,1.,1.,1.,1.,1.,1.,1.,1.,1.,1.,1.,1.,1.,1.,
1.,1.,1.,1.,1.,1.,1.,1.,1.,1.,1.,1.,1.,1.,1.,1.,1.,1.,1.,1.,1.,1.,1.,1.,
1.,1.,1.,1.,1.,1.))
REPRESENTATION_ITEM('')
);
#174=(
BOUNDED_CURVE()
B_SPLINE_CURVE(5,(#25967,#25968,#25969,#25970,#25971,#25972,#25973,#25974,
#25975,#25976,#25977,#25978,#25979,#25980,#25981,#25982,#25983,#25984,#25985,
#25986,#25987,#25988,#25989,#25990,#25991,#25992,#25993,#25994,#25995,#25996,
#25997,#25998,#25999,#26000,#26001,#26002,#26003,#26004,#26005,#26006,#26007,
#26008,#26009,#26010,#26011,#26012,#26013,#26014,#26015,#26016,#26017,#26018,
#26019,#26020,#26021,#26022,#26023,#26024,#26025,#26026,#26027,#26028,#26029,
#26030,#26031,#26032,#26033,#26034,#26035,#26036),.UNSPECIFIED.,.F.,.F.)
B_SPLINE_CURVE_WITH_KNOTS((6,1,1,1,1,1,1,1,1,1,1,1,1,1,1,1,1,1,1,1,1,1,
1,1,1,1,1,1,1,1,1,1,1,1,1,1,1,1,1,1,1,1,1,1,1,1,1,1,1,1,1,1,1,1,1,1,1,1,
1,1,1,1,1,1,1,6),(-1.,-0.984615384615383,-0.969230769230768,-0.953846153846152,
-0.938461538461537,-0.923076923076922,-0.907692307692306,-0.892307692307691,
-0.876923076923076,-0.86153846153846,-0.846153846153845,-0.83076923076923,
-0.815384615384614,-0.799999999999999,-0.784615384615384,-0.769230769230768,
-0.753846153846153,-0.738461538461538,-0.723076923076922,-0.707692307692307,
-0.692307692307692,-0.676923076923076,-0.661538461538461,-0.646153846153846,
-0.63076923076923,-0.615384615384615,-0.6,-0.584615384615384,-0.569230769230769,
-0.553846153846154,-0.538461538461538,-0.523076923076923,-0.507692307692308,
-0.492307692307692,-0.476923076923077,-0.461538461538462,-0.446153846153846,
-0.430769230769231,-0.415384615384615,-0.4,-0.384615384615385,-0.369230769230769,
-0.353846153846154,-0.338461538461538,-0.323076923076923,-0.307692307692308,
-0.292307692307692,-0.276923076923077,-0.261538461538462,-0.246153846153846,
-0.230769230769231,-0.215384615384615,-0.2,-0.184615384615385,-0.169230769230769,
-0.153846153846154,-0.138461538461538,-0.123076923076923,-0.107692307692308,
-0.0923076923076923,-0.0769230769230769,-0.0615384615384615,-0.0461538461538462,
-0.0307692307692308,-0.0153846153846154,0.),.UNSPECIFIED.)
CURVE()
GEOMETRIC_REPRESENTATION_ITEM()
RATIONAL_B_SPLINE_CURVE((1.,1.,1.,1.,1.,1.,1.,1.,1.,1.,1.,1.,1.,1.,1.,1.,
1.,1.,1.,1.,1.,1.,1.,1.,1.,1.,1.,1.,1.,1.,1.,1.,1.,1.,1.,1.,1.,1.,1.,1.,
1.,1.,1.,1.,1.,1.,1.,1.,1.,1.,1.,1.,1.,1.,1.,1.,1.,1.,1.,1.,1.,1.,1.,1.,
1.,1.,1.,1.,1.,1.))
REPRESENTATION_ITEM('')
);
#175=(
BOUNDED_CURVE()
B_SPLINE_CURVE(5,(#26183,#26184,#26185,#26186,#26187,#26188,#26189,#26190,
#26191,#26192,#26193,#26194,#26195,#26196,#26197,#26198,#26199,#26200,#26201,
#26202,#26203,#26204,#26205,#26206,#26207,#26208,#26209,#26210,#26211,#26212,
#26213,#26214,#26215,#26216,#26217,#26218,#26219,#26220,#26221,#26222,#26223,
#26224,#26225,#26226,#26227,#26228,#26229,#26230,#26231,#26232,#26233,#26234,
#26235,#26236,#26237,#26238,#26239,#26240,#26241,#26242,#26243,#26244,#26245,
#26246,#26247,#26248,#26249,#26250,#26251,#26252),.UNSPECIFIED.,.F.,.F.)
B_SPLINE_CURVE_WITH_KNOTS((6,1,1,1,1,1,1,1,1,1,1,1,1,1,1,1,1,1,1,1,1,1,
1,1,1,1,1,1,1,1,1,1,1,1,1,1,1,1,1,1,1,1,1,1,1,1,1,1,1,1,1,1,1,1,1,1,1,1,
1,1,1,1,1,1,1,6),(-1.,-0.984615384615383,-0.969230769230768,-0.953846153846152,
-0.938461538461537,-0.923076923076922,-0.907692307692306,-0.892307692307691,
-0.876923076923076,-0.86153846153846,-0.846153846153845,-0.83076923076923,
-0.815384615384614,-0.799999999999999,-0.784615384615384,-0.769230769230768,
-0.753846153846153,-0.738461538461538,-0.723076923076922,-0.707692307692307,
-0.692307692307692,-0.676923076923076,-0.661538461538461,-0.646153846153846,
-0.63076923076923,-0.615384615384615,-0.6,-0.584615384615384,-0.569230769230769,
-0.553846153846154,-0.538461538461538,-0.523076923076923,-0.507692307692308,
-0.492307692307692,-0.476923076923077,-0.461538461538462,-0.446153846153846,
-0.430769230769231,-0.415384615384615,-0.4,-0.384615384615385,-0.369230769230769,
-0.353846153846154,-0.338461538461538,-0.323076923076923,-0.307692307692308,
-0.292307692307692,-0.276923076923077,-0.261538461538462,-0.246153846153846,
-0.230769230769231,-0.215384615384615,-0.2,-0.184615384615385,-0.169230769230769,
-0.153846153846154,-0.138461538461538,-0.123076923076923,-0.107692307692308,
-0.0923076923076923,-0.0769230769230769,-0.0615384615384615,-0.0461538461538462,
-0.0307692307692308,-0.0153846153846154,0.),.UNSPECIFIED.)
CURVE()
GEOMETRIC_REPRESENTATION_ITEM()
RATIONAL_B_SPLINE_CURVE((1.,1.,1.,1.,1.,1.,1.,1.,1.,1.,1.,1.,1.,1.,1.,1.,
1.,1.,1.,1.,1.,1.,1.,1.,1.,1.,1.,1.,1.,1.,1.,1.,1.,1.,1.,1.,1.,1.,1.,1.,
1.,1.,1.,1.,1.,1.,1.,1.,1.,1.,1.,1.,1.,1.,1.,1.,1.,1.,1.,1.,1.,1.,1.,1.,
1.,1.,1.,1.,1.,1.))
REPRESENTATION_ITEM('')
);
#176=(
BOUNDED_CURVE()
B_SPLINE_CURVE(5,(#26399,#26400,#26401,#26402,#26403,#26404,#26405,#26406,
#26407,#26408,#26409,#26410,#26411,#26412,#26413,#26414,#26415,#26416,#26417,
#26418,#26419,#26420,#26421,#26422,#26423,#26424,#26425,#26426,#26427,#26428,
#26429,#26430,#26431,#26432,#26433,#26434,#26435,#26436,#26437,#26438,#26439,
#26440,#26441,#26442,#26443,#26444,#26445,#26446,#26447,#26448,#26449,#26450,
#26451,#26452,#26453,#26454,#26455,#26456,#26457,#26458,#26459,#26460,#26461,
#26462,#26463,#26464,#26465,#26466,#26467,#26468),.UNSPECIFIED.,.F.,.F.)
B_SPLINE_CURVE_WITH_KNOTS((6,1,1,1,1,1,1,1,1,1,1,1,1,1,1,1,1,1,1,1,1,1,
1,1,1,1,1,1,1,1,1,1,1,1,1,1,1,1,1,1,1,1,1,1,1,1,1,1,1,1,1,1,1,1,1,1,1,1,
1,1,1,1,1,1,1,6),(-1.,-0.984615384615383,-0.969230769230768,-0.953846153846152,
-0.938461538461537,-0.923076923076922,-0.907692307692306,-0.892307692307691,
-0.876923076923076,-0.86153846153846,-0.846153846153845,-0.83076923076923,
-0.815384615384614,-0.799999999999999,-0.784615384615384,-0.769230769230768,
-0.753846153846153,-0.738461538461538,-0.723076923076922,-0.707692307692307,
-0.692307692307692,-0.676923076923076,-0.661538461538461,-0.646153846153846,
-0.63076923076923,-0.615384615384615,-0.6,-0.584615384615384,-0.569230769230769,
-0.553846153846154,-0.538461538461538,-0.523076923076923,-0.507692307692308,
-0.492307692307692,-0.476923076923077,-0.461538461538462,-0.446153846153846,
-0.430769230769231,-0.415384615384615,-0.4,-0.384615384615385,-0.369230769230769,
-0.353846153846154,-0.338461538461538,-0.323076923076923,-0.307692307692308,
-0.292307692307692,-0.276923076923077,-0.261538461538462,-0.246153846153846,
-0.230769230769231,-0.215384615384615,-0.2,-0.184615384615385,-0.169230769230769,
-0.153846153846154,-0.138461538461538,-0.123076923076923,-0.107692307692308,
-0.0923076923076923,-0.0769230769230769,-0.0615384615384615,-0.0461538461538462,
-0.0307692307692308,-0.0153846153846154,0.),.UNSPECIFIED.)
CURVE()
GEOMETRIC_REPRESENTATION_ITEM()
RATIONAL_B_SPLINE_CURVE((1.,1.,1.,1.,1.,1.,1.,1.,1.,1.,1.,1.,1.,1.,1.,1.,
1.,1.,1.,1.,1.,1.,1.,1.,1.,1.,1.,1.,1.,1.,1.,1.,1.,1.,1.,1.,1.,1.,1.,1.,
1.,1.,1.,1.,1.,1.,1.,1.,1.,1.,1.,1.,1.,1.,1.,1.,1.,1.,1.,1.,1.,1.,1.,1.,
1.,1.,1.,1.,1.,1.))
REPRESENTATION_ITEM('')
);
#177=(
BOUNDED_CURVE()
B_SPLINE_CURVE(5,(#26615,#26616,#26617,#26618,#26619,#26620,#26621,#26622,
#26623,#26624,#26625,#26626,#26627,#26628,#26629,#26630,#26631,#26632,#26633,
#26634,#26635,#26636,#26637,#26638,#26639,#26640,#26641,#26642,#26643,#26644,
#26645,#26646,#26647,#26648,#26649,#26650,#26651,#26652,#26653,#26654,#26655,
#26656,#26657,#26658,#26659,#26660,#26661,#26662,#26663,#26664,#26665,#26666,
#26667,#26668,#26669,#26670,#26671,#26672,#26673,#26674,#26675,#26676,#26677,
#26678,#26679,#26680,#26681,#26682,#26683,#26684),.UNSPECIFIED.,.F.,.F.)
B_SPLINE_CURVE_WITH_KNOTS((6,1,1,1,1,1,1,1,1,1,1,1,1,1,1,1,1,1,1,1,1,1,
1,1,1,1,1,1,1,1,1,1,1,1,1,1,1,1,1,1,1,1,1,1,1,1,1,1,1,1,1,1,1,1,1,1,1,1,
1,1,1,1,1,1,1,6),(-1.,-0.984615384615383,-0.969230769230768,-0.953846153846152,
-0.938461538461537,-0.923076923076922,-0.907692307692306,-0.892307692307691,
-0.876923076923076,-0.86153846153846,-0.846153846153845,-0.83076923076923,
-0.815384615384614,-0.799999999999999,-0.784615384615384,-0.769230769230768,
-0.753846153846153,-0.738461538461538,-0.723076923076922,-0.707692307692307,
-0.692307692307692,-0.676923076923076,-0.661538461538461,-0.646153846153846,
-0.63076923076923,-0.615384615384615,-0.6,-0.584615384615384,-0.569230769230769,
-0.553846153846154,-0.538461538461538,-0.523076923076923,-0.507692307692308,
-0.492307692307692,-0.476923076923077,-0.461538461538462,-0.446153846153846,
-0.430769230769231,-0.415384615384615,-0.4,-0.384615384615385,-0.369230769230769,
-0.353846153846154,-0.338461538461538,-0.323076923076923,-0.307692307692308,
-0.292307692307692,-0.276923076923077,-0.261538461538462,-0.246153846153846,
-0.230769230769231,-0.215384615384615,-0.2,-0.184615384615385,-0.169230769230769,
-0.153846153846154,-0.138461538461538,-0.123076923076923,-0.107692307692308,
-0.0923076923076923,-0.0769230769230769,-0.0615384615384615,-0.0461538461538462,
-0.0307692307692308,-0.0153846153846154,0.),.UNSPECIFIED.)
CURVE()
GEOMETRIC_REPRESENTATION_ITEM()
RATIONAL_B_SPLINE_CURVE((1.,1.,1.,1.,1.,1.,1.,1.,1.,1.,1.,1.,1.,1.,1.,1.,
1.,1.,1.,1.,1.,1.,1.,1.,1.,1.,1.,1.,1.,1.,1.,1.,1.,1.,1.,1.,1.,1.,1.,1.,
1.,1.,1.,1.,1.,1.,1.,1.,1.,1.,1.,1.,1.,1.,1.,1.,1.,1.,1.,1.,1.,1.,1.,1.,
1.,1.,1.,1.,1.,1.))
REPRESENTATION_ITEM('')
);
#178=(
BOUNDED_CURVE()
B_SPLINE_CURVE(5,(#26831,#26832,#26833,#26834,#26835,#26836,#26837,#26838,
#26839,#26840,#26841,#26842,#26843,#26844,#26845,#26846,#26847,#26848,#26849,
#26850,#26851,#26852,#26853,#26854,#26855,#26856,#26857,#26858,#26859,#26860,
#26861,#26862,#26863,#26864,#26865,#26866,#26867,#26868,#26869,#26870,#26871,
#26872,#26873,#26874,#26875,#26876,#26877,#26878,#26879,#26880,#26881,#26882,
#26883,#26884,#26885,#26886,#26887,#26888,#26889,#26890,#26891,#26892,#26893,
#26894,#26895,#26896,#26897,#26898,#26899,#26900),.UNSPECIFIED.,.F.,.F.)
B_SPLINE_CURVE_WITH_KNOTS((6,1,1,1,1,1,1,1,1,1,1,1,1,1,1,1,1,1,1,1,1,1,
1,1,1,1,1,1,1,1,1,1,1,1,1,1,1,1,1,1,1,1,1,1,1,1,1,1,1,1,1,1,1,1,1,1,1,1,
1,1,1,1,1,1,1,6),(-1.,-0.984615384615383,-0.969230769230768,-0.953846153846152,
-0.938461538461537,-0.923076923076922,-0.907692307692306,-0.892307692307691,
-0.876923076923076,-0.86153846153846,-0.846153846153845,-0.83076923076923,
-0.815384615384614,-0.799999999999999,-0.784615384615384,-0.769230769230768,
-0.753846153846153,-0.738461538461538,-0.723076923076922,-0.707692307692307,
-0.692307692307692,-0.676923076923076,-0.661538461538461,-0.646153846153846,
-0.63076923076923,-0.615384615384615,-0.6,-0.584615384615384,-0.569230769230769,
-0.553846153846154,-0.538461538461538,-0.523076923076923,-0.507692307692308,
-0.492307692307692,-0.476923076923077,-0.461538461538462,-0.446153846153846,
-0.430769230769231,-0.415384615384615,-0.4,-0.384615384615385,-0.369230769230769,
-0.353846153846154,-0.338461538461538,-0.323076923076923,-0.307692307692308,
-0.292307692307692,-0.276923076923077,-0.261538461538462,-0.246153846153846,
-0.230769230769231,-0.215384615384615,-0.2,-0.184615384615385,-0.169230769230769,
-0.153846153846154,-0.138461538461538,-0.123076923076923,-0.107692307692308,
-0.0923076923076923,-0.0769230769230769,-0.0615384615384615,-0.0461538461538462,
-0.0307692307692308,-0.0153846153846154,0.),.UNSPECIFIED.)
CURVE()
GEOMETRIC_REPRESENTATION_ITEM()
RATIONAL_B_SPLINE_CURVE((1.,1.,1.,1.,1.,1.,1.,1.,1.,1.,1.,1.,1.,1.,1.,1.,
1.,1.,1.,1.,1.,1.,1.,1.,1.,1.,1.,1.,1.,1.,1.,1.,1.,1.,1.,1.,1.,1.,1.,1.,
1.,1.,1.,1.,1.,1.,1.,1.,1.,1.,1.,1.,1.,1.,1.,1.,1.,1.,1.,1.,1.,1.,1.,1.,
1.,1.,1.,1.,1.,1.))
REPRESENTATION_ITEM('')
);
#179=(
BOUNDED_CURVE()
B_SPLINE_CURVE(5,(#27047,#27048,#27049,#27050,#27051,#27052,#27053,#27054,
#27055,#27056,#27057,#27058,#27059,#27060,#27061,#27062,#27063,#27064,#27065,
#27066,#27067,#27068,#27069,#27070,#27071,#27072,#27073,#27074,#27075,#27076,
#27077,#27078,#27079,#27080,#27081,#27082,#27083,#27084,#27085,#27086,#27087,
#27088,#27089,#27090,#27091,#27092,#27093,#27094,#27095,#27096,#27097,#27098,
#27099,#27100,#27101,#27102,#27103,#27104,#27105,#27106,#27107,#27108,#27109,
#27110,#27111,#27112,#27113,#27114,#27115,#27116),.UNSPECIFIED.,.F.,.F.)
B_SPLINE_CURVE_WITH_KNOTS((6,1,1,1,1,1,1,1,1,1,1,1,1,1,1,1,1,1,1,1,1,1,
1,1,1,1,1,1,1,1,1,1,1,1,1,1,1,1,1,1,1,1,1,1,1,1,1,1,1,1,1,1,1,1,1,1,1,1,
1,1,1,1,1,1,1,6),(-1.,-0.984615384615383,-0.969230769230768,-0.953846153846152,
-0.938461538461537,-0.923076923076922,-0.907692307692306,-0.892307692307691,
-0.876923076923076,-0.86153846153846,-0.846153846153845,-0.83076923076923,
-0.815384615384614,-0.799999999999999,-0.784615384615384,-0.769230769230768,
-0.753846153846153,-0.738461538461538,-0.723076923076922,-0.707692307692307,
-0.692307692307692,-0.676923076923076,-0.661538461538461,-0.646153846153846,
-0.63076923076923,-0.615384615384615,-0.6,-0.584615384615384,-0.569230769230769,
-0.553846153846154,-0.538461538461538,-0.523076923076923,-0.507692307692308,
-0.492307692307692,-0.476923076923077,-0.461538461538462,-0.446153846153846,
-0.430769230769231,-0.415384615384615,-0.4,-0.384615384615385,-0.369230769230769,
-0.353846153846154,-0.338461538461538,-0.323076923076923,-0.307692307692308,
-0.292307692307692,-0.276923076923077,-0.261538461538462,-0.246153846153846,
-0.230769230769231,-0.215384615384615,-0.2,-0.184615384615385,-0.169230769230769,
-0.153846153846154,-0.138461538461538,-0.123076923076923,-0.107692307692308,
-0.0923076923076923,-0.0769230769230769,-0.0615384615384615,-0.0461538461538462,
-0.0307692307692308,-0.0153846153846154,0.),.UNSPECIFIED.)
CURVE()
GEOMETRIC_REPRESENTATION_ITEM()
RATIONAL_B_SPLINE_CURVE((1.,1.,1.,1.,1.,1.,1.,1.,1.,1.,1.,1.,1.,1.,1.,1.,
1.,1.,1.,1.,1.,1.,1.,1.,1.,1.,1.,1.,1.,1.,1.,1.,1.,1.,1.,1.,1.,1.,1.,1.,
1.,1.,1.,1.,1.,1.,1.,1.,1.,1.,1.,1.,1.,1.,1.,1.,1.,1.,1.,1.,1.,1.,1.,1.,
1.,1.,1.,1.,1.,1.))
REPRESENTATION_ITEM('')
);
#180=(
BOUNDED_CURVE()
B_SPLINE_CURVE(5,(#27263,#27264,#27265,#27266,#27267,#27268,#27269,#27270,
#27271,#27272,#27273,#27274,#27275,#27276,#27277,#27278,#27279,#27280,#27281,
#27282,#27283,#27284,#27285,#27286,#27287,#27288,#27289,#27290,#27291,#27292,
#27293,#27294,#27295,#27296,#27297,#27298,#27299,#27300,#27301,#27302,#27303,
#27304,#27305,#27306,#27307,#27308,#27309,#27310,#27311,#27312,#27313,#27314,
#27315,#27316,#27317,#27318,#27319,#27320,#27321,#27322,#27323,#27324,#27325,
#27326,#27327,#27328,#27329,#27330,#27331,#27332),.UNSPECIFIED.,.F.,.F.)
B_SPLINE_CURVE_WITH_KNOTS((6,1,1,1,1,1,1,1,1,1,1,1,1,1,1,1,1,1,1,1,1,1,
1,1,1,1,1,1,1,1,1,1,1,1,1,1,1,1,1,1,1,1,1,1,1,1,1,1,1,1,1,1,1,1,1,1,1,1,
1,1,1,1,1,1,1,6),(-1.,-0.984615384615383,-0.969230769230768,-0.953846153846152,
-0.938461538461537,-0.923076923076922,-0.907692307692306,-0.892307692307691,
-0.876923076923076,-0.86153846153846,-0.846153846153845,-0.83076923076923,
-0.815384615384614,-0.799999999999999,-0.784615384615384,-0.769230769230768,
-0.753846153846153,-0.738461538461538,-0.723076923076922,-0.707692307692307,
-0.692307692307692,-0.676923076923076,-0.661538461538461,-0.646153846153846,
-0.63076923076923,-0.615384615384615,-0.6,-0.584615384615384,-0.569230769230769,
-0.553846153846154,-0.538461538461538,-0.523076923076923,-0.507692307692308,
-0.492307692307692,-0.476923076923077,-0.461538461538462,-0.446153846153846,
-0.430769230769231,-0.415384615384615,-0.4,-0.384615384615385,-0.369230769230769,
-0.353846153846154,-0.338461538461538,-0.323076923076923,-0.307692307692308,
-0.292307692307692,-0.276923076923077,-0.261538461538462,-0.246153846153846,
-0.230769230769231,-0.215384615384615,-0.2,-0.184615384615385,-0.169230769230769,
-0.153846153846154,-0.138461538461538,-0.123076923076923,-0.107692307692308,
-0.0923076923076923,-0.0769230769230769,-0.0615384615384615,-0.0461538461538462,
-0.0307692307692308,-0.0153846153846154,0.),.UNSPECIFIED.)
CURVE()
GEOMETRIC_REPRESENTATION_ITEM()
RATIONAL_B_SPLINE_CURVE((1.,1.,1.,1.,1.,1.,1.,1.,1.,1.,1.,1.,1.,1.,1.,1.,
1.,1.,1.,1.,1.,1.,1.,1.,1.,1.,1.,1.,1.,1.,1.,1.,1.,1.,1.,1.,1.,1.,1.,1.,
1.,1.,1.,1.,1.,1.,1.,1.,1.,1.,1.,1.,1.,1.,1.,1.,1.,1.,1.,1.,1.,1.,1.,1.,
1.,1.,1.,1.,1.,1.))
REPRESENTATION_ITEM('')
);
#181=(
BOUNDED_CURVE()
B_SPLINE_CURVE(5,(#27479,#27480,#27481,#27482,#27483,#27484,#27485,#27486,
#27487,#27488,#27489,#27490,#27491,#27492,#27493,#27494,#27495,#27496,#27497,
#27498,#27499,#27500,#27501,#27502,#27503,#27504,#27505,#27506,#27507,#27508,
#27509,#27510,#27511,#27512,#27513,#27514,#27515,#27516,#27517,#27518,#27519,
#27520,#27521,#27522,#27523,#27524,#27525,#27526,#27527,#27528,#27529,#27530,
#27531,#27532,#27533,#27534,#27535,#27536,#27537,#27538,#27539,#27540,#27541,
#27542,#27543,#27544,#27545,#27546,#27547,#27548),.UNSPECIFIED.,.F.,.F.)
B_SPLINE_CURVE_WITH_KNOTS((6,1,1,1,1,1,1,1,1,1,1,1,1,1,1,1,1,1,1,1,1,1,
1,1,1,1,1,1,1,1,1,1,1,1,1,1,1,1,1,1,1,1,1,1,1,1,1,1,1,1,1,1,1,1,1,1,1,1,
1,1,1,1,1,1,1,6),(-1.,-0.984615384615383,-0.969230769230768,-0.953846153846152,
-0.938461538461537,-0.923076923076922,-0.907692307692306,-0.892307692307691,
-0.876923076923076,-0.86153846153846,-0.846153846153845,-0.83076923076923,
-0.815384615384614,-0.799999999999999,-0.784615384615384,-0.769230769230768,
-0.753846153846153,-0.738461538461538,-0.723076923076922,-0.707692307692307,
-0.692307692307692,-0.676923076923076,-0.661538461538461,-0.646153846153846,
-0.63076923076923,-0.615384615384615,-0.6,-0.584615384615384,-0.569230769230769,
-0.553846153846154,-0.538461538461538,-0.523076923076923,-0.507692307692308,
-0.492307692307692,-0.476923076923077,-0.461538461538462,-0.446153846153846,
-0.430769230769231,-0.415384615384615,-0.4,-0.384615384615385,-0.369230769230769,
-0.353846153846154,-0.338461538461538,-0.323076923076923,-0.307692307692308,
-0.292307692307692,-0.276923076923077,-0.261538461538462,-0.246153846153846,
-0.230769230769231,-0.215384615384615,-0.2,-0.184615384615385,-0.169230769230769,
-0.153846153846154,-0.138461538461538,-0.123076923076923,-0.107692307692308,
-0.0923076923076923,-0.0769230769230769,-0.0615384615384615,-0.0461538461538462,
-0.0307692307692308,-0.0153846153846154,0.),.UNSPECIFIED.)
CURVE()
GEOMETRIC_REPRESENTATION_ITEM()
RATIONAL_B_SPLINE_CURVE((1.,1.,1.,1.,1.,1.,1.,1.,1.,1.,1.,1.,1.,1.,1.,1.,
1.,1.,1.,1.,1.,1.,1.,1.,1.,1.,1.,1.,1.,1.,1.,1.,1.,1.,1.,1.,1.,1.,1.,1.,
1.,1.,1.,1.,1.,1.,1.,1.,1.,1.,1.,1.,1.,1.,1.,1.,1.,1.,1.,1.,1.,1.,1.,1.,
1.,1.,1.,1.,1.,1.))
REPRESENTATION_ITEM('')
);
#182=(
BOUNDED_CURVE()
B_SPLINE_CURVE(5,(#27695,#27696,#27697,#27698,#27699,#27700,#27701,#27702,
#27703,#27704,#27705,#27706,#27707,#27708,#27709,#27710,#27711,#27712,#27713,
#27714,#27715,#27716,#27717,#27718,#27719,#27720,#27721,#27722,#27723,#27724,
#27725,#27726,#27727,#27728,#27729,#27730,#27731,#27732,#27733,#27734,#27735,
#27736,#27737,#27738,#27739,#27740,#27741,#27742,#27743,#27744,#27745,#27746,
#27747,#27748,#27749,#27750,#27751,#27752,#27753,#27754,#27755,#27756,#27757,
#27758,#27759,#27760,#27761,#27762,#27763,#27764),.UNSPECIFIED.,.F.,.F.)
B_SPLINE_CURVE_WITH_KNOTS((6,1,1,1,1,1,1,1,1,1,1,1,1,1,1,1,1,1,1,1,1,1,
1,1,1,1,1,1,1,1,1,1,1,1,1,1,1,1,1,1,1,1,1,1,1,1,1,1,1,1,1,1,1,1,1,1,1,1,
1,1,1,1,1,1,1,6),(-1.,-0.984615384615383,-0.969230769230768,-0.953846153846152,
-0.938461538461537,-0.923076923076922,-0.907692307692306,-0.892307692307691,
-0.876923076923076,-0.86153846153846,-0.846153846153845,-0.83076923076923,
-0.815384615384614,-0.799999999999999,-0.784615384615384,-0.769230769230768,
-0.753846153846153,-0.738461538461538,-0.723076923076922,-0.707692307692307,
-0.692307692307692,-0.676923076923076,-0.661538461538461,-0.646153846153846,
-0.63076923076923,-0.615384615384615,-0.6,-0.584615384615384,-0.569230769230769,
-0.553846153846154,-0.538461538461538,-0.523076923076923,-0.507692307692308,
-0.492307692307692,-0.476923076923077,-0.461538461538462,-0.446153846153846,
-0.430769230769231,-0.415384615384615,-0.4,-0.384615384615385,-0.369230769230769,
-0.353846153846154,-0.338461538461538,-0.323076923076923,-0.307692307692308,
-0.292307692307692,-0.276923076923077,-0.261538461538462,-0.246153846153846,
-0.230769230769231,-0.215384615384615,-0.2,-0.184615384615385,-0.169230769230769,
-0.153846153846154,-0.138461538461538,-0.123076923076923,-0.107692307692308,
-0.0923076923076923,-0.0769230769230769,-0.0615384615384615,-0.0461538461538462,
-0.0307692307692308,-0.0153846153846154,0.),.UNSPECIFIED.)
CURVE()
GEOMETRIC_REPRESENTATION_ITEM()
RATIONAL_B_SPLINE_CURVE((1.,1.,1.,1.,1.,1.,1.,1.,1.,1.,1.,1.,1.,1.,1.,1.,
1.,1.,1.,1.,1.,1.,1.,1.,1.,1.,1.,1.,1.,1.,1.,1.,1.,1.,1.,1.,1.,1.,1.,1.,
1.,1.,1.,1.,1.,1.,1.,1.,1.,1.,1.,1.,1.,1.,1.,1.,1.,1.,1.,1.,1.,1.,1.,1.,
1.,1.,1.,1.,1.,1.))
REPRESENTATION_ITEM('')
);
#183=(
BOUNDED_CURVE()
B_SPLINE_CURVE(5,(#27911,#27912,#27913,#27914,#27915,#27916,#27917,#27918,
#27919,#27920,#27921,#27922,#27923,#27924,#27925,#27926,#27927,#27928,#27929,
#27930,#27931,#27932,#27933,#27934,#27935,#27936,#27937,#27938,#27939,#27940,
#27941,#27942,#27943,#27944,#27945,#27946,#27947,#27948,#27949,#27950,#27951,
#27952,#27953,#27954,#27955,#27956,#27957,#27958,#27959,#27960,#27961,#27962,
#27963,#27964,#27965,#27966,#27967,#27968,#27969,#27970,#27971,#27972,#27973,
#27974,#27975,#27976,#27977,#27978,#27979,#27980),.UNSPECIFIED.,.F.,.F.)
B_SPLINE_CURVE_WITH_KNOTS((6,1,1,1,1,1,1,1,1,1,1,1,1,1,1,1,1,1,1,1,1,1,
1,1,1,1,1,1,1,1,1,1,1,1,1,1,1,1,1,1,1,1,1,1,1,1,1,1,1,1,1,1,1,1,1,1,1,1,
1,1,1,1,1,1,1,6),(-1.,-0.984615384615383,-0.969230769230768,-0.953846153846152,
-0.938461538461537,-0.923076923076922,-0.907692307692306,-0.892307692307691,
-0.876923076923076,-0.86153846153846,-0.846153846153845,-0.83076923076923,
-0.815384615384614,-0.799999999999999,-0.784615384615384,-0.769230769230768,
-0.753846153846153,-0.738461538461538,-0.723076923076922,-0.707692307692307,
-0.692307692307692,-0.676923076923076,-0.661538461538461,-0.646153846153846,
-0.63076923076923,-0.615384615384615,-0.6,-0.584615384615384,-0.569230769230769,
-0.553846153846154,-0.538461538461538,-0.523076923076923,-0.507692307692308,
-0.492307692307692,-0.476923076923077,-0.461538461538462,-0.446153846153846,
-0.430769230769231,-0.415384615384615,-0.4,-0.384615384615385,-0.369230769230769,
-0.353846153846154,-0.338461538461538,-0.323076923076923,-0.307692307692308,
-0.292307692307692,-0.276923076923077,-0.261538461538462,-0.246153846153846,
-0.230769230769231,-0.215384615384615,-0.2,-0.184615384615385,-0.169230769230769,
-0.153846153846154,-0.138461538461538,-0.123076923076923,-0.107692307692308,
-0.0923076923076923,-0.0769230769230769,-0.0615384615384615,-0.0461538461538462,
-0.0307692307692308,-0.0153846153846154,0.),.UNSPECIFIED.)
CURVE()
GEOMETRIC_REPRESENTATION_ITEM()
RATIONAL_B_SPLINE_CURVE((1.,1.,1.,1.,1.,1.,1.,1.,1.,1.,1.,1.,1.,1.,1.,1.,
1.,1.,1.,1.,1.,1.,1.,1.,1.,1.,1.,1.,1.,1.,1.,1.,1.,1.,1.,1.,1.,1.,1.,1.,
1.,1.,1.,1.,1.,1.,1.,1.,1.,1.,1.,1.,1.,1.,1.,1.,1.,1.,1.,1.,1.,1.,1.,1.,
1.,1.,1.,1.,1.,1.))
REPRESENTATION_ITEM('')
);
#184=(
BOUNDED_CURVE()
B_SPLINE_CURVE(5,(#28127,#28128,#28129,#28130,#28131,#28132,#28133,#28134,
#28135,#28136,#28137,#28138,#28139,#28140,#28141,#28142,#28143,#28144,#28145,
#28146,#28147,#28148,#28149,#28150,#28151,#28152,#28153,#28154,#28155,#28156,
#28157,#28158,#28159,#28160,#28161,#28162,#28163,#28164,#28165,#28166,#28167,
#28168,#28169,#28170,#28171,#28172,#28173,#28174,#28175,#28176,#28177,#28178,
#28179,#28180,#28181,#28182,#28183,#28184,#28185,#28186,#28187,#28188,#28189,
#28190,#28191,#28192,#28193,#28194,#28195,#28196),.UNSPECIFIED.,.F.,.F.)
B_SPLINE_CURVE_WITH_KNOTS((6,1,1,1,1,1,1,1,1,1,1,1,1,1,1,1,1,1,1,1,1,1,
1,1,1,1,1,1,1,1,1,1,1,1,1,1,1,1,1,1,1,1,1,1,1,1,1,1,1,1,1,1,1,1,1,1,1,1,
1,1,1,1,1,1,1,6),(-1.,-0.984615384615383,-0.969230769230768,-0.953846153846152,
-0.938461538461537,-0.923076923076922,-0.907692307692306,-0.892307692307691,
-0.876923076923076,-0.86153846153846,-0.846153846153845,-0.83076923076923,
-0.815384615384614,-0.799999999999999,-0.784615384615384,-0.769230769230768,
-0.753846153846153,-0.738461538461538,-0.723076923076922,-0.707692307692307,
-0.692307692307692,-0.676923076923076,-0.661538461538461,-0.646153846153846,
-0.63076923076923,-0.615384615384615,-0.6,-0.584615384615384,-0.569230769230769,
-0.553846153846154,-0.538461538461538,-0.523076923076923,-0.507692307692308,
-0.492307692307692,-0.476923076923077,-0.461538461538462,-0.446153846153846,
-0.430769230769231,-0.415384615384615,-0.4,-0.384615384615385,-0.369230769230769,
-0.353846153846154,-0.338461538461538,-0.323076923076923,-0.307692307692308,
-0.292307692307692,-0.276923076923077,-0.261538461538462,-0.246153846153846,
-0.230769230769231,-0.215384615384615,-0.2,-0.184615384615385,-0.169230769230769,
-0.153846153846154,-0.138461538461538,-0.123076923076923,-0.107692307692308,
-0.0923076923076923,-0.0769230769230769,-0.0615384615384615,-0.0461538461538462,
-0.0307692307692308,-0.0153846153846154,0.),.UNSPECIFIED.)
CURVE()
GEOMETRIC_REPRESENTATION_ITEM()
RATIONAL_B_SPLINE_CURVE((1.,1.,1.,1.,1.,1.,1.,1.,1.,1.,1.,1.,1.,1.,1.,1.,
1.,1.,1.,1.,1.,1.,1.,1.,1.,1.,1.,1.,1.,1.,1.,1.,1.,1.,1.,1.,1.,1.,1.,1.,
1.,1.,1.,1.,1.,1.,1.,1.,1.,1.,1.,1.,1.,1.,1.,1.,1.,1.,1.,1.,1.,1.,1.,1.,
1.,1.,1.,1.,1.,1.))
REPRESENTATION_ITEM('')
);
#185=(
BOUNDED_CURVE()
B_SPLINE_CURVE(5,(#28343,#28344,#28345,#28346,#28347,#28348,#28349,#28350,
#28351,#28352,#28353,#28354,#28355,#28356,#28357,#28358,#28359,#28360,#28361,
#28362,#28363,#28364,#28365,#28366,#28367,#28368,#28369,#28370,#28371,#28372,
#28373,#28374,#28375,#28376,#28377,#28378,#28379,#28380,#28381,#28382,#28383,
#28384,#28385,#28386,#28387,#28388,#28389,#28390,#28391,#28392,#28393,#28394,
#28395,#28396,#28397,#28398,#28399,#28400,#28401,#28402,#28403,#28404,#28405,
#28406,#28407,#28408,#28409,#28410,#28411,#28412),.UNSPECIFIED.,.F.,.F.)
B_SPLINE_CURVE_WITH_KNOTS((6,1,1,1,1,1,1,1,1,1,1,1,1,1,1,1,1,1,1,1,1,1,
1,1,1,1,1,1,1,1,1,1,1,1,1,1,1,1,1,1,1,1,1,1,1,1,1,1,1,1,1,1,1,1,1,1,1,1,
1,1,1,1,1,1,1,6),(-1.,-0.984615384615383,-0.969230769230768,-0.953846153846152,
-0.938461538461537,-0.923076923076922,-0.907692307692306,-0.892307692307691,
-0.876923076923076,-0.86153846153846,-0.846153846153845,-0.83076923076923,
-0.815384615384614,-0.799999999999999,-0.784615384615384,-0.769230769230768,
-0.753846153846153,-0.738461538461538,-0.723076923076922,-0.707692307692307,
-0.692307692307692,-0.676923076923076,-0.661538461538461,-0.646153846153846,
-0.63076923076923,-0.615384615384615,-0.6,-0.584615384615384,-0.569230769230769,
-0.553846153846154,-0.538461538461538,-0.523076923076923,-0.507692307692308,
-0.492307692307692,-0.476923076923077,-0.461538461538462,-0.446153846153846,
-0.430769230769231,-0.415384615384615,-0.4,-0.384615384615385,-0.369230769230769,
-0.353846153846154,-0.338461538461538,-0.323076923076923,-0.307692307692308,
-0.292307692307692,-0.276923076923077,-0.261538461538462,-0.246153846153846,
-0.230769230769231,-0.215384615384615,-0.2,-0.184615384615385,-0.169230769230769,
-0.153846153846154,-0.138461538461538,-0.123076923076923,-0.107692307692308,
-0.0923076923076923,-0.0769230769230769,-0.0615384615384615,-0.0461538461538462,
-0.0307692307692308,-0.0153846153846154,0.),.UNSPECIFIED.)
CURVE()
GEOMETRIC_REPRESENTATION_ITEM()
RATIONAL_B_SPLINE_CURVE((1.,1.,1.,1.,1.,1.,1.,1.,1.,1.,1.,1.,1.,1.,1.,1.,
1.,1.,1.,1.,1.,1.,1.,1.,1.,1.,1.,1.,1.,1.,1.,1.,1.,1.,1.,1.,1.,1.,1.,1.,
1.,1.,1.,1.,1.,1.,1.,1.,1.,1.,1.,1.,1.,1.,1.,1.,1.,1.,1.,1.,1.,1.,1.,1.,
1.,1.,1.,1.,1.,1.))
REPRESENTATION_ITEM('')
);
#186=(
BOUNDED_CURVE()
B_SPLINE_CURVE(5,(#28559,#28560,#28561,#28562,#28563,#28564,#28565,#28566,
#28567,#28568,#28569,#28570,#28571,#28572,#28573,#28574,#28575,#28576,#28577,
#28578,#28579,#28580,#28581,#28582,#28583,#28584,#28585,#28586,#28587,#28588,
#28589,#28590,#28591,#28592,#28593,#28594,#28595,#28596,#28597,#28598,#28599,
#28600,#28601,#28602,#28603,#28604,#28605,#28606,#28607,#28608,#28609,#28610,
#28611,#28612,#28613,#28614,#28615,#28616,#28617,#28618,#28619,#28620,#28621,
#28622,#28623,#28624,#28625,#28626,#28627,#28628),.UNSPECIFIED.,.F.,.F.)
B_SPLINE_CURVE_WITH_KNOTS((6,1,1,1,1,1,1,1,1,1,1,1,1,1,1,1,1,1,1,1,1,1,
1,1,1,1,1,1,1,1,1,1,1,1,1,1,1,1,1,1,1,1,1,1,1,1,1,1,1,1,1,1,1,1,1,1,1,1,
1,1,1,1,1,1,1,6),(-1.,-0.984615384615383,-0.969230769230768,-0.953846153846152,
-0.938461538461537,-0.923076923076922,-0.907692307692306,-0.892307692307691,
-0.876923076923076,-0.86153846153846,-0.846153846153845,-0.83076923076923,
-0.815384615384614,-0.799999999999999,-0.784615384615384,-0.769230769230768,
-0.753846153846153,-0.738461538461538,-0.723076923076922,-0.707692307692307,
-0.692307692307692,-0.676923076923076,-0.661538461538461,-0.646153846153846,
-0.63076923076923,-0.615384615384615,-0.6,-0.584615384615384,-0.569230769230769,
-0.553846153846154,-0.538461538461538,-0.523076923076923,-0.507692307692308,
-0.492307692307692,-0.476923076923077,-0.461538461538462,-0.446153846153846,
-0.430769230769231,-0.415384615384615,-0.4,-0.384615384615385,-0.369230769230769,
-0.353846153846154,-0.338461538461538,-0.323076923076923,-0.307692307692308,
-0.292307692307692,-0.276923076923077,-0.261538461538462,-0.246153846153846,
-0.230769230769231,-0.215384615384615,-0.2,-0.184615384615385,-0.169230769230769,
-0.153846153846154,-0.138461538461538,-0.123076923076923,-0.107692307692308,
-0.0923076923076923,-0.0769230769230769,-0.0615384615384615,-0.0461538461538462,
-0.0307692307692308,-0.0153846153846154,0.),.UNSPECIFIED.)
CURVE()
GEOMETRIC_REPRESENTATION_ITEM()
RATIONAL_B_SPLINE_CURVE((1.,1.,1.,1.,1.,1.,1.,1.,1.,1.,1.,1.,1.,1.,1.,1.,
1.,1.,1.,1.,1.,1.,1.,1.,1.,1.,1.,1.,1.,1.,1.,1.,1.,1.,1.,1.,1.,1.,1.,1.,
1.,1.,1.,1.,1.,1.,1.,1.,1.,1.,1.,1.,1.,1.,1.,1.,1.,1.,1.,1.,1.,1.,1.,1.,
1.,1.,1.,1.,1.,1.))
REPRESENTATION_ITEM('')
);
#187=(
BOUNDED_CURVE()
B_SPLINE_CURVE(5,(#28775,#28776,#28777,#28778,#28779,#28780,#28781,#28782,
#28783,#28784,#28785,#28786,#28787,#28788,#28789,#28790,#28791,#28792,#28793,
#28794,#28795,#28796,#28797,#28798,#28799,#28800,#28801,#28802,#28803,#28804,
#28805,#28806,#28807,#28808,#28809,#28810,#28811,#28812,#28813,#28814,#28815,
#28816,#28817,#28818,#28819,#28820,#28821,#28822,#28823,#28824,#28825,#28826,
#28827,#28828,#28829,#28830,#28831,#28832,#28833,#28834,#28835,#28836,#28837,
#28838,#28839,#28840,#28841,#28842,#28843,#28844),.UNSPECIFIED.,.F.,.F.)
B_SPLINE_CURVE_WITH_KNOTS((6,1,1,1,1,1,1,1,1,1,1,1,1,1,1,1,1,1,1,1,1,1,
1,1,1,1,1,1,1,1,1,1,1,1,1,1,1,1,1,1,1,1,1,1,1,1,1,1,1,1,1,1,1,1,1,1,1,1,
1,1,1,1,1,1,1,6),(-1.,-0.984615384615383,-0.969230769230768,-0.953846153846152,
-0.938461538461537,-0.923076923076922,-0.907692307692306,-0.892307692307691,
-0.876923076923076,-0.86153846153846,-0.846153846153845,-0.83076923076923,
-0.815384615384614,-0.799999999999999,-0.784615384615384,-0.769230769230768,
-0.753846153846153,-0.738461538461538,-0.723076923076922,-0.707692307692307,
-0.692307692307692,-0.676923076923076,-0.661538461538461,-0.646153846153846,
-0.63076923076923,-0.615384615384615,-0.6,-0.584615384615384,-0.569230769230769,
-0.553846153846154,-0.538461538461538,-0.523076923076923,-0.507692307692308,
-0.492307692307692,-0.476923076923077,-0.461538461538462,-0.446153846153846,
-0.430769230769231,-0.415384615384615,-0.4,-0.384615384615385,-0.369230769230769,
-0.353846153846154,-0.338461538461538,-0.323076923076923,-0.307692307692308,
-0.292307692307692,-0.276923076923077,-0.261538461538462,-0.246153846153846,
-0.230769230769231,-0.215384615384615,-0.2,-0.184615384615385,-0.169230769230769,
-0.153846153846154,-0.138461538461538,-0.123076923076923,-0.107692307692308,
-0.0923076923076923,-0.0769230769230769,-0.0615384615384615,-0.0461538461538462,
-0.0307692307692308,-0.0153846153846154,0.),.UNSPECIFIED.)
CURVE()
GEOMETRIC_REPRESENTATION_ITEM()
RATIONAL_B_SPLINE_CURVE((1.,1.,1.,1.,1.,1.,1.,1.,1.,1.,1.,1.,1.,1.,1.,1.,
1.,1.,1.,1.,1.,1.,1.,1.,1.,1.,1.,1.,1.,1.,1.,1.,1.,1.,1.,1.,1.,1.,1.,1.,
1.,1.,1.,1.,1.,1.,1.,1.,1.,1.,1.,1.,1.,1.,1.,1.,1.,1.,1.,1.,1.,1.,1.,1.,
1.,1.,1.,1.,1.,1.))
REPRESENTATION_ITEM('')
);
#188=(
BOUNDED_CURVE()
B_SPLINE_CURVE(5,(#28991,#28992,#28993,#28994,#28995,#28996,#28997,#28998,
#28999,#29000,#29001,#29002,#29003,#29004,#29005,#29006,#29007,#29008,#29009,
#29010,#29011,#29012,#29013,#29014,#29015,#29016,#29017,#29018,#29019,#29020,
#29021,#29022,#29023,#29024,#29025,#29026,#29027,#29028,#29029,#29030,#29031,
#29032,#29033,#29034,#29035,#29036,#29037,#29038,#29039,#29040,#29041,#29042,
#29043,#29044,#29045,#29046,#29047,#29048,#29049,#29050,#29051,#29052,#29053,
#29054,#29055,#29056,#29057,#29058,#29059,#29060),.UNSPECIFIED.,.F.,.F.)
B_SPLINE_CURVE_WITH_KNOTS((6,1,1,1,1,1,1,1,1,1,1,1,1,1,1,1,1,1,1,1,1,1,
1,1,1,1,1,1,1,1,1,1,1,1,1,1,1,1,1,1,1,1,1,1,1,1,1,1,1,1,1,1,1,1,1,1,1,1,
1,1,1,1,1,1,1,6),(-1.,-0.984615384615383,-0.969230769230768,-0.953846153846152,
-0.938461538461537,-0.923076923076922,-0.907692307692306,-0.892307692307691,
-0.876923076923076,-0.86153846153846,-0.846153846153845,-0.83076923076923,
-0.815384615384614,-0.799999999999999,-0.784615384615384,-0.769230769230768,
-0.753846153846153,-0.738461538461538,-0.723076923076922,-0.707692307692307,
-0.692307692307692,-0.676923076923076,-0.661538461538461,-0.646153846153846,
-0.63076923076923,-0.615384615384615,-0.6,-0.584615384615384,-0.569230769230769,
-0.553846153846154,-0.538461538461538,-0.523076923076923,-0.507692307692308,
-0.492307692307692,-0.476923076923077,-0.461538461538462,-0.446153846153846,
-0.430769230769231,-0.415384615384615,-0.4,-0.384615384615385,-0.369230769230769,
-0.353846153846154,-0.338461538461538,-0.323076923076923,-0.307692307692308,
-0.292307692307692,-0.276923076923077,-0.261538461538462,-0.246153846153846,
-0.230769230769231,-0.215384615384615,-0.2,-0.184615384615385,-0.169230769230769,
-0.153846153846154,-0.138461538461538,-0.123076923076923,-0.107692307692308,
-0.0923076923076923,-0.0769230769230769,-0.0615384615384615,-0.0461538461538462,
-0.0307692307692308,-0.0153846153846154,0.),.UNSPECIFIED.)
CURVE()
GEOMETRIC_REPRESENTATION_ITEM()
RATIONAL_B_SPLINE_CURVE((1.,1.,1.,1.,1.,1.,1.,1.,1.,1.,1.,1.,1.,1.,1.,1.,
1.,1.,1.,1.,1.,1.,1.,1.,1.,1.,1.,1.,1.,1.,1.,1.,1.,1.,1.,1.,1.,1.,1.,1.,
1.,1.,1.,1.,1.,1.,1.,1.,1.,1.,1.,1.,1.,1.,1.,1.,1.,1.,1.,1.,1.,1.,1.,1.,
1.,1.,1.,1.,1.,1.))
REPRESENTATION_ITEM('')
);
#189=(
BOUNDED_CURVE()
B_SPLINE_CURVE(5,(#29207,#29208,#29209,#29210,#29211,#29212,#29213,#29214,
#29215,#29216,#29217,#29218,#29219,#29220,#29221,#29222,#29223,#29224,#29225,
#29226,#29227,#29228,#29229,#29230,#29231,#29232,#29233,#29234,#29235,#29236,
#29237,#29238,#29239,#29240,#29241,#29242,#29243,#29244,#29245,#29246,#29247,
#29248,#29249,#29250,#29251,#29252,#29253,#29254,#29255,#29256,#29257,#29258,
#29259,#29260,#29261,#29262,#29263,#29264,#29265,#29266,#29267,#29268,#29269,
#29270,#29271,#29272,#29273,#29274,#29275,#29276),.UNSPECIFIED.,.F.,.F.)
B_SPLINE_CURVE_WITH_KNOTS((6,1,1,1,1,1,1,1,1,1,1,1,1,1,1,1,1,1,1,1,1,1,
1,1,1,1,1,1,1,1,1,1,1,1,1,1,1,1,1,1,1,1,1,1,1,1,1,1,1,1,1,1,1,1,1,1,1,1,
1,1,1,1,1,1,1,6),(-1.,-0.984615384615383,-0.969230769230768,-0.953846153846152,
-0.938461538461537,-0.923076923076922,-0.907692307692306,-0.892307692307691,
-0.876923076923076,-0.86153846153846,-0.846153846153845,-0.83076923076923,
-0.815384615384614,-0.799999999999999,-0.784615384615384,-0.769230769230768,
-0.753846153846153,-0.738461538461538,-0.723076923076922,-0.707692307692307,
-0.692307692307692,-0.676923076923076,-0.661538461538461,-0.646153846153846,
-0.63076923076923,-0.615384615384615,-0.6,-0.584615384615384,-0.569230769230769,
-0.553846153846154,-0.538461538461538,-0.523076923076923,-0.507692307692308,
-0.492307692307692,-0.476923076923077,-0.461538461538462,-0.446153846153846,
-0.430769230769231,-0.415384615384615,-0.4,-0.384615384615385,-0.369230769230769,
-0.353846153846154,-0.338461538461538,-0.323076923076923,-0.307692307692308,
-0.292307692307692,-0.276923076923077,-0.261538461538462,-0.246153846153846,
-0.230769230769231,-0.215384615384615,-0.2,-0.184615384615385,-0.169230769230769,
-0.153846153846154,-0.138461538461538,-0.123076923076923,-0.107692307692308,
-0.0923076923076923,-0.0769230769230769,-0.0615384615384615,-0.0461538461538462,
-0.0307692307692308,-0.0153846153846154,0.),.UNSPECIFIED.)
CURVE()
GEOMETRIC_REPRESENTATION_ITEM()
RATIONAL_B_SPLINE_CURVE((1.,1.,1.,1.,1.,1.,1.,1.,1.,1.,1.,1.,1.,1.,1.,1.,
1.,1.,1.,1.,1.,1.,1.,1.,1.,1.,1.,1.,1.,1.,1.,1.,1.,1.,1.,1.,1.,1.,1.,1.,
1.,1.,1.,1.,1.,1.,1.,1.,1.,1.,1.,1.,1.,1.,1.,1.,1.,1.,1.,1.,1.,1.,1.,1.,
1.,1.,1.,1.,1.,1.))
REPRESENTATION_ITEM('')
);
#190=(
BOUNDED_CURVE()
B_SPLINE_CURVE(5,(#29423,#29424,#29425,#29426,#29427,#29428,#29429,#29430,
#29431,#29432,#29433,#29434,#29435,#29436,#29437,#29438,#29439,#29440,#29441,
#29442,#29443,#29444,#29445,#29446,#29447,#29448,#29449,#29450,#29451,#29452,
#29453,#29454,#29455,#29456,#29457,#29458,#29459,#29460,#29461,#29462,#29463,
#29464,#29465,#29466,#29467,#29468,#29469,#29470,#29471,#29472,#29473,#29474,
#29475,#29476,#29477,#29478,#29479,#29480,#29481,#29482,#29483,#29484,#29485,
#29486,#29487,#29488,#29489,#29490,#29491,#29492),.UNSPECIFIED.,.F.,.F.)
B_SPLINE_CURVE_WITH_KNOTS((6,1,1,1,1,1,1,1,1,1,1,1,1,1,1,1,1,1,1,1,1,1,
1,1,1,1,1,1,1,1,1,1,1,1,1,1,1,1,1,1,1,1,1,1,1,1,1,1,1,1,1,1,1,1,1,1,1,1,
1,1,1,1,1,1,1,6),(-1.,-0.984615384615383,-0.969230769230768,-0.953846153846152,
-0.938461538461537,-0.923076923076922,-0.907692307692306,-0.892307692307691,
-0.876923076923076,-0.86153846153846,-0.846153846153845,-0.83076923076923,
-0.815384615384614,-0.799999999999999,-0.784615384615384,-0.769230769230768,
-0.753846153846153,-0.738461538461538,-0.723076923076922,-0.707692307692307,
-0.692307692307692,-0.676923076923076,-0.661538461538461,-0.646153846153846,
-0.63076923076923,-0.615384615384615,-0.6,-0.584615384615384,-0.569230769230769,
-0.553846153846154,-0.538461538461538,-0.523076923076923,-0.507692307692308,
-0.492307692307692,-0.476923076923077,-0.461538461538462,-0.446153846153846,
-0.430769230769231,-0.415384615384615,-0.4,-0.384615384615385,-0.369230769230769,
-0.353846153846154,-0.338461538461538,-0.323076923076923,-0.307692307692308,
-0.292307692307692,-0.276923076923077,-0.261538461538462,-0.246153846153846,
-0.230769230769231,-0.215384615384615,-0.2,-0.184615384615385,-0.169230769230769,
-0.153846153846154,-0.138461538461538,-0.123076923076923,-0.107692307692308,
-0.0923076923076923,-0.0769230769230769,-0.0615384615384615,-0.0461538461538462,
-0.0307692307692308,-0.0153846153846154,0.),.UNSPECIFIED.)
CURVE()
GEOMETRIC_REPRESENTATION_ITEM()
RATIONAL_B_SPLINE_CURVE((1.,1.,1.,1.,1.,1.,1.,1.,1.,1.,1.,1.,1.,1.,1.,1.,
1.,1.,1.,1.,1.,1.,1.,1.,1.,1.,1.,1.,1.,1.,1.,1.,1.,1.,1.,1.,1.,1.,1.,1.,
1.,1.,1.,1.,1.,1.,1.,1.,1.,1.,1.,1.,1.,1.,1.,1.,1.,1.,1.,1.,1.,1.,1.,1.,
1.,1.,1.,1.,1.,1.))
REPRESENTATION_ITEM('')
);
#191=(
BOUNDED_CURVE()
B_SPLINE_CURVE(5,(#29639,#29640,#29641,#29642,#29643,#29644,#29645,#29646,
#29647,#29648,#29649,#29650,#29651,#29652,#29653,#29654,#29655,#29656,#29657,
#29658,#29659,#29660,#29661,#29662,#29663,#29664,#29665,#29666,#29667,#29668,
#29669,#29670,#29671,#29672,#29673,#29674,#29675,#29676,#29677,#29678,#29679,
#29680,#29681,#29682,#29683,#29684,#29685,#29686,#29687,#29688,#29689,#29690,
#29691,#29692,#29693,#29694,#29695,#29696,#29697,#29698,#29699,#29700,#29701,
#29702,#29703,#29704,#29705,#29706,#29707,#29708),.UNSPECIFIED.,.F.,.F.)
B_SPLINE_CURVE_WITH_KNOTS((6,1,1,1,1,1,1,1,1,1,1,1,1,1,1,1,1,1,1,1,1,1,
1,1,1,1,1,1,1,1,1,1,1,1,1,1,1,1,1,1,1,1,1,1,1,1,1,1,1,1,1,1,1,1,1,1,1,1,
1,1,1,1,1,1,1,6),(-1.,-0.984615384615383,-0.969230769230768,-0.953846153846152,
-0.938461538461537,-0.923076923076922,-0.907692307692306,-0.892307692307691,
-0.876923076923076,-0.86153846153846,-0.846153846153845,-0.83076923076923,
-0.815384615384614,-0.799999999999999,-0.784615384615384,-0.769230769230768,
-0.753846153846153,-0.738461538461538,-0.723076923076922,-0.707692307692307,
-0.692307692307692,-0.676923076923076,-0.661538461538461,-0.646153846153846,
-0.63076923076923,-0.615384615384615,-0.6,-0.584615384615384,-0.569230769230769,
-0.553846153846154,-0.538461538461538,-0.523076923076923,-0.507692307692308,
-0.492307692307692,-0.476923076923077,-0.461538461538462,-0.446153846153846,
-0.430769230769231,-0.415384615384615,-0.4,-0.384615384615385,-0.369230769230769,
-0.353846153846154,-0.338461538461538,-0.323076923076923,-0.307692307692308,
-0.292307692307692,-0.276923076923077,-0.261538461538462,-0.246153846153846,
-0.230769230769231,-0.215384615384615,-0.2,-0.184615384615385,-0.169230769230769,
-0.153846153846154,-0.138461538461538,-0.123076923076923,-0.107692307692308,
-0.0923076923076923,-0.0769230769230769,-0.0615384615384615,-0.0461538461538462,
-0.0307692307692308,-0.0153846153846154,0.),.UNSPECIFIED.)
CURVE()
GEOMETRIC_REPRESENTATION_ITEM()
RATIONAL_B_SPLINE_CURVE((1.,1.,1.,1.,1.,1.,1.,1.,1.,1.,1.,1.,1.,1.,1.,1.,
1.,1.,1.,1.,1.,1.,1.,1.,1.,1.,1.,1.,1.,1.,1.,1.,1.,1.,1.,1.,1.,1.,1.,1.,
1.,1.,1.,1.,1.,1.,1.,1.,1.,1.,1.,1.,1.,1.,1.,1.,1.,1.,1.,1.,1.,1.,1.,1.,
1.,1.,1.,1.,1.,1.))
REPRESENTATION_ITEM('')
);
#192=(
BOUNDED_CURVE()
B_SPLINE_CURVE(5,(#29855,#29856,#29857,#29858,#29859,#29860,#29861,#29862,
#29863,#29864,#29865,#29866,#29867,#29868,#29869,#29870,#29871,#29872,#29873,
#29874,#29875,#29876,#29877,#29878,#29879,#29880,#29881,#29882,#29883,#29884,
#29885,#29886,#29887,#29888,#29889,#29890,#29891,#29892,#29893,#29894,#29895,
#29896,#29897,#29898,#29899,#29900,#29901,#29902,#29903,#29904,#29905,#29906,
#29907,#29908,#29909,#29910,#29911,#29912,#29913,#29914,#29915,#29916,#29917,
#29918,#29919,#29920,#29921,#29922,#29923,#29924),.UNSPECIFIED.,.F.,.F.)
B_SPLINE_CURVE_WITH_KNOTS((6,1,1,1,1,1,1,1,1,1,1,1,1,1,1,1,1,1,1,1,1,1,
1,1,1,1,1,1,1,1,1,1,1,1,1,1,1,1,1,1,1,1,1,1,1,1,1,1,1,1,1,1,1,1,1,1,1,1,
1,1,1,1,1,1,1,6),(-1.,-0.984615384615383,-0.969230769230768,-0.953846153846152,
-0.938461538461537,-0.923076923076922,-0.907692307692306,-0.892307692307691,
-0.876923076923076,-0.86153846153846,-0.846153846153845,-0.83076923076923,
-0.815384615384614,-0.799999999999999,-0.784615384615384,-0.769230769230768,
-0.753846153846153,-0.738461538461538,-0.723076923076922,-0.707692307692307,
-0.692307692307692,-0.676923076923076,-0.661538461538461,-0.646153846153846,
-0.63076923076923,-0.615384615384615,-0.6,-0.584615384615384,-0.569230769230769,
-0.553846153846154,-0.538461538461538,-0.523076923076923,-0.507692307692308,
-0.492307692307692,-0.476923076923077,-0.461538461538462,-0.446153846153846,
-0.430769230769231,-0.415384615384615,-0.4,-0.384615384615385,-0.369230769230769,
-0.353846153846154,-0.338461538461538,-0.323076923076923,-0.307692307692308,
-0.292307692307692,-0.276923076923077,-0.261538461538462,-0.246153846153846,
-0.230769230769231,-0.215384615384615,-0.2,-0.184615384615385,-0.169230769230769,
-0.153846153846154,-0.138461538461538,-0.123076923076923,-0.107692307692308,
-0.0923076923076923,-0.0769230769230769,-0.0615384615384615,-0.0461538461538462,
-0.0307692307692308,-0.0153846153846154,0.),.UNSPECIFIED.)
CURVE()
GEOMETRIC_REPRESENTATION_ITEM()
RATIONAL_B_SPLINE_CURVE((1.,1.,1.,1.,1.,1.,1.,1.,1.,1.,1.,1.,1.,1.,1.,1.,
1.,1.,1.,1.,1.,1.,1.,1.,1.,1.,1.,1.,1.,1.,1.,1.,1.,1.,1.,1.,1.,1.,1.,1.,
1.,1.,1.,1.,1.,1.,1.,1.,1.,1.,1.,1.,1.,1.,1.,1.,1.,1.,1.,1.,1.,1.,1.,1.,
1.,1.,1.,1.,1.,1.))
REPRESENTATION_ITEM('')
);
#193=(
BOUNDED_CURVE()
B_SPLINE_CURVE(5,(#30071,#30072,#30073,#30074,#30075,#30076,#30077,#30078,
#30079,#30080,#30081,#30082,#30083,#30084,#30085,#30086,#30087,#30088,#30089,
#30090,#30091,#30092,#30093,#30094,#30095,#30096,#30097,#30098,#30099,#30100,
#30101,#30102,#30103,#30104,#30105,#30106,#30107,#30108,#30109,#30110,#30111,
#30112,#30113,#30114,#30115,#30116,#30117,#30118,#30119,#30120,#30121,#30122,
#30123,#30124,#30125,#30126,#30127,#30128,#30129,#30130,#30131,#30132,#30133,
#30134,#30135,#30136,#30137,#30138,#30139,#30140),.UNSPECIFIED.,.F.,.F.)
B_SPLINE_CURVE_WITH_KNOTS((6,1,1,1,1,1,1,1,1,1,1,1,1,1,1,1,1,1,1,1,1,1,
1,1,1,1,1,1,1,1,1,1,1,1,1,1,1,1,1,1,1,1,1,1,1,1,1,1,1,1,1,1,1,1,1,1,1,1,
1,1,1,1,1,1,1,6),(-1.,-0.984615384615383,-0.969230769230768,-0.953846153846152,
-0.938461538461537,-0.923076923076922,-0.907692307692306,-0.892307692307691,
-0.876923076923076,-0.86153846153846,-0.846153846153845,-0.83076923076923,
-0.815384615384614,-0.799999999999999,-0.784615384615384,-0.769230769230768,
-0.753846153846153,-0.738461538461538,-0.723076923076922,-0.707692307692307,
-0.692307692307692,-0.676923076923076,-0.661538461538461,-0.646153846153846,
-0.63076923076923,-0.615384615384615,-0.6,-0.584615384615384,-0.569230769230769,
-0.553846153846154,-0.538461538461538,-0.523076923076923,-0.507692307692308,
-0.492307692307692,-0.476923076923077,-0.461538461538462,-0.446153846153846,
-0.430769230769231,-0.415384615384615,-0.4,-0.384615384615385,-0.369230769230769,
-0.353846153846154,-0.338461538461538,-0.323076923076923,-0.307692307692308,
-0.292307692307692,-0.276923076923077,-0.261538461538462,-0.246153846153846,
-0.230769230769231,-0.215384615384615,-0.2,-0.184615384615385,-0.169230769230769,
-0.153846153846154,-0.138461538461538,-0.123076923076923,-0.107692307692308,
-0.0923076923076923,-0.0769230769230769,-0.0615384615384615,-0.0461538461538462,
-0.0307692307692308,-0.0153846153846154,0.),.UNSPECIFIED.)
CURVE()
GEOMETRIC_REPRESENTATION_ITEM()
RATIONAL_B_SPLINE_CURVE((1.,1.,1.,1.,1.,1.,1.,1.,1.,1.,1.,1.,1.,1.,1.,1.,
1.,1.,1.,1.,1.,1.,1.,1.,1.,1.,1.,1.,1.,1.,1.,1.,1.,1.,1.,1.,1.,1.,1.,1.,
1.,1.,1.,1.,1.,1.,1.,1.,1.,1.,1.,1.,1.,1.,1.,1.,1.,1.,1.,1.,1.,1.,1.,1.,
1.,1.,1.,1.,1.,1.))
REPRESENTATION_ITEM('')
);
#194=(
BOUNDED_CURVE()
B_SPLINE_CURVE(5,(#30287,#30288,#30289,#30290,#30291,#30292,#30293,#30294,
#30295,#30296,#30297,#30298,#30299,#30300,#30301,#30302,#30303,#30304,#30305,
#30306,#30307,#30308,#30309,#30310,#30311,#30312,#30313,#30314,#30315,#30316,
#30317,#30318,#30319,#30320,#30321,#30322,#30323,#30324,#30325,#30326,#30327,
#30328,#30329,#30330,#30331,#30332,#30333,#30334,#30335,#30336,#30337,#30338,
#30339,#30340,#30341,#30342,#30343,#30344,#30345,#30346,#30347,#30348,#30349,
#30350,#30351,#30352,#30353,#30354,#30355,#30356),.UNSPECIFIED.,.F.,.F.)
B_SPLINE_CURVE_WITH_KNOTS((6,1,1,1,1,1,1,1,1,1,1,1,1,1,1,1,1,1,1,1,1,1,
1,1,1,1,1,1,1,1,1,1,1,1,1,1,1,1,1,1,1,1,1,1,1,1,1,1,1,1,1,1,1,1,1,1,1,1,
1,1,1,1,1,1,1,6),(-1.,-0.984615384615383,-0.969230769230768,-0.953846153846152,
-0.938461538461537,-0.923076923076922,-0.907692307692306,-0.892307692307691,
-0.876923076923076,-0.86153846153846,-0.846153846153845,-0.83076923076923,
-0.815384615384614,-0.799999999999999,-0.784615384615384,-0.769230769230768,
-0.753846153846153,-0.738461538461538,-0.723076923076922,-0.707692307692307,
-0.692307692307692,-0.676923076923076,-0.661538461538461,-0.646153846153846,
-0.63076923076923,-0.615384615384615,-0.6,-0.584615384615384,-0.569230769230769,
-0.553846153846154,-0.538461538461538,-0.523076923076923,-0.507692307692308,
-0.492307692307692,-0.476923076923077,-0.461538461538462,-0.446153846153846,
-0.430769230769231,-0.415384615384615,-0.4,-0.384615384615385,-0.369230769230769,
-0.353846153846154,-0.338461538461538,-0.323076923076923,-0.307692307692308,
-0.292307692307692,-0.276923076923077,-0.261538461538462,-0.246153846153846,
-0.230769230769231,-0.215384615384615,-0.2,-0.184615384615385,-0.169230769230769,
-0.153846153846154,-0.138461538461538,-0.123076923076923,-0.107692307692308,
-0.0923076923076923,-0.0769230769230769,-0.0615384615384615,-0.0461538461538462,
-0.0307692307692308,-0.0153846153846154,0.),.UNSPECIFIED.)
CURVE()
GEOMETRIC_REPRESENTATION_ITEM()
RATIONAL_B_SPLINE_CURVE((1.,1.,1.,1.,1.,1.,1.,1.,1.,1.,1.,1.,1.,1.,1.,1.,
1.,1.,1.,1.,1.,1.,1.,1.,1.,1.,1.,1.,1.,1.,1.,1.,1.,1.,1.,1.,1.,1.,1.,1.,
1.,1.,1.,1.,1.,1.,1.,1.,1.,1.,1.,1.,1.,1.,1.,1.,1.,1.,1.,1.,1.,1.,1.,1.,
1.,1.,1.,1.,1.,1.))
REPRESENTATION_ITEM('')
);
#195=(
BOUNDED_CURVE()
B_SPLINE_CURVE(5,(#30503,#30504,#30505,#30506,#30507,#30508,#30509,#30510,
#30511,#30512,#30513,#30514,#30515,#30516,#30517,#30518,#30519,#30520,#30521,
#30522,#30523,#30524,#30525,#30526,#30527,#30528,#30529,#30530,#30531,#30532,
#30533,#30534,#30535,#30536,#30537,#30538,#30539,#30540,#30541,#30542,#30543,
#30544,#30545,#30546,#30547,#30548,#30549,#30550,#30551,#30552,#30553,#30554,
#30555,#30556,#30557,#30558,#30559,#30560,#30561,#30562,#30563,#30564,#30565,
#30566,#30567,#30568,#30569,#30570,#30571,#30572),.UNSPECIFIED.,.F.,.F.)
B_SPLINE_CURVE_WITH_KNOTS((6,1,1,1,1,1,1,1,1,1,1,1,1,1,1,1,1,1,1,1,1,1,
1,1,1,1,1,1,1,1,1,1,1,1,1,1,1,1,1,1,1,1,1,1,1,1,1,1,1,1,1,1,1,1,1,1,1,1,
1,1,1,1,1,1,1,6),(-1.,-0.984615384615383,-0.969230769230768,-0.953846153846152,
-0.938461538461537,-0.923076923076922,-0.907692307692306,-0.892307692307691,
-0.876923076923076,-0.86153846153846,-0.846153846153845,-0.83076923076923,
-0.815384615384614,-0.799999999999999,-0.784615384615384,-0.769230769230768,
-0.753846153846153,-0.738461538461538,-0.723076923076922,-0.707692307692307,
-0.692307692307692,-0.676923076923076,-0.661538461538461,-0.646153846153846,
-0.63076923076923,-0.615384615384615,-0.6,-0.584615384615384,-0.569230769230769,
-0.553846153846154,-0.538461538461538,-0.523076923076923,-0.507692307692308,
-0.492307692307692,-0.476923076923077,-0.461538461538462,-0.446153846153846,
-0.430769230769231,-0.415384615384615,-0.4,-0.384615384615385,-0.369230769230769,
-0.353846153846154,-0.338461538461538,-0.323076923076923,-0.307692307692308,
-0.292307692307692,-0.276923076923077,-0.261538461538462,-0.246153846153846,
-0.230769230769231,-0.215384615384615,-0.2,-0.184615384615385,-0.169230769230769,
-0.153846153846154,-0.138461538461538,-0.123076923076923,-0.107692307692308,
-0.0923076923076923,-0.0769230769230769,-0.0615384615384615,-0.0461538461538462,
-0.0307692307692308,-0.0153846153846154,0.),.UNSPECIFIED.)
CURVE()
GEOMETRIC_REPRESENTATION_ITEM()
RATIONAL_B_SPLINE_CURVE((1.,1.,1.,1.,1.,1.,1.,1.,1.,1.,1.,1.,1.,1.,1.,1.,
1.,1.,1.,1.,1.,1.,1.,1.,1.,1.,1.,1.,1.,1.,1.,1.,1.,1.,1.,1.,1.,1.,1.,1.,
1.,1.,1.,1.,1.,1.,1.,1.,1.,1.,1.,1.,1.,1.,1.,1.,1.,1.,1.,1.,1.,1.,1.,1.,
1.,1.,1.,1.,1.,1.))
REPRESENTATION_ITEM('')
);
#196=(
BOUNDED_CURVE()
B_SPLINE_CURVE(5,(#30719,#30720,#30721,#30722,#30723,#30724,#30725,#30726,
#30727,#30728,#30729,#30730,#30731,#30732,#30733,#30734,#30735,#30736,#30737,
#30738,#30739,#30740,#30741,#30742,#30743,#30744,#30745,#30746,#30747,#30748,
#30749,#30750,#30751,#30752,#30753,#30754,#30755,#30756,#30757,#30758,#30759,
#30760,#30761,#30762,#30763,#30764,#30765,#30766,#30767,#30768,#30769,#30770,
#30771,#30772,#30773,#30774,#30775,#30776,#30777,#30778,#30779,#30780,#30781,
#30782,#30783,#30784,#30785,#30786,#30787,#30788),.UNSPECIFIED.,.F.,.F.)
B_SPLINE_CURVE_WITH_KNOTS((6,1,1,1,1,1,1,1,1,1,1,1,1,1,1,1,1,1,1,1,1,1,
1,1,1,1,1,1,1,1,1,1,1,1,1,1,1,1,1,1,1,1,1,1,1,1,1,1,1,1,1,1,1,1,1,1,1,1,
1,1,1,1,1,1,1,6),(-1.,-0.984615384615383,-0.969230769230768,-0.953846153846152,
-0.938461538461537,-0.923076923076922,-0.907692307692306,-0.892307692307691,
-0.876923076923076,-0.86153846153846,-0.846153846153845,-0.83076923076923,
-0.815384615384614,-0.799999999999999,-0.784615384615384,-0.769230769230768,
-0.753846153846153,-0.738461538461538,-0.723076923076922,-0.707692307692307,
-0.692307692307692,-0.676923076923076,-0.661538461538461,-0.646153846153846,
-0.63076923076923,-0.615384615384615,-0.6,-0.584615384615384,-0.569230769230769,
-0.553846153846154,-0.538461538461538,-0.523076923076923,-0.507692307692308,
-0.492307692307692,-0.476923076923077,-0.461538461538462,-0.446153846153846,
-0.430769230769231,-0.415384615384615,-0.4,-0.384615384615385,-0.369230769230769,
-0.353846153846154,-0.338461538461538,-0.323076923076923,-0.307692307692308,
-0.292307692307692,-0.276923076923077,-0.261538461538462,-0.246153846153846,
-0.230769230769231,-0.215384615384615,-0.2,-0.184615384615385,-0.169230769230769,
-0.153846153846154,-0.138461538461538,-0.123076923076923,-0.107692307692308,
-0.0923076923076923,-0.0769230769230769,-0.0615384615384615,-0.0461538461538462,
-0.0307692307692308,-0.0153846153846154,0.),.UNSPECIFIED.)
CURVE()
GEOMETRIC_REPRESENTATION_ITEM()
RATIONAL_B_SPLINE_CURVE((1.,1.,1.,1.,1.,1.,1.,1.,1.,1.,1.,1.,1.,1.,1.,1.,
1.,1.,1.,1.,1.,1.,1.,1.,1.,1.,1.,1.,1.,1.,1.,1.,1.,1.,1.,1.,1.,1.,1.,1.,
1.,1.,1.,1.,1.,1.,1.,1.,1.,1.,1.,1.,1.,1.,1.,1.,1.,1.,1.,1.,1.,1.,1.,1.,
1.,1.,1.,1.,1.,1.))
REPRESENTATION_ITEM('')
);
#197=(
BOUNDED_CURVE()
B_SPLINE_CURVE(5,(#30935,#30936,#30937,#30938,#30939,#30940,#30941,#30942,
#30943,#30944,#30945,#30946,#30947,#30948,#30949,#30950,#30951,#30952,#30953,
#30954,#30955,#30956,#30957,#30958,#30959,#30960,#30961,#30962,#30963,#30964,
#30965,#30966,#30967,#30968,#30969,#30970,#30971,#30972,#30973,#30974,#30975,
#30976,#30977,#30978,#30979,#30980,#30981,#30982,#30983,#30984,#30985,#30986,
#30987,#30988,#30989,#30990,#30991,#30992,#30993,#30994,#30995,#30996,#30997,
#30998,#30999,#31000,#31001,#31002,#31003,#31004),.UNSPECIFIED.,.F.,.F.)
B_SPLINE_CURVE_WITH_KNOTS((6,1,1,1,1,1,1,1,1,1,1,1,1,1,1,1,1,1,1,1,1,1,
1,1,1,1,1,1,1,1,1,1,1,1,1,1,1,1,1,1,1,1,1,1,1,1,1,1,1,1,1,1,1,1,1,1,1,1,
1,1,1,1,1,1,1,6),(-1.,-0.984615384615383,-0.969230769230768,-0.953846153846152,
-0.938461538461537,-0.923076923076922,-0.907692307692306,-0.892307692307691,
-0.876923076923076,-0.86153846153846,-0.846153846153845,-0.83076923076923,
-0.815384615384614,-0.799999999999999,-0.784615384615384,-0.769230769230768,
-0.753846153846153,-0.738461538461538,-0.723076923076922,-0.707692307692307,
-0.692307692307692,-0.676923076923076,-0.661538461538461,-0.646153846153846,
-0.63076923076923,-0.615384615384615,-0.6,-0.584615384615384,-0.569230769230769,
-0.553846153846154,-0.538461538461538,-0.523076923076923,-0.507692307692308,
-0.492307692307692,-0.476923076923077,-0.461538461538462,-0.446153846153846,
-0.430769230769231,-0.415384615384615,-0.4,-0.384615384615385,-0.369230769230769,
-0.353846153846154,-0.338461538461538,-0.323076923076923,-0.307692307692308,
-0.292307692307692,-0.276923076923077,-0.261538461538462,-0.246153846153846,
-0.230769230769231,-0.215384615384615,-0.2,-0.184615384615385,-0.169230769230769,
-0.153846153846154,-0.138461538461538,-0.123076923076923,-0.107692307692308,
-0.0923076923076923,-0.0769230769230769,-0.0615384615384615,-0.0461538461538462,
-0.0307692307692308,-0.0153846153846154,0.),.UNSPECIFIED.)
CURVE()
GEOMETRIC_REPRESENTATION_ITEM()
RATIONAL_B_SPLINE_CURVE((1.,1.,1.,1.,1.,1.,1.,1.,1.,1.,1.,1.,1.,1.,1.,1.,
1.,1.,1.,1.,1.,1.,1.,1.,1.,1.,1.,1.,1.,1.,1.,1.,1.,1.,1.,1.,1.,1.,1.,1.,
1.,1.,1.,1.,1.,1.,1.,1.,1.,1.,1.,1.,1.,1.,1.,1.,1.,1.,1.,1.,1.,1.,1.,1.,
1.,1.,1.,1.,1.,1.))
REPRESENTATION_ITEM('')
);
#198=(
BOUNDED_CURVE()
B_SPLINE_CURVE(5,(#31151,#31152,#31153,#31154,#31155,#31156,#31157,#31158,
#31159,#31160,#31161,#31162,#31163,#31164,#31165,#31166,#31167,#31168,#31169,
#31170,#31171,#31172,#31173,#31174,#31175,#31176,#31177,#31178,#31179,#31180,
#31181,#31182,#31183,#31184,#31185,#31186,#31187,#31188,#31189,#31190,#31191,
#31192,#31193,#31194,#31195,#31196,#31197,#31198,#31199,#31200,#31201,#31202,
#31203,#31204,#31205,#31206,#31207,#31208,#31209,#31210,#31211,#31212,#31213,
#31214,#31215,#31216,#31217,#31218,#31219,#31220),.UNSPECIFIED.,.F.,.F.)
B_SPLINE_CURVE_WITH_KNOTS((6,1,1,1,1,1,1,1,1,1,1,1,1,1,1,1,1,1,1,1,1,1,
1,1,1,1,1,1,1,1,1,1,1,1,1,1,1,1,1,1,1,1,1,1,1,1,1,1,1,1,1,1,1,1,1,1,1,1,
1,1,1,1,1,1,1,6),(-1.,-0.984615384615383,-0.969230769230768,-0.953846153846152,
-0.938461538461537,-0.923076923076922,-0.907692307692306,-0.892307692307691,
-0.876923076923076,-0.86153846153846,-0.846153846153845,-0.83076923076923,
-0.815384615384614,-0.799999999999999,-0.784615384615384,-0.769230769230768,
-0.753846153846153,-0.738461538461538,-0.723076923076922,-0.707692307692307,
-0.692307692307692,-0.676923076923076,-0.661538461538461,-0.646153846153846,
-0.63076923076923,-0.615384615384615,-0.6,-0.584615384615384,-0.569230769230769,
-0.553846153846154,-0.538461538461538,-0.523076923076923,-0.507692307692308,
-0.492307692307692,-0.476923076923077,-0.461538461538462,-0.446153846153846,
-0.430769230769231,-0.415384615384615,-0.4,-0.384615384615385,-0.369230769230769,
-0.353846153846154,-0.338461538461538,-0.323076923076923,-0.307692307692308,
-0.292307692307692,-0.276923076923077,-0.261538461538462,-0.246153846153846,
-0.230769230769231,-0.215384615384615,-0.2,-0.184615384615385,-0.169230769230769,
-0.153846153846154,-0.138461538461538,-0.123076923076923,-0.107692307692308,
-0.0923076923076923,-0.0769230769230769,-0.0615384615384615,-0.0461538461538462,
-0.0307692307692308,-0.0153846153846154,0.),.UNSPECIFIED.)
CURVE()
GEOMETRIC_REPRESENTATION_ITEM()
RATIONAL_B_SPLINE_CURVE((1.,1.,1.,1.,1.,1.,1.,1.,1.,1.,1.,1.,1.,1.,1.,1.,
1.,1.,1.,1.,1.,1.,1.,1.,1.,1.,1.,1.,1.,1.,1.,1.,1.,1.,1.,1.,1.,1.,1.,1.,
1.,1.,1.,1.,1.,1.,1.,1.,1.,1.,1.,1.,1.,1.,1.,1.,1.,1.,1.,1.,1.,1.,1.,1.,
1.,1.,1.,1.,1.,1.))
REPRESENTATION_ITEM('')
);
#199=(
BOUNDED_CURVE()
B_SPLINE_CURVE(5,(#31367,#31368,#31369,#31370,#31371,#31372,#31373,#31374,
#31375,#31376,#31377,#31378,#31379,#31380,#31381,#31382,#31383,#31384,#31385,
#31386,#31387,#31388,#31389,#31390,#31391,#31392,#31393,#31394,#31395,#31396,
#31397,#31398,#31399,#31400,#31401,#31402,#31403,#31404,#31405,#31406,#31407,
#31408,#31409,#31410,#31411,#31412,#31413,#31414,#31415,#31416,#31417,#31418,
#31419,#31420,#31421,#31422,#31423,#31424,#31425,#31426,#31427,#31428,#31429,
#31430,#31431,#31432,#31433,#31434,#31435,#31436),.UNSPECIFIED.,.F.,.F.)
B_SPLINE_CURVE_WITH_KNOTS((6,1,1,1,1,1,1,1,1,1,1,1,1,1,1,1,1,1,1,1,1,1,
1,1,1,1,1,1,1,1,1,1,1,1,1,1,1,1,1,1,1,1,1,1,1,1,1,1,1,1,1,1,1,1,1,1,1,1,
1,1,1,1,1,1,1,6),(-1.,-0.984615384615383,-0.969230769230768,-0.953846153846152,
-0.938461538461537,-0.923076923076922,-0.907692307692306,-0.892307692307691,
-0.876923076923076,-0.86153846153846,-0.846153846153845,-0.83076923076923,
-0.815384615384614,-0.799999999999999,-0.784615384615384,-0.769230769230768,
-0.753846153846153,-0.738461538461538,-0.723076923076922,-0.707692307692307,
-0.692307692307692,-0.676923076923076,-0.661538461538461,-0.646153846153846,
-0.63076923076923,-0.615384615384615,-0.6,-0.584615384615384,-0.569230769230769,
-0.553846153846154,-0.538461538461538,-0.523076923076923,-0.507692307692308,
-0.492307692307692,-0.476923076923077,-0.461538461538462,-0.446153846153846,
-0.430769230769231,-0.415384615384615,-0.4,-0.384615384615385,-0.369230769230769,
-0.353846153846154,-0.338461538461538,-0.323076923076923,-0.307692307692308,
-0.292307692307692,-0.276923076923077,-0.261538461538462,-0.246153846153846,
-0.230769230769231,-0.215384615384615,-0.2,-0.184615384615385,-0.169230769230769,
-0.153846153846154,-0.138461538461538,-0.123076923076923,-0.107692307692308,
-0.0923076923076923,-0.0769230769230769,-0.0615384615384615,-0.0461538461538462,
-0.0307692307692308,-0.0153846153846154,0.),.UNSPECIFIED.)
CURVE()
GEOMETRIC_REPRESENTATION_ITEM()
RATIONAL_B_SPLINE_CURVE((1.,1.,1.,1.,1.,1.,1.,1.,1.,1.,1.,1.,1.,1.,1.,1.,
1.,1.,1.,1.,1.,1.,1.,1.,1.,1.,1.,1.,1.,1.,1.,1.,1.,1.,1.,1.,1.,1.,1.,1.,
1.,1.,1.,1.,1.,1.,1.,1.,1.,1.,1.,1.,1.,1.,1.,1.,1.,1.,1.,1.,1.,1.,1.,1.,
1.,1.,1.,1.,1.,1.))
REPRESENTATION_ITEM('')
);
#200=(
BOUNDED_CURVE()
B_SPLINE_CURVE(5,(#31583,#31584,#31585,#31586,#31587,#31588,#31589,#31590,
#31591,#31592,#31593,#31594,#31595,#31596,#31597,#31598,#31599,#31600,#31601,
#31602,#31603,#31604,#31605,#31606,#31607,#31608,#31609,#31610,#31611,#31612,
#31613,#31614,#31615,#31616,#31617,#31618,#31619,#31620,#31621,#31622,#31623,
#31624,#31625,#31626,#31627,#31628,#31629,#31630,#31631,#31632,#31633,#31634,
#31635,#31636,#31637,#31638,#31639,#31640,#31641,#31642,#31643,#31644,#31645,
#31646,#31647,#31648,#31649,#31650,#31651,#31652),.UNSPECIFIED.,.F.,.F.)
B_SPLINE_CURVE_WITH_KNOTS((6,1,1,1,1,1,1,1,1,1,1,1,1,1,1,1,1,1,1,1,1,1,
1,1,1,1,1,1,1,1,1,1,1,1,1,1,1,1,1,1,1,1,1,1,1,1,1,1,1,1,1,1,1,1,1,1,1,1,
1,1,1,1,1,1,1,6),(-1.,-0.984615384615383,-0.969230769230768,-0.953846153846152,
-0.938461538461537,-0.923076923076922,-0.907692307692306,-0.892307692307691,
-0.876923076923076,-0.86153846153846,-0.846153846153845,-0.83076923076923,
-0.815384615384614,-0.799999999999999,-0.784615384615384,-0.769230769230768,
-0.753846153846153,-0.738461538461538,-0.723076923076922,-0.707692307692307,
-0.692307692307692,-0.676923076923076,-0.661538461538461,-0.646153846153846,
-0.63076923076923,-0.615384615384615,-0.6,-0.584615384615384,-0.569230769230769,
-0.553846153846154,-0.538461538461538,-0.523076923076923,-0.507692307692308,
-0.492307692307692,-0.476923076923077,-0.461538461538462,-0.446153846153846,
-0.430769230769231,-0.415384615384615,-0.4,-0.384615384615385,-0.369230769230769,
-0.353846153846154,-0.338461538461538,-0.323076923076923,-0.307692307692308,
-0.292307692307692,-0.276923076923077,-0.261538461538462,-0.246153846153846,
-0.230769230769231,-0.215384615384615,-0.2,-0.184615384615385,-0.169230769230769,
-0.153846153846154,-0.138461538461538,-0.123076923076923,-0.107692307692308,
-0.0923076923076923,-0.0769230769230769,-0.0615384615384615,-0.0461538461538462,
-0.0307692307692308,-0.0153846153846154,0.),.UNSPECIFIED.)
CURVE()
GEOMETRIC_REPRESENTATION_ITEM()
RATIONAL_B_SPLINE_CURVE((1.,1.,1.,1.,1.,1.,1.,1.,1.,1.,1.,1.,1.,1.,1.,1.,
1.,1.,1.,1.,1.,1.,1.,1.,1.,1.,1.,1.,1.,1.,1.,1.,1.,1.,1.,1.,1.,1.,1.,1.,
1.,1.,1.,1.,1.,1.,1.,1.,1.,1.,1.,1.,1.,1.,1.,1.,1.,1.,1.,1.,1.,1.,1.,1.,
1.,1.,1.,1.,1.,1.))
REPRESENTATION_ITEM('')
);
#201=(
BOUNDED_CURVE()
B_SPLINE_CURVE(5,(#31799,#31800,#31801,#31802,#31803,#31804,#31805,#31806,
#31807,#31808,#31809,#31810,#31811,#31812,#31813,#31814,#31815,#31816,#31817,
#31818,#31819,#31820,#31821,#31822,#31823,#31824,#31825,#31826,#31827,#31828,
#31829,#31830,#31831,#31832,#31833,#31834,#31835,#31836,#31837,#31838,#31839,
#31840,#31841,#31842,#31843,#31844,#31845,#31846,#31847,#31848,#31849,#31850,
#31851,#31852,#31853,#31854,#31855,#31856,#31857,#31858,#31859,#31860,#31861,
#31862,#31863,#31864,#31865,#31866,#31867,#31868),.UNSPECIFIED.,.F.,.F.)
B_SPLINE_CURVE_WITH_KNOTS((6,1,1,1,1,1,1,1,1,1,1,1,1,1,1,1,1,1,1,1,1,1,
1,1,1,1,1,1,1,1,1,1,1,1,1,1,1,1,1,1,1,1,1,1,1,1,1,1,1,1,1,1,1,1,1,1,1,1,
1,1,1,1,1,1,1,6),(-1.,-0.984615384615383,-0.969230769230768,-0.953846153846152,
-0.938461538461537,-0.923076923076922,-0.907692307692306,-0.892307692307691,
-0.876923076923076,-0.86153846153846,-0.846153846153845,-0.83076923076923,
-0.815384615384614,-0.799999999999999,-0.784615384615384,-0.769230769230768,
-0.753846153846153,-0.738461538461538,-0.723076923076922,-0.707692307692307,
-0.692307692307692,-0.676923076923076,-0.661538461538461,-0.646153846153846,
-0.63076923076923,-0.615384615384615,-0.6,-0.584615384615384,-0.569230769230769,
-0.553846153846154,-0.538461538461538,-0.523076923076923,-0.507692307692308,
-0.492307692307692,-0.476923076923077,-0.461538461538462,-0.446153846153846,
-0.430769230769231,-0.415384615384615,-0.4,-0.384615384615385,-0.369230769230769,
-0.353846153846154,-0.338461538461538,-0.323076923076923,-0.307692307692308,
-0.292307692307692,-0.276923076923077,-0.261538461538462,-0.246153846153846,
-0.230769230769231,-0.215384615384615,-0.2,-0.184615384615385,-0.169230769230769,
-0.153846153846154,-0.138461538461538,-0.123076923076923,-0.107692307692308,
-0.0923076923076923,-0.0769230769230769,-0.0615384615384615,-0.0461538461538462,
-0.0307692307692308,-0.0153846153846154,0.),.UNSPECIFIED.)
CURVE()
GEOMETRIC_REPRESENTATION_ITEM()
RATIONAL_B_SPLINE_CURVE((1.,1.,1.,1.,1.,1.,1.,1.,1.,1.,1.,1.,1.,1.,1.,1.,
1.,1.,1.,1.,1.,1.,1.,1.,1.,1.,1.,1.,1.,1.,1.,1.,1.,1.,1.,1.,1.,1.,1.,1.,
1.,1.,1.,1.,1.,1.,1.,1.,1.,1.,1.,1.,1.,1.,1.,1.,1.,1.,1.,1.,1.,1.,1.,1.,
1.,1.,1.,1.,1.,1.))
REPRESENTATION_ITEM('')
);
#202=(
BOUNDED_CURVE()
B_SPLINE_CURVE(5,(#32015,#32016,#32017,#32018,#32019,#32020,#32021,#32022,
#32023,#32024,#32025,#32026,#32027,#32028,#32029,#32030,#32031,#32032,#32033,
#32034,#32035,#32036,#32037,#32038,#32039,#32040,#32041,#32042,#32043,#32044,
#32045,#32046,#32047,#32048,#32049,#32050,#32051,#32052,#32053,#32054,#32055,
#32056,#32057,#32058,#32059,#32060,#32061,#32062,#32063,#32064,#32065,#32066,
#32067,#32068,#32069,#32070,#32071,#32072,#32073,#32074,#32075,#32076,#32077,
#32078,#32079,#32080,#32081,#32082,#32083,#32084),.UNSPECIFIED.,.F.,.F.)
B_SPLINE_CURVE_WITH_KNOTS((6,1,1,1,1,1,1,1,1,1,1,1,1,1,1,1,1,1,1,1,1,1,
1,1,1,1,1,1,1,1,1,1,1,1,1,1,1,1,1,1,1,1,1,1,1,1,1,1,1,1,1,1,1,1,1,1,1,1,
1,1,1,1,1,1,1,6),(-1.,-0.984615384615383,-0.969230769230768,-0.953846153846152,
-0.938461538461537,-0.923076923076922,-0.907692307692306,-0.892307692307691,
-0.876923076923076,-0.86153846153846,-0.846153846153845,-0.83076923076923,
-0.815384615384614,-0.799999999999999,-0.784615384615384,-0.769230769230768,
-0.753846153846153,-0.738461538461538,-0.723076923076922,-0.707692307692307,
-0.692307692307692,-0.676923076923076,-0.661538461538461,-0.646153846153846,
-0.63076923076923,-0.615384615384615,-0.6,-0.584615384615384,-0.569230769230769,
-0.553846153846154,-0.538461538461538,-0.523076923076923,-0.507692307692308,
-0.492307692307692,-0.476923076923077,-0.461538461538462,-0.446153846153846,
-0.430769230769231,-0.415384615384615,-0.4,-0.384615384615385,-0.369230769230769,
-0.353846153846154,-0.338461538461538,-0.323076923076923,-0.307692307692308,
-0.292307692307692,-0.276923076923077,-0.261538461538462,-0.246153846153846,
-0.230769230769231,-0.215384615384615,-0.2,-0.184615384615385,-0.169230769230769,
-0.153846153846154,-0.138461538461538,-0.123076923076923,-0.107692307692308,
-0.0923076923076923,-0.0769230769230769,-0.0615384615384615,-0.0461538461538462,
-0.0307692307692308,-0.0153846153846154,0.),.UNSPECIFIED.)
CURVE()
GEOMETRIC_REPRESENTATION_ITEM()
RATIONAL_B_SPLINE_CURVE((1.,1.,1.,1.,1.,1.,1.,1.,1.,1.,1.,1.,1.,1.,1.,1.,
1.,1.,1.,1.,1.,1.,1.,1.,1.,1.,1.,1.,1.,1.,1.,1.,1.,1.,1.,1.,1.,1.,1.,1.,
1.,1.,1.,1.,1.,1.,1.,1.,1.,1.,1.,1.,1.,1.,1.,1.,1.,1.,1.,1.,1.,1.,1.,1.,
1.,1.,1.,1.,1.,1.))
REPRESENTATION_ITEM('')
);
#203=(
BOUNDED_CURVE()
B_SPLINE_CURVE(5,(#32231,#32232,#32233,#32234,#32235,#32236,#32237,#32238,
#32239,#32240,#32241,#32242,#32243,#32244,#32245,#32246,#32247,#32248,#32249,
#32250,#32251,#32252,#32253,#32254,#32255,#32256,#32257,#32258,#32259,#32260,
#32261,#32262,#32263,#32264,#32265,#32266,#32267,#32268,#32269,#32270,#32271,
#32272,#32273,#32274,#32275,#32276,#32277,#32278,#32279,#32280,#32281,#32282,
#32283,#32284,#32285,#32286,#32287,#32288,#32289,#32290,#32291,#32292,#32293,
#32294,#32295,#32296,#32297,#32298,#32299,#32300),.UNSPECIFIED.,.F.,.F.)
B_SPLINE_CURVE_WITH_KNOTS((6,1,1,1,1,1,1,1,1,1,1,1,1,1,1,1,1,1,1,1,1,1,
1,1,1,1,1,1,1,1,1,1,1,1,1,1,1,1,1,1,1,1,1,1,1,1,1,1,1,1,1,1,1,1,1,1,1,1,
1,1,1,1,1,1,1,6),(-1.,-0.984615384615383,-0.969230769230768,-0.953846153846152,
-0.938461538461537,-0.923076923076922,-0.907692307692306,-0.892307692307691,
-0.876923076923076,-0.86153846153846,-0.846153846153845,-0.83076923076923,
-0.815384615384614,-0.799999999999999,-0.784615384615384,-0.769230769230768,
-0.753846153846153,-0.738461538461538,-0.723076923076922,-0.707692307692307,
-0.692307692307692,-0.676923076923076,-0.661538461538461,-0.646153846153846,
-0.63076923076923,-0.615384615384615,-0.6,-0.584615384615384,-0.569230769230769,
-0.553846153846154,-0.538461538461538,-0.523076923076923,-0.507692307692308,
-0.492307692307692,-0.476923076923077,-0.461538461538462,-0.446153846153846,
-0.430769230769231,-0.415384615384615,-0.4,-0.384615384615385,-0.369230769230769,
-0.353846153846154,-0.338461538461538,-0.323076923076923,-0.307692307692308,
-0.292307692307692,-0.276923076923077,-0.261538461538462,-0.246153846153846,
-0.230769230769231,-0.215384615384615,-0.2,-0.184615384615385,-0.169230769230769,
-0.153846153846154,-0.138461538461538,-0.123076923076923,-0.107692307692308,
-0.0923076923076923,-0.0769230769230769,-0.0615384615384615,-0.0461538461538462,
-0.0307692307692308,-0.0153846153846154,0.),.UNSPECIFIED.)
CURVE()
GEOMETRIC_REPRESENTATION_ITEM()
RATIONAL_B_SPLINE_CURVE((1.,1.,1.,1.,1.,1.,1.,1.,1.,1.,1.,1.,1.,1.,1.,1.,
1.,1.,1.,1.,1.,1.,1.,1.,1.,1.,1.,1.,1.,1.,1.,1.,1.,1.,1.,1.,1.,1.,1.,1.,
1.,1.,1.,1.,1.,1.,1.,1.,1.,1.,1.,1.,1.,1.,1.,1.,1.,1.,1.,1.,1.,1.,1.,1.,
1.,1.,1.,1.,1.,1.))
REPRESENTATION_ITEM('')
);
#204=(
BOUNDED_CURVE()
B_SPLINE_CURVE(5,(#32447,#32448,#32449,#32450,#32451,#32452,#32453,#32454,
#32455,#32456,#32457,#32458,#32459,#32460,#32461,#32462,#32463,#32464,#32465,
#32466,#32467,#32468,#32469,#32470,#32471,#32472,#32473,#32474,#32475,#32476,
#32477,#32478,#32479,#32480,#32481,#32482,#32483,#32484,#32485,#32486,#32487,
#32488,#32489,#32490,#32491,#32492,#32493,#32494,#32495,#32496,#32497,#32498,
#32499,#32500,#32501,#32502,#32503,#32504,#32505,#32506,#32507,#32508,#32509,
#32510,#32511,#32512,#32513,#32514,#32515,#32516),.UNSPECIFIED.,.F.,.F.)
B_SPLINE_CURVE_WITH_KNOTS((6,1,1,1,1,1,1,1,1,1,1,1,1,1,1,1,1,1,1,1,1,1,
1,1,1,1,1,1,1,1,1,1,1,1,1,1,1,1,1,1,1,1,1,1,1,1,1,1,1,1,1,1,1,1,1,1,1,1,
1,1,1,1,1,1,1,6),(-1.,-0.984615384615383,-0.969230769230768,-0.953846153846152,
-0.938461538461537,-0.923076923076922,-0.907692307692306,-0.892307692307691,
-0.876923076923076,-0.86153846153846,-0.846153846153845,-0.83076923076923,
-0.815384615384614,-0.799999999999999,-0.784615384615384,-0.769230769230768,
-0.753846153846153,-0.738461538461538,-0.723076923076922,-0.707692307692307,
-0.692307692307692,-0.676923076923076,-0.661538461538461,-0.646153846153846,
-0.63076923076923,-0.615384615384615,-0.6,-0.584615384615384,-0.569230769230769,
-0.553846153846154,-0.538461538461538,-0.523076923076923,-0.507692307692308,
-0.492307692307692,-0.476923076923077,-0.461538461538462,-0.446153846153846,
-0.430769230769231,-0.415384615384615,-0.4,-0.384615384615385,-0.369230769230769,
-0.353846153846154,-0.338461538461538,-0.323076923076923,-0.307692307692308,
-0.292307692307692,-0.276923076923077,-0.261538461538462,-0.246153846153846,
-0.230769230769231,-0.215384615384615,-0.2,-0.184615384615385,-0.169230769230769,
-0.153846153846154,-0.138461538461538,-0.123076923076923,-0.107692307692308,
-0.0923076923076923,-0.0769230769230769,-0.0615384615384615,-0.0461538461538462,
-0.0307692307692308,-0.0153846153846154,0.),.UNSPECIFIED.)
CURVE()
GEOMETRIC_REPRESENTATION_ITEM()
RATIONAL_B_SPLINE_CURVE((1.,1.,1.,1.,1.,1.,1.,1.,1.,1.,1.,1.,1.,1.,1.,1.,
1.,1.,1.,1.,1.,1.,1.,1.,1.,1.,1.,1.,1.,1.,1.,1.,1.,1.,1.,1.,1.,1.,1.,1.,
1.,1.,1.,1.,1.,1.,1.,1.,1.,1.,1.,1.,1.,1.,1.,1.,1.,1.,1.,1.,1.,1.,1.,1.,
1.,1.,1.,1.,1.,1.))
REPRESENTATION_ITEM('')
);
#205=(
BOUNDED_CURVE()
B_SPLINE_CURVE(5,(#32663,#32664,#32665,#32666,#32667,#32668,#32669,#32670,
#32671,#32672,#32673,#32674,#32675,#32676,#32677,#32678,#32679,#32680,#32681,
#32682,#32683,#32684,#32685,#32686,#32687,#32688,#32689,#32690,#32691,#32692,
#32693,#32694,#32695,#32696,#32697,#32698,#32699,#32700,#32701,#32702,#32703,
#32704,#32705,#32706,#32707,#32708,#32709,#32710,#32711,#32712,#32713,#32714,
#32715,#32716,#32717,#32718,#32719,#32720,#32721,#32722,#32723,#32724,#32725,
#32726,#32727,#32728,#32729,#32730,#32731,#32732),.UNSPECIFIED.,.F.,.F.)
B_SPLINE_CURVE_WITH_KNOTS((6,1,1,1,1,1,1,1,1,1,1,1,1,1,1,1,1,1,1,1,1,1,
1,1,1,1,1,1,1,1,1,1,1,1,1,1,1,1,1,1,1,1,1,1,1,1,1,1,1,1,1,1,1,1,1,1,1,1,
1,1,1,1,1,1,1,6),(-1.,-0.984615384615383,-0.969230769230768,-0.953846153846152,
-0.938461538461537,-0.923076923076922,-0.907692307692306,-0.892307692307691,
-0.876923076923076,-0.86153846153846,-0.846153846153845,-0.83076923076923,
-0.815384615384614,-0.799999999999999,-0.784615384615384,-0.769230769230768,
-0.753846153846153,-0.738461538461538,-0.723076923076922,-0.707692307692307,
-0.692307692307692,-0.676923076923076,-0.661538461538461,-0.646153846153846,
-0.63076923076923,-0.615384615384615,-0.6,-0.584615384615384,-0.569230769230769,
-0.553846153846154,-0.538461538461538,-0.523076923076923,-0.507692307692308,
-0.492307692307692,-0.476923076923077,-0.461538461538462,-0.446153846153846,
-0.430769230769231,-0.415384615384615,-0.4,-0.384615384615385,-0.369230769230769,
-0.353846153846154,-0.338461538461538,-0.323076923076923,-0.307692307692308,
-0.292307692307692,-0.276923076923077,-0.261538461538462,-0.246153846153846,
-0.230769230769231,-0.215384615384615,-0.2,-0.184615384615385,-0.169230769230769,
-0.153846153846154,-0.138461538461538,-0.123076923076923,-0.107692307692308,
-0.0923076923076923,-0.0769230769230769,-0.0615384615384615,-0.0461538461538462,
-0.0307692307692308,-0.0153846153846154,0.),.UNSPECIFIED.)
CURVE()
GEOMETRIC_REPRESENTATION_ITEM()
RATIONAL_B_SPLINE_CURVE((1.,1.,1.,1.,1.,1.,1.,1.,1.,1.,1.,1.,1.,1.,1.,1.,
1.,1.,1.,1.,1.,1.,1.,1.,1.,1.,1.,1.,1.,1.,1.,1.,1.,1.,1.,1.,1.,1.,1.,1.,
1.,1.,1.,1.,1.,1.,1.,1.,1.,1.,1.,1.,1.,1.,1.,1.,1.,1.,1.,1.,1.,1.,1.,1.,
1.,1.,1.,1.,1.,1.))
REPRESENTATION_ITEM('')
);
#206=(
BOUNDED_CURVE()
B_SPLINE_CURVE(5,(#32879,#32880,#32881,#32882,#32883,#32884,#32885,#32886,
#32887,#32888,#32889,#32890,#32891,#32892,#32893,#32894,#32895,#32896,#32897,
#32898,#32899,#32900,#32901,#32902,#32903,#32904,#32905,#32906,#32907,#32908,
#32909,#32910,#32911,#32912,#32913,#32914,#32915,#32916,#32917,#32918,#32919,
#32920,#32921,#32922,#32923,#32924,#32925,#32926,#32927,#32928,#32929,#32930,
#32931,#32932,#32933,#32934,#32935,#32936,#32937,#32938,#32939,#32940,#32941,
#32942,#32943,#32944,#32945,#32946,#32947,#32948),.UNSPECIFIED.,.F.,.F.)
B_SPLINE_CURVE_WITH_KNOTS((6,1,1,1,1,1,1,1,1,1,1,1,1,1,1,1,1,1,1,1,1,1,
1,1,1,1,1,1,1,1,1,1,1,1,1,1,1,1,1,1,1,1,1,1,1,1,1,1,1,1,1,1,1,1,1,1,1,1,
1,1,1,1,1,1,1,6),(-1.,-0.984615384615383,-0.969230769230768,-0.953846153846152,
-0.938461538461537,-0.923076923076922,-0.907692307692306,-0.892307692307691,
-0.876923076923076,-0.86153846153846,-0.846153846153845,-0.83076923076923,
-0.815384615384614,-0.799999999999999,-0.784615384615384,-0.769230769230768,
-0.753846153846153,-0.738461538461538,-0.723076923076922,-0.707692307692307,
-0.692307692307692,-0.676923076923076,-0.661538461538461,-0.646153846153846,
-0.63076923076923,-0.615384615384615,-0.6,-0.584615384615384,-0.569230769230769,
-0.553846153846154,-0.538461538461538,-0.523076923076923,-0.507692307692308,
-0.492307692307692,-0.476923076923077,-0.461538461538462,-0.446153846153846,
-0.430769230769231,-0.415384615384615,-0.4,-0.384615384615385,-0.369230769230769,
-0.353846153846154,-0.338461538461538,-0.323076923076923,-0.307692307692308,
-0.292307692307692,-0.276923076923077,-0.261538461538462,-0.246153846153846,
-0.230769230769231,-0.215384615384615,-0.2,-0.184615384615385,-0.169230769230769,
-0.153846153846154,-0.138461538461538,-0.123076923076923,-0.107692307692308,
-0.0923076923076923,-0.0769230769230769,-0.0615384615384615,-0.0461538461538462,
-0.0307692307692308,-0.0153846153846154,0.),.UNSPECIFIED.)
CURVE()
GEOMETRIC_REPRESENTATION_ITEM()
RATIONAL_B_SPLINE_CURVE((1.,1.,1.,1.,1.,1.,1.,1.,1.,1.,1.,1.,1.,1.,1.,1.,
1.,1.,1.,1.,1.,1.,1.,1.,1.,1.,1.,1.,1.,1.,1.,1.,1.,1.,1.,1.,1.,1.,1.,1.,
1.,1.,1.,1.,1.,1.,1.,1.,1.,1.,1.,1.,1.,1.,1.,1.,1.,1.,1.,1.,1.,1.,1.,1.,
1.,1.,1.,1.,1.,1.))
REPRESENTATION_ITEM('')
);
#207=(
BOUNDED_CURVE()
B_SPLINE_CURVE(5,(#33095,#33096,#33097,#33098,#33099,#33100,#33101,#33102,
#33103,#33104,#33105,#33106,#33107,#33108,#33109,#33110,#33111,#33112,#33113,
#33114,#33115,#33116,#33117,#33118,#33119,#33120,#33121,#33122,#33123,#33124,
#33125,#33126,#33127,#33128,#33129,#33130,#33131,#33132,#33133,#33134,#33135,
#33136,#33137,#33138,#33139,#33140,#33141,#33142,#33143,#33144,#33145,#33146,
#33147,#33148,#33149,#33150,#33151,#33152,#33153,#33154,#33155,#33156,#33157,
#33158,#33159,#33160,#33161,#33162,#33163,#33164),.UNSPECIFIED.,.F.,.F.)
B_SPLINE_CURVE_WITH_KNOTS((6,1,1,1,1,1,1,1,1,1,1,1,1,1,1,1,1,1,1,1,1,1,
1,1,1,1,1,1,1,1,1,1,1,1,1,1,1,1,1,1,1,1,1,1,1,1,1,1,1,1,1,1,1,1,1,1,1,1,
1,1,1,1,1,1,1,6),(-1.,-0.984615384615383,-0.969230769230768,-0.953846153846152,
-0.938461538461537,-0.923076923076922,-0.907692307692306,-0.892307692307691,
-0.876923076923076,-0.86153846153846,-0.846153846153845,-0.83076923076923,
-0.815384615384614,-0.799999999999999,-0.784615384615384,-0.769230769230768,
-0.753846153846153,-0.738461538461538,-0.723076923076922,-0.707692307692307,
-0.692307692307692,-0.676923076923076,-0.661538461538461,-0.646153846153846,
-0.63076923076923,-0.615384615384615,-0.6,-0.584615384615384,-0.569230769230769,
-0.553846153846154,-0.538461538461538,-0.523076923076923,-0.507692307692308,
-0.492307692307692,-0.476923076923077,-0.461538461538462,-0.446153846153846,
-0.430769230769231,-0.415384615384615,-0.4,-0.384615384615385,-0.369230769230769,
-0.353846153846154,-0.338461538461538,-0.323076923076923,-0.307692307692308,
-0.292307692307692,-0.276923076923077,-0.261538461538462,-0.246153846153846,
-0.230769230769231,-0.215384615384615,-0.2,-0.184615384615385,-0.169230769230769,
-0.153846153846154,-0.138461538461538,-0.123076923076923,-0.107692307692308,
-0.0923076923076923,-0.0769230769230769,-0.0615384615384615,-0.0461538461538462,
-0.0307692307692308,-0.0153846153846154,0.),.UNSPECIFIED.)
CURVE()
GEOMETRIC_REPRESENTATION_ITEM()
RATIONAL_B_SPLINE_CURVE((1.,1.,1.,1.,1.,1.,1.,1.,1.,1.,1.,1.,1.,1.,1.,1.,
1.,1.,1.,1.,1.,1.,1.,1.,1.,1.,1.,1.,1.,1.,1.,1.,1.,1.,1.,1.,1.,1.,1.,1.,
1.,1.,1.,1.,1.,1.,1.,1.,1.,1.,1.,1.,1.,1.,1.,1.,1.,1.,1.,1.,1.,1.,1.,1.,
1.,1.,1.,1.,1.,1.))
REPRESENTATION_ITEM('')
);
#208=(
BOUNDED_CURVE()
B_SPLINE_CURVE(5,(#33311,#33312,#33313,#33314,#33315,#33316,#33317,#33318,
#33319,#33320,#33321,#33322,#33323,#33324,#33325,#33326,#33327,#33328,#33329,
#33330,#33331,#33332,#33333,#33334,#33335,#33336,#33337,#33338,#33339,#33340,
#33341,#33342,#33343,#33344,#33345,#33346,#33347,#33348,#33349,#33350,#33351,
#33352,#33353,#33354,#33355,#33356,#33357,#33358,#33359,#33360,#33361,#33362,
#33363,#33364,#33365,#33366,#33367,#33368,#33369,#33370,#33371,#33372,#33373,
#33374,#33375,#33376,#33377,#33378,#33379,#33380),.UNSPECIFIED.,.F.,.F.)
B_SPLINE_CURVE_WITH_KNOTS((6,1,1,1,1,1,1,1,1,1,1,1,1,1,1,1,1,1,1,1,1,1,
1,1,1,1,1,1,1,1,1,1,1,1,1,1,1,1,1,1,1,1,1,1,1,1,1,1,1,1,1,1,1,1,1,1,1,1,
1,1,1,1,1,1,1,6),(-1.,-0.984615384615383,-0.969230769230768,-0.953846153846152,
-0.938461538461537,-0.923076923076922,-0.907692307692306,-0.892307692307691,
-0.876923076923076,-0.86153846153846,-0.846153846153845,-0.83076923076923,
-0.815384615384614,-0.799999999999999,-0.784615384615384,-0.769230769230768,
-0.753846153846153,-0.738461538461538,-0.723076923076922,-0.707692307692307,
-0.692307692307692,-0.676923076923076,-0.661538461538461,-0.646153846153846,
-0.63076923076923,-0.615384615384615,-0.6,-0.584615384615384,-0.569230769230769,
-0.553846153846154,-0.538461538461538,-0.523076923076923,-0.507692307692308,
-0.492307692307692,-0.476923076923077,-0.461538461538462,-0.446153846153846,
-0.430769230769231,-0.415384615384615,-0.4,-0.384615384615385,-0.369230769230769,
-0.353846153846154,-0.338461538461538,-0.323076923076923,-0.307692307692308,
-0.292307692307692,-0.276923076923077,-0.261538461538462,-0.246153846153846,
-0.230769230769231,-0.215384615384615,-0.2,-0.184615384615385,-0.169230769230769,
-0.153846153846154,-0.138461538461538,-0.123076923076923,-0.107692307692308,
-0.0923076923076923,-0.0769230769230769,-0.0615384615384615,-0.0461538461538462,
-0.0307692307692308,-0.0153846153846154,0.),.UNSPECIFIED.)
CURVE()
GEOMETRIC_REPRESENTATION_ITEM()
RATIONAL_B_SPLINE_CURVE((1.,1.,1.,1.,1.,1.,1.,1.,1.,1.,1.,1.,1.,1.,1.,1.,
1.,1.,1.,1.,1.,1.,1.,1.,1.,1.,1.,1.,1.,1.,1.,1.,1.,1.,1.,1.,1.,1.,1.,1.,
1.,1.,1.,1.,1.,1.,1.,1.,1.,1.,1.,1.,1.,1.,1.,1.,1.,1.,1.,1.,1.,1.,1.,1.,
1.,1.,1.,1.,1.,1.))
REPRESENTATION_ITEM('')
);
#209=(
BOUNDED_CURVE()
B_SPLINE_CURVE(5,(#33527,#33528,#33529,#33530,#33531,#33532,#33533,#33534,
#33535,#33536,#33537,#33538,#33539,#33540,#33541,#33542,#33543,#33544,#33545,
#33546,#33547,#33548,#33549,#33550,#33551,#33552,#33553,#33554,#33555,#33556,
#33557,#33558,#33559,#33560,#33561,#33562,#33563,#33564,#33565,#33566,#33567,
#33568,#33569,#33570,#33571,#33572,#33573,#33574,#33575,#33576,#33577,#33578,
#33579,#33580,#33581,#33582,#33583,#33584,#33585,#33586,#33587,#33588,#33589,
#33590,#33591,#33592,#33593,#33594,#33595,#33596),.UNSPECIFIED.,.F.,.F.)
B_SPLINE_CURVE_WITH_KNOTS((6,1,1,1,1,1,1,1,1,1,1,1,1,1,1,1,1,1,1,1,1,1,
1,1,1,1,1,1,1,1,1,1,1,1,1,1,1,1,1,1,1,1,1,1,1,1,1,1,1,1,1,1,1,1,1,1,1,1,
1,1,1,1,1,1,1,6),(-1.,-0.984615384615383,-0.969230769230768,-0.953846153846152,
-0.938461538461537,-0.923076923076922,-0.907692307692306,-0.892307692307691,
-0.876923076923076,-0.86153846153846,-0.846153846153845,-0.83076923076923,
-0.815384615384614,-0.799999999999999,-0.784615384615384,-0.769230769230768,
-0.753846153846153,-0.738461538461538,-0.723076923076922,-0.707692307692307,
-0.692307692307692,-0.676923076923076,-0.661538461538461,-0.646153846153846,
-0.63076923076923,-0.615384615384615,-0.6,-0.584615384615384,-0.569230769230769,
-0.553846153846154,-0.538461538461538,-0.523076923076923,-0.507692307692308,
-0.492307692307692,-0.476923076923077,-0.461538461538462,-0.446153846153846,
-0.430769230769231,-0.415384615384615,-0.4,-0.384615384615385,-0.369230769230769,
-0.353846153846154,-0.338461538461538,-0.323076923076923,-0.307692307692308,
-0.292307692307692,-0.276923076923077,-0.261538461538462,-0.246153846153846,
-0.230769230769231,-0.215384615384615,-0.2,-0.184615384615385,-0.169230769230769,
-0.153846153846154,-0.138461538461538,-0.123076923076923,-0.107692307692308,
-0.0923076923076923,-0.0769230769230769,-0.0615384615384615,-0.0461538461538462,
-0.0307692307692308,-0.0153846153846154,0.),.UNSPECIFIED.)
CURVE()
GEOMETRIC_REPRESENTATION_ITEM()
RATIONAL_B_SPLINE_CURVE((1.,1.,1.,1.,1.,1.,1.,1.,1.,1.,1.,1.,1.,1.,1.,1.,
1.,1.,1.,1.,1.,1.,1.,1.,1.,1.,1.,1.,1.,1.,1.,1.,1.,1.,1.,1.,1.,1.,1.,1.,
1.,1.,1.,1.,1.,1.,1.,1.,1.,1.,1.,1.,1.,1.,1.,1.,1.,1.,1.,1.,1.,1.,1.,1.,
1.,1.,1.,1.,1.,1.))
REPRESENTATION_ITEM('')
);
#210=(
BOUNDED_CURVE()
B_SPLINE_CURVE(5,(#33743,#33744,#33745,#33746,#33747,#33748,#33749,#33750,
#33751,#33752,#33753,#33754,#33755,#33756,#33757,#33758,#33759,#33760,#33761,
#33762,#33763,#33764,#33765,#33766,#33767,#33768,#33769,#33770,#33771,#33772,
#33773,#33774,#33775,#33776,#33777,#33778,#33779,#33780,#33781,#33782,#33783,
#33784,#33785,#33786,#33787,#33788,#33789,#33790,#33791,#33792,#33793,#33794,
#33795,#33796,#33797,#33798,#33799,#33800,#33801,#33802,#33803,#33804,#33805,
#33806,#33807,#33808,#33809,#33810,#33811,#33812),.UNSPECIFIED.,.F.,.F.)
B_SPLINE_CURVE_WITH_KNOTS((6,1,1,1,1,1,1,1,1,1,1,1,1,1,1,1,1,1,1,1,1,1,
1,1,1,1,1,1,1,1,1,1,1,1,1,1,1,1,1,1,1,1,1,1,1,1,1,1,1,1,1,1,1,1,1,1,1,1,
1,1,1,1,1,1,1,6),(-1.,-0.984615384615383,-0.969230769230768,-0.953846153846152,
-0.938461538461537,-0.923076923076922,-0.907692307692306,-0.892307692307691,
-0.876923076923076,-0.86153846153846,-0.846153846153845,-0.83076923076923,
-0.815384615384614,-0.799999999999999,-0.784615384615384,-0.769230769230768,
-0.753846153846153,-0.738461538461538,-0.723076923076922,-0.707692307692307,
-0.692307692307692,-0.676923076923076,-0.661538461538461,-0.646153846153846,
-0.63076923076923,-0.615384615384615,-0.6,-0.584615384615384,-0.569230769230769,
-0.553846153846154,-0.538461538461538,-0.523076923076923,-0.507692307692308,
-0.492307692307692,-0.476923076923077,-0.461538461538462,-0.446153846153846,
-0.430769230769231,-0.415384615384615,-0.4,-0.384615384615385,-0.369230769230769,
-0.353846153846154,-0.338461538461538,-0.323076923076923,-0.307692307692308,
-0.292307692307692,-0.276923076923077,-0.261538461538462,-0.246153846153846,
-0.230769230769231,-0.215384615384615,-0.2,-0.184615384615385,-0.169230769230769,
-0.153846153846154,-0.138461538461538,-0.123076923076923,-0.107692307692308,
-0.0923076923076923,-0.0769230769230769,-0.0615384615384615,-0.0461538461538462,
-0.0307692307692308,-0.0153846153846154,0.),.UNSPECIFIED.)
CURVE()
GEOMETRIC_REPRESENTATION_ITEM()
RATIONAL_B_SPLINE_CURVE((1.,1.,1.,1.,1.,1.,1.,1.,1.,1.,1.,1.,1.,1.,1.,1.,
1.,1.,1.,1.,1.,1.,1.,1.,1.,1.,1.,1.,1.,1.,1.,1.,1.,1.,1.,1.,1.,1.,1.,1.,
1.,1.,1.,1.,1.,1.,1.,1.,1.,1.,1.,1.,1.,1.,1.,1.,1.,1.,1.,1.,1.,1.,1.,1.,
1.,1.,1.,1.,1.,1.))
REPRESENTATION_ITEM('')
);
#211=(
BOUNDED_CURVE()
B_SPLINE_CURVE(5,(#34115,#34116,#34117,#34118,#34119,#34120,#34121,#34122,
#34123,#34124,#34125,#34126,#34127,#34128,#34129,#34130,#34131,#34132,#34133,
#34134,#34135,#34136,#34137,#34138,#34139,#34140,#34141,#34142,#34143,#34144,
#34145,#34146,#34147,#34148,#34149,#34150,#34151,#34152,#34153,#34154,#34155,
#34156,#34157,#34158,#34159,#34160,#34161,#34162,#34163,#34164,#34165,#34166,
#34167,#34168,#34169,#34170,#34171,#34172,#34173,#34174,#34175,#34176,#34177,
#34178,#34179,#34180,#34181,#34182,#34183,#34184),.UNSPECIFIED.,.F.,.F.)
B_SPLINE_CURVE_WITH_KNOTS((6,1,1,1,1,1,1,1,1,1,1,1,1,1,1,1,1,1,1,1,1,1,
1,1,1,1,1,1,1,1,1,1,1,1,1,1,1,1,1,1,1,1,1,1,1,1,1,1,1,1,1,1,1,1,1,1,1,1,
1,1,1,1,1,1,1,6),(0.00577184337450058,0.0153846153846154,0.0307692307692308,
0.0461538461538462,0.0615384615384615,0.0769230769230769,0.0923076923076923,
0.107692307692308,0.123076923076923,0.138461538461538,0.153846153846154,
0.169230769230769,0.184615384615385,0.2,0.215384615384615,0.230769230769231,
0.246153846153846,0.261538461538462,0.276923076923077,0.292307692307692,
0.307692307692308,0.323076923076923,0.338461538461538,0.353846153846154,
0.369230769230769,0.384615384615385,0.4,0.415384615384615,0.430769230769231,
0.446153846153846,0.461538461538462,0.476923076923077,0.492307692307692,
0.507692307692308,0.523076923076923,0.538461538461538,0.553846153846154,
0.569230769230769,0.584615384615384,0.6,0.615384615384615,0.63076923076923,
0.646153846153846,0.661538461538461,0.676923076923076,0.692307692307692,
0.707692307692307,0.723076923076922,0.738461538461538,0.753846153846153,
0.769230769230768,0.784615384615384,0.799999999999999,0.815384615384614,
0.83076923076923,0.846153846153845,0.86153846153846,0.876923076923076,0.892307692307691,
0.907692307692306,0.923076923076922,0.938461538461537,0.953846153846152,
0.969230769230768,0.984615384615383,1.),.UNSPECIFIED.)
CURVE()
GEOMETRIC_REPRESENTATION_ITEM()
RATIONAL_B_SPLINE_CURVE((1.,1.,1.,1.,1.,1.,1.,1.,1.,1.,1.,1.,1.,1.,1.,1.,
1.,1.,1.,1.,1.,1.,1.,1.,1.,1.,1.,1.,1.,1.,1.,1.,1.,1.,1.,1.,1.,1.,1.,1.,
1.,1.,1.,1.,1.,1.,1.,1.,1.,1.,1.,1.,1.,1.,1.,1.,1.,1.,1.,1.,1.,1.,1.,1.,
1.,1.,1.,1.,1.,1.))
REPRESENTATION_ITEM('')
);
#212=(
BOUNDED_CURVE()
B_SPLINE_CURVE(5,(#34188,#34189,#34190,#34191,#34192,#34193,#34194,#34195,
#34196,#34197,#34198,#34199,#34200,#34201,#34202,#34203,#34204,#34205,#34206,
#34207,#34208,#34209,#34210,#34211,#34212,#34213,#34214,#34215,#34216,#34217,
#34218,#34219,#34220,#34221,#34222,#34223,#34224,#34225,#34226,#34227,#34228,
#34229,#34230,#34231,#34232,#34233,#34234,#34235,#34236,#34237,#34238,#34239,
#34240,#34241,#34242,#34243,#34244,#34245,#34246,#34247,#34248,#34249,#34250,
#34251,#34252,#34253,#34254,#34255,#34256,#34257),.UNSPECIFIED.,.F.,.F.)
B_SPLINE_CURVE_WITH_KNOTS((6,1,1,1,1,1,1,1,1,1,1,1,1,1,1,1,1,1,1,1,1,1,
1,1,1,1,1,1,1,1,1,1,1,1,1,1,1,1,1,1,1,1,1,1,1,1,1,1,1,1,1,1,1,1,1,1,1,1,
1,1,1,1,1,1,1,6),(0.,0.0153846153846154,0.0307692307692308,0.0461538461538462,
0.0615384615384615,0.0769230769230769,0.0923076923076923,0.107692307692308,
0.123076923076923,0.138461538461538,0.153846153846154,0.169230769230769,
0.184615384615385,0.2,0.215384615384615,0.230769230769231,0.246153846153846,
0.261538461538462,0.276923076923077,0.292307692307692,0.307692307692308,
0.323076923076923,0.338461538461538,0.353846153846154,0.369230769230769,
0.384615384615385,0.4,0.415384615384615,0.430769230769231,0.446153846153846,
0.461538461538462,0.476923076923077,0.492307692307692,0.507692307692308,
0.523076923076923,0.538461538461538,0.553846153846154,0.569230769230769,
0.584615384615384,0.6,0.615384615384615,0.63076923076923,0.646153846153846,
0.661538461538461,0.676923076923076,0.692307692307692,0.707692307692307,
0.723076923076922,0.738461538461538,0.753846153846153,0.769230769230768,
0.784615384615384,0.799999999999999,0.815384615384614,0.83076923076923,
0.846153846153845,0.86153846153846,0.876923076923076,0.892307692307691,
0.907692307692306,0.923076923076922,0.938461538461537,0.953846153846152,
0.969230769230768,0.984615384615383,0.994228156739708),.UNSPECIFIED.)
CURVE()
GEOMETRIC_REPRESENTATION_ITEM()
RATIONAL_B_SPLINE_CURVE((1.,1.,1.,1.,1.,1.,1.,1.,1.,1.,1.,1.,1.,1.,1.,1.,
1.,1.,1.,1.,1.,1.,1.,1.,1.,1.,1.,1.,1.,1.,1.,1.,1.,1.,1.,1.,1.,1.,1.,1.,
1.,1.,1.,1.,1.,1.,1.,1.,1.,1.,1.,1.,1.,1.,1.,1.,1.,1.,1.,1.,1.,1.,1.,1.,
1.,1.,1.,1.,1.,1.))
REPRESENTATION_ITEM('')
);
#213=(
BOUNDED_CURVE()
B_SPLINE_CURVE(5,(#34261,#34262,#34263,#34264,#34265,#34266,#34267,#34268,
#34269,#34270,#34271,#34272,#34273,#34274,#34275,#34276,#34277,#34278,#34279,
#34280,#34281,#34282,#34283,#34284,#34285,#34286,#34287,#34288,#34289,#34290,
#34291,#34292,#34293,#34294,#34295,#34296,#34297,#34298,#34299,#34300,#34301,
#34302,#34303,#34304,#34305,#34306,#34307,#34308,#34309,#34310,#34311,#34312,
#34313,#34314,#34315,#34316,#34317,#34318,#34319,#34320,#34321,#34322,#34323,
#34324,#34325,#34326,#34327,#34328,#34329,#34330),.UNSPECIFIED.,.F.,.F.)
B_SPLINE_CURVE_WITH_KNOTS((6,1,1,1,1,1,1,1,1,1,1,1,1,1,1,1,1,1,1,1,1,1,
1,1,1,1,1,1,1,1,1,1,1,1,1,1,1,1,1,1,1,1,1,1,1,1,1,1,1,1,1,1,1,1,1,1,1,1,
1,1,1,1,1,1,1,6),(0.0057718433745091,0.0153846153846154,0.0307692307692308,
0.0461538461538462,0.0615384615384615,0.0769230769230769,0.0923076923076923,
0.107692307692308,0.123076923076923,0.138461538461538,0.153846153846154,
0.169230769230769,0.184615384615385,0.2,0.215384615384615,0.230769230769231,
0.246153846153846,0.261538461538462,0.276923076923077,0.292307692307692,
0.307692307692308,0.323076923076923,0.338461538461538,0.353846153846154,
0.369230769230769,0.384615384615385,0.4,0.415384615384615,0.430769230769231,
0.446153846153846,0.461538461538462,0.476923076923077,0.492307692307692,
0.507692307692308,0.523076923076923,0.538461538461538,0.553846153846154,
0.569230769230769,0.584615384615384,0.6,0.615384615384615,0.63076923076923,
0.646153846153846,0.661538461538461,0.676923076923076,0.692307692307692,
0.707692307692307,0.723076923076922,0.738461538461538,0.753846153846153,
0.769230769230768,0.784615384615384,0.799999999999999,0.815384615384614,
0.83076923076923,0.846153846153845,0.86153846153846,0.876923076923076,0.892307692307691,
0.907692307692306,0.923076923076922,0.938461538461537,0.953846153846152,
0.969230769230768,0.984615384615383,1.),.UNSPECIFIED.)
CURVE()
GEOMETRIC_REPRESENTATION_ITEM()
RATIONAL_B_SPLINE_CURVE((1.,1.,1.,1.,1.,1.,1.,1.,1.,1.,1.,1.,1.,1.,1.,1.,
1.,1.,1.,1.,1.,1.,1.,1.,1.,1.,1.,1.,1.,1.,1.,1.,1.,1.,1.,1.,1.,1.,1.,1.,
1.,1.,1.,1.,1.,1.,1.,1.,1.,1.,1.,1.,1.,1.,1.,1.,1.,1.,1.,1.,1.,1.,1.,1.,
1.,1.,1.,1.,1.,1.))
REPRESENTATION_ITEM('')
);
#214=(
BOUNDED_CURVE()
B_SPLINE_CURVE(5,(#34334,#34335,#34336,#34337,#34338,#34339,#34340,#34341,
#34342,#34343,#34344,#34345,#34346,#34347,#34348,#34349,#34350,#34351,#34352,
#34353,#34354,#34355,#34356,#34357,#34358,#34359,#34360,#34361,#34362,#34363,
#34364,#34365,#34366,#34367,#34368,#34369,#34370,#34371,#34372,#34373,#34374,
#34375,#34376,#34377,#34378,#34379,#34380,#34381,#34382,#34383,#34384,#34385,
#34386,#34387,#34388,#34389,#34390,#34391,#34392,#34393,#34394,#34395,#34396,
#34397,#34398,#34399,#34400,#34401,#34402,#34403),.UNSPECIFIED.,.F.,.F.)
B_SPLINE_CURVE_WITH_KNOTS((6,1,1,1,1,1,1,1,1,1,1,1,1,1,1,1,1,1,1,1,1,1,
1,1,1,1,1,1,1,1,1,1,1,1,1,1,1,1,1,1,1,1,1,1,1,1,1,1,1,1,1,1,1,1,1,1,1,1,
1,1,1,1,1,1,1,6),(0.,0.0153846153846154,0.0307692307692308,0.0461538461538462,
0.0615384615384615,0.0769230769230769,0.0923076923076923,0.107692307692308,
0.123076923076923,0.138461538461538,0.153846153846154,0.169230769230769,
0.184615384615385,0.2,0.215384615384615,0.230769230769231,0.246153846153846,
0.261538461538462,0.276923076923077,0.292307692307692,0.307692307692308,
0.323076923076923,0.338461538461538,0.353846153846154,0.369230769230769,
0.384615384615385,0.4,0.415384615384615,0.430769230769231,0.446153846153846,
0.461538461538462,0.476923076923077,0.492307692307692,0.507692307692308,
0.523076923076923,0.538461538461538,0.553846153846154,0.569230769230769,
0.584615384615384,0.6,0.615384615384615,0.63076923076923,0.646153846153846,
0.661538461538461,0.676923076923076,0.692307692307692,0.707692307692307,
0.723076923076922,0.738461538461538,0.753846153846153,0.769230769230768,
0.784615384615384,0.799999999999999,0.815384615384614,0.83076923076923,
0.846153846153845,0.86153846153846,0.876923076923076,0.892307692307691,
0.907692307692306,0.923076923076922,0.938461538461537,0.953846153846152,
0.969230769230768,0.984615384615383,0.994228156739689),.UNSPECIFIED.)
CURVE()
GEOMETRIC_REPRESENTATION_ITEM()
RATIONAL_B_SPLINE_CURVE((1.,1.,1.,1.,1.,1.,1.,1.,1.,1.,1.,1.,1.,1.,1.,1.,
1.,1.,1.,1.,1.,1.,1.,1.,1.,1.,1.,1.,1.,1.,1.,1.,1.,1.,1.,1.,1.,1.,1.,1.,
1.,1.,1.,1.,1.,1.,1.,1.,1.,1.,1.,1.,1.,1.,1.,1.,1.,1.,1.,1.,1.,1.,1.,1.,
1.,1.,1.,1.,1.,1.))
REPRESENTATION_ITEM('')
);
#215=(
BOUNDED_CURVE()
B_SPLINE_CURVE(5,(#34407,#34408,#34409,#34410,#34411,#34412,#34413,#34414,
#34415,#34416,#34417,#34418,#34419,#34420,#34421,#34422,#34423,#34424,#34425,
#34426,#34427,#34428,#34429,#34430,#34431,#34432,#34433,#34434,#34435,#34436,
#34437,#34438,#34439,#34440,#34441,#34442,#34443,#34444,#34445,#34446,#34447,
#34448,#34449,#34450,#34451,#34452,#34453,#34454,#34455,#34456,#34457,#34458,
#34459,#34460,#34461,#34462,#34463,#34464,#34465,#34466,#34467,#34468,#34469,
#34470,#34471,#34472,#34473,#34474,#34475,#34476),.UNSPECIFIED.,.F.,.F.)
B_SPLINE_CURVE_WITH_KNOTS((6,1,1,1,1,1,1,1,1,1,1,1,1,1,1,1,1,1,1,1,1,1,
1,1,1,1,1,1,1,1,1,1,1,1,1,1,1,1,1,1,1,1,1,1,1,1,1,1,1,1,1,1,1,1,1,1,1,1,
1,1,1,1,1,1,1,6),(0.00577184337448946,0.0153846153846154,0.0307692307692308,
0.0461538461538462,0.0615384615384615,0.0769230769230769,0.0923076923076923,
0.107692307692308,0.123076923076923,0.138461538461538,0.153846153846154,
0.169230769230769,0.184615384615385,0.2,0.215384615384615,0.230769230769231,
0.246153846153846,0.261538461538462,0.276923076923077,0.292307692307692,
0.307692307692308,0.323076923076923,0.338461538461538,0.353846153846154,
0.369230769230769,0.384615384615385,0.4,0.415384615384615,0.430769230769231,
0.446153846153846,0.461538461538462,0.476923076923077,0.492307692307692,
0.507692307692308,0.523076923076923,0.538461538461538,0.553846153846154,
0.569230769230769,0.584615384615384,0.6,0.615384615384615,0.63076923076923,
0.646153846153846,0.661538461538461,0.676923076923076,0.692307692307692,
0.707692307692307,0.723076923076922,0.738461538461538,0.753846153846153,
0.769230769230768,0.784615384615384,0.799999999999999,0.815384615384614,
0.83076923076923,0.846153846153845,0.86153846153846,0.876923076923076,0.892307692307691,
0.907692307692306,0.923076923076922,0.938461538461537,0.953846153846152,
0.969230769230768,0.984615384615383,1.),.UNSPECIFIED.)
CURVE()
GEOMETRIC_REPRESENTATION_ITEM()
RATIONAL_B_SPLINE_CURVE((1.,1.,1.,1.,1.,1.,1.,1.,1.,1.,1.,1.,1.,1.,1.,1.,
1.,1.,1.,1.,1.,1.,1.,1.,1.,1.,1.,1.,1.,1.,1.,1.,1.,1.,1.,1.,1.,1.,1.,1.,
1.,1.,1.,1.,1.,1.,1.,1.,1.,1.,1.,1.,1.,1.,1.,1.,1.,1.,1.,1.,1.,1.,1.,1.,
1.,1.,1.,1.,1.,1.))
REPRESENTATION_ITEM('')
);
#216=(
BOUNDED_CURVE()
B_SPLINE_CURVE(5,(#34480,#34481,#34482,#34483,#34484,#34485,#34486,#34487,
#34488,#34489,#34490,#34491,#34492,#34493,#34494,#34495,#34496,#34497,#34498,
#34499,#34500,#34501,#34502,#34503,#34504,#34505,#34506,#34507,#34508,#34509,
#34510,#34511,#34512,#34513,#34514,#34515,#34516,#34517,#34518,#34519,#34520,
#34521,#34522,#34523,#34524,#34525,#34526,#34527,#34528,#34529,#34530,#34531,
#34532,#34533,#34534,#34535,#34536,#34537,#34538,#34539,#34540,#34541,#34542,
#34543,#34544,#34545,#34546,#34547,#34548,#34549),.UNSPECIFIED.,.F.,.F.)
B_SPLINE_CURVE_WITH_KNOTS((6,1,1,1,1,1,1,1,1,1,1,1,1,1,1,1,1,1,1,1,1,1,
1,1,1,1,1,1,1,1,1,1,1,1,1,1,1,1,1,1,1,1,1,1,1,1,1,1,1,1,1,1,1,1,1,1,1,1,
1,1,1,1,1,1,1,6),(0.,0.0153846153846154,0.0307692307692308,0.0461538461538462,
0.0615384615384615,0.0769230769230769,0.0923076923076923,0.107692307692308,
0.123076923076923,0.138461538461538,0.153846153846154,0.169230769230769,
0.184615384615385,0.2,0.215384615384615,0.230769230769231,0.246153846153846,
0.261538461538462,0.276923076923077,0.292307692307692,0.307692307692308,
0.323076923076923,0.338461538461538,0.353846153846154,0.369230769230769,
0.384615384615385,0.4,0.415384615384615,0.430769230769231,0.446153846153846,
0.461538461538462,0.476923076923077,0.492307692307692,0.507692307692308,
0.523076923076923,0.538461538461538,0.553846153846154,0.569230769230769,
0.584615384615384,0.6,0.615384615384615,0.63076923076923,0.646153846153846,
0.661538461538461,0.676923076923076,0.692307692307692,0.707692307692307,
0.723076923076922,0.738461538461538,0.753846153846153,0.769230769230768,
0.784615384615384,0.799999999999999,0.815384615384614,0.83076923076923,
0.846153846153845,0.86153846153846,0.876923076923076,0.892307692307691,
0.907692307692306,0.923076923076922,0.938461538461537,0.953846153846152,
0.969230769230768,0.984615384615383,0.994228156739718),.UNSPECIFIED.)
CURVE()
GEOMETRIC_REPRESENTATION_ITEM()
RATIONAL_B_SPLINE_CURVE((1.,1.,1.,1.,1.,1.,1.,1.,1.,1.,1.,1.,1.,1.,1.,1.,
1.,1.,1.,1.,1.,1.,1.,1.,1.,1.,1.,1.,1.,1.,1.,1.,1.,1.,1.,1.,1.,1.,1.,1.,
1.,1.,1.,1.,1.,1.,1.,1.,1.,1.,1.,1.,1.,1.,1.,1.,1.,1.,1.,1.,1.,1.,1.,1.,
1.,1.,1.,1.,1.,1.))
REPRESENTATION_ITEM('')
);
#217=(
BOUNDED_CURVE()
B_SPLINE_CURVE(5,(#34553,#34554,#34555,#34556,#34557,#34558,#34559,#34560,
#34561,#34562,#34563,#34564,#34565,#34566,#34567,#34568,#34569,#34570,#34571,
#34572,#34573,#34574,#34575,#34576,#34577,#34578,#34579,#34580,#34581,#34582,
#34583,#34584,#34585,#34586,#34587,#34588,#34589,#34590,#34591,#34592,#34593,
#34594,#34595,#34596,#34597,#34598,#34599,#34600,#34601,#34602,#34603,#34604,
#34605,#34606,#34607,#34608,#34609,#34610,#34611,#34612,#34613,#34614,#34615,
#34616,#34617,#34618,#34619,#34620,#34621,#34622),.UNSPECIFIED.,.F.,.F.)
B_SPLINE_CURVE_WITH_KNOTS((6,1,1,1,1,1,1,1,1,1,1,1,1,1,1,1,1,1,1,1,1,1,
1,1,1,1,1,1,1,1,1,1,1,1,1,1,1,1,1,1,1,1,1,1,1,1,1,1,1,1,1,1,1,1,1,1,1,1,
1,1,1,1,1,1,1,6),(0.00577184337450897,0.0153846153846154,0.0307692307692308,
0.0461538461538462,0.0615384615384615,0.0769230769230769,0.0923076923076923,
0.107692307692308,0.123076923076923,0.138461538461538,0.153846153846154,
0.169230769230769,0.184615384615385,0.2,0.215384615384615,0.230769230769231,
0.246153846153846,0.261538461538462,0.276923076923077,0.292307692307692,
0.307692307692308,0.323076923076923,0.338461538461538,0.353846153846154,
0.369230769230769,0.384615384615385,0.4,0.415384615384615,0.430769230769231,
0.446153846153846,0.461538461538462,0.476923076923077,0.492307692307692,
0.507692307692308,0.523076923076923,0.538461538461538,0.553846153846154,
0.569230769230769,0.584615384615384,0.6,0.615384615384615,0.63076923076923,
0.646153846153846,0.661538461538461,0.676923076923076,0.692307692307692,
0.707692307692307,0.723076923076922,0.738461538461538,0.753846153846153,
0.769230769230768,0.784615384615384,0.799999999999999,0.815384615384614,
0.83076923076923,0.846153846153845,0.86153846153846,0.876923076923076,0.892307692307691,
0.907692307692306,0.923076923076922,0.938461538461537,0.953846153846152,
0.969230769230768,0.984615384615383,1.),.UNSPECIFIED.)
CURVE()
GEOMETRIC_REPRESENTATION_ITEM()
RATIONAL_B_SPLINE_CURVE((1.,1.,1.,1.,1.,1.,1.,1.,1.,1.,1.,1.,1.,1.,1.,1.,
1.,1.,1.,1.,1.,1.,1.,1.,1.,1.,1.,1.,1.,1.,1.,1.,1.,1.,1.,1.,1.,1.,1.,1.,
1.,1.,1.,1.,1.,1.,1.,1.,1.,1.,1.,1.,1.,1.,1.,1.,1.,1.,1.,1.,1.,1.,1.,1.,
1.,1.,1.,1.,1.,1.))
REPRESENTATION_ITEM('')
);
#218=(
BOUNDED_CURVE()
B_SPLINE_CURVE(5,(#34626,#34627,#34628,#34629,#34630,#34631,#34632,#34633,
#34634,#34635,#34636,#34637,#34638,#34639,#34640,#34641,#34642,#34643,#34644,
#34645,#34646,#34647,#34648,#34649,#34650,#34651,#34652,#34653,#34654,#34655,
#34656,#34657,#34658,#34659,#34660,#34661,#34662,#34663,#34664,#34665,#34666,
#34667,#34668,#34669,#34670,#34671,#34672,#34673,#34674,#34675,#34676,#34677,
#34678,#34679,#34680,#34681,#34682,#34683,#34684,#34685,#34686,#34687,#34688,
#34689,#34690,#34691,#34692,#34693,#34694,#34695),.UNSPECIFIED.,.F.,.F.)
B_SPLINE_CURVE_WITH_KNOTS((6,1,1,1,1,1,1,1,1,1,1,1,1,1,1,1,1,1,1,1,1,1,
1,1,1,1,1,1,1,1,1,1,1,1,1,1,1,1,1,1,1,1,1,1,1,1,1,1,1,1,1,1,1,1,1,1,1,1,
1,1,1,1,1,1,1,6),(0.,0.0153846153846154,0.0307692307692308,0.0461538461538462,
0.0615384615384615,0.0769230769230769,0.0923076923076923,0.107692307692308,
0.123076923076923,0.138461538461538,0.153846153846154,0.169230769230769,
0.184615384615385,0.2,0.215384615384615,0.230769230769231,0.246153846153846,
0.261538461538462,0.276923076923077,0.292307692307692,0.307692307692308,
0.323076923076923,0.338461538461538,0.353846153846154,0.369230769230769,
0.384615384615385,0.4,0.415384615384615,0.430769230769231,0.446153846153846,
0.461538461538462,0.476923076923077,0.492307692307692,0.507692307692308,
0.523076923076923,0.538461538461538,0.553846153846154,0.569230769230769,
0.584615384615384,0.6,0.615384615384615,0.63076923076923,0.646153846153846,
0.661538461538461,0.676923076923076,0.692307692307692,0.707692307692307,
0.723076923076922,0.738461538461538,0.753846153846153,0.769230769230768,
0.784615384615384,0.799999999999999,0.815384615384614,0.83076923076923,
0.846153846153845,0.86153846153846,0.876923076923076,0.892307692307691,
0.907692307692306,0.923076923076922,0.938461538461537,0.953846153846152,
0.969230769230768,0.984615384615383,0.994228156739701),.UNSPECIFIED.)
CURVE()
GEOMETRIC_REPRESENTATION_ITEM()
RATIONAL_B_SPLINE_CURVE((1.,1.,1.,1.,1.,1.,1.,1.,1.,1.,1.,1.,1.,1.,1.,1.,
1.,1.,1.,1.,1.,1.,1.,1.,1.,1.,1.,1.,1.,1.,1.,1.,1.,1.,1.,1.,1.,1.,1.,1.,
1.,1.,1.,1.,1.,1.,1.,1.,1.,1.,1.,1.,1.,1.,1.,1.,1.,1.,1.,1.,1.,1.,1.,1.,
1.,1.,1.,1.,1.,1.))
REPRESENTATION_ITEM('')
);
#219=(
BOUNDED_CURVE()
B_SPLINE_CURVE(5,(#34699,#34700,#34701,#34702,#34703,#34704,#34705,#34706,
#34707,#34708,#34709,#34710,#34711,#34712,#34713,#34714,#34715,#34716,#34717,
#34718,#34719,#34720,#34721,#34722,#34723,#34724,#34725,#34726,#34727,#34728,
#34729,#34730,#34731,#34732,#34733,#34734,#34735,#34736,#34737,#34738,#34739,
#34740,#34741,#34742,#34743,#34744,#34745,#34746,#34747,#34748,#34749,#34750,
#34751,#34752,#34753,#34754,#34755,#34756,#34757,#34758,#34759,#34760,#34761,
#34762,#34763,#34764,#34765,#34766,#34767,#34768),.UNSPECIFIED.,.F.,.F.)
B_SPLINE_CURVE_WITH_KNOTS((6,1,1,1,1,1,1,1,1,1,1,1,1,1,1,1,1,1,1,1,1,1,
1,1,1,1,1,1,1,1,1,1,1,1,1,1,1,1,1,1,1,1,1,1,1,1,1,1,1,1,1,1,1,1,1,1,1,1,
1,1,1,1,1,1,1,6),(0.00577184337451001,0.0153846153846154,0.0307692307692308,
0.0461538461538462,0.0615384615384615,0.0769230769230769,0.0923076923076923,
0.107692307692308,0.123076923076923,0.138461538461538,0.153846153846154,
0.169230769230769,0.184615384615385,0.2,0.215384615384615,0.230769230769231,
0.246153846153846,0.261538461538462,0.276923076923077,0.292307692307692,
0.307692307692308,0.323076923076923,0.338461538461538,0.353846153846154,
0.369230769230769,0.384615384615385,0.4,0.415384615384615,0.430769230769231,
0.446153846153846,0.461538461538462,0.476923076923077,0.492307692307692,
0.507692307692308,0.523076923076923,0.538461538461538,0.553846153846154,
0.569230769230769,0.584615384615384,0.6,0.615384615384615,0.63076923076923,
0.646153846153846,0.661538461538461,0.676923076923076,0.692307692307692,
0.707692307692307,0.723076923076922,0.738461538461538,0.753846153846153,
0.769230769230768,0.784615384615384,0.799999999999999,0.815384615384614,
0.83076923076923,0.846153846153845,0.86153846153846,0.876923076923076,0.892307692307691,
0.907692307692306,0.923076923076922,0.938461538461537,0.953846153846152,
0.969230769230768,0.984615384615383,1.),.UNSPECIFIED.)
CURVE()
GEOMETRIC_REPRESENTATION_ITEM()
RATIONAL_B_SPLINE_CURVE((1.,1.,1.,1.,1.,1.,1.,1.,1.,1.,1.,1.,1.,1.,1.,1.,
1.,1.,1.,1.,1.,1.,1.,1.,1.,1.,1.,1.,1.,1.,1.,1.,1.,1.,1.,1.,1.,1.,1.,1.,
1.,1.,1.,1.,1.,1.,1.,1.,1.,1.,1.,1.,1.,1.,1.,1.,1.,1.,1.,1.,1.,1.,1.,1.,
1.,1.,1.,1.,1.,1.))
REPRESENTATION_ITEM('')
);
#220=(
BOUNDED_CURVE()
B_SPLINE_CURVE(5,(#34772,#34773,#34774,#34775,#34776,#34777,#34778,#34779,
#34780,#34781,#34782,#34783,#34784,#34785,#34786,#34787,#34788,#34789,#34790,
#34791,#34792,#34793,#34794,#34795,#34796,#34797,#34798,#34799,#34800,#34801,
#34802,#34803,#34804,#34805,#34806,#34807,#34808,#34809,#34810,#34811,#34812,
#34813,#34814,#34815,#34816,#34817,#34818,#34819,#34820,#34821,#34822,#34823,
#34824,#34825,#34826,#34827,#34828,#34829,#34830,#34831,#34832,#34833,#34834,
#34835,#34836,#34837,#34838,#34839,#34840,#34841),.UNSPECIFIED.,.F.,.F.)
B_SPLINE_CURVE_WITH_KNOTS((6,1,1,1,1,1,1,1,1,1,1,1,1,1,1,1,1,1,1,1,1,1,
1,1,1,1,1,1,1,1,1,1,1,1,1,1,1,1,1,1,1,1,1,1,1,1,1,1,1,1,1,1,1,1,1,1,1,1,
1,1,1,1,1,1,1,6),(0.,0.0153846153846154,0.0307692307692308,0.0461538461538462,
0.0615384615384615,0.0769230769230769,0.0923076923076923,0.107692307692308,
0.123076923076923,0.138461538461538,0.153846153846154,0.169230769230769,
0.184615384615385,0.2,0.215384615384615,0.230769230769231,0.246153846153846,
0.261538461538462,0.276923076923077,0.292307692307692,0.307692307692308,
0.323076923076923,0.338461538461538,0.353846153846154,0.369230769230769,
0.384615384615385,0.4,0.415384615384615,0.430769230769231,0.446153846153846,
0.461538461538462,0.476923076923077,0.492307692307692,0.507692307692308,
0.523076923076923,0.538461538461538,0.553846153846154,0.569230769230769,
0.584615384615384,0.6,0.615384615384615,0.63076923076923,0.646153846153846,
0.661538461538461,0.676923076923076,0.692307692307692,0.707692307692307,
0.723076923076922,0.738461538461538,0.753846153846153,0.769230769230768,
0.784615384615384,0.799999999999999,0.815384615384614,0.83076923076923,
0.846153846153845,0.86153846153846,0.876923076923076,0.892307692307691,
0.907692307692306,0.923076923076922,0.938461538461537,0.953846153846152,
0.969230769230768,0.984615384615383,0.994228156739697),.UNSPECIFIED.)
CURVE()
GEOMETRIC_REPRESENTATION_ITEM()
RATIONAL_B_SPLINE_CURVE((1.,1.,1.,1.,1.,1.,1.,1.,1.,1.,1.,1.,1.,1.,1.,1.,
1.,1.,1.,1.,1.,1.,1.,1.,1.,1.,1.,1.,1.,1.,1.,1.,1.,1.,1.,1.,1.,1.,1.,1.,
1.,1.,1.,1.,1.,1.,1.,1.,1.,1.,1.,1.,1.,1.,1.,1.,1.,1.,1.,1.,1.,1.,1.,1.,
1.,1.,1.,1.,1.,1.))
REPRESENTATION_ITEM('')
);
#221=(
BOUNDED_CURVE()
B_SPLINE_CURVE(5,(#34845,#34846,#34847,#34848,#34849,#34850,#34851,#34852,
#34853,#34854,#34855,#34856,#34857,#34858,#34859,#34860,#34861,#34862,#34863,
#34864,#34865,#34866,#34867,#34868,#34869,#34870,#34871,#34872,#34873,#34874,
#34875,#34876,#34877,#34878,#34879,#34880,#34881,#34882,#34883,#34884,#34885,
#34886,#34887,#34888,#34889,#34890,#34891,#34892,#34893,#34894,#34895,#34896,
#34897,#34898,#34899,#34900,#34901,#34902,#34903,#34904,#34905,#34906,#34907,
#34908,#34909,#34910,#34911,#34912,#34913,#34914),.UNSPECIFIED.,.F.,.F.)
B_SPLINE_CURVE_WITH_KNOTS((6,1,1,1,1,1,1,1,1,1,1,1,1,1,1,1,1,1,1,1,1,1,
1,1,1,1,1,1,1,1,1,1,1,1,1,1,1,1,1,1,1,1,1,1,1,1,1,1,1,1,1,1,1,1,1,1,1,1,
1,1,1,1,1,1,1,6),(0.00577184337452306,0.0153846153846154,0.0307692307692308,
0.0461538461538462,0.0615384615384615,0.0769230769230769,0.0923076923076923,
0.107692307692308,0.123076923076923,0.138461538461538,0.153846153846154,
0.169230769230769,0.184615384615385,0.2,0.215384615384615,0.230769230769231,
0.246153846153846,0.261538461538462,0.276923076923077,0.292307692307692,
0.307692307692308,0.323076923076923,0.338461538461538,0.353846153846154,
0.369230769230769,0.384615384615385,0.4,0.415384615384615,0.430769230769231,
0.446153846153846,0.461538461538462,0.476923076923077,0.492307692307692,
0.507692307692308,0.523076923076923,0.538461538461538,0.553846153846154,
0.569230769230769,0.584615384615384,0.6,0.615384615384615,0.63076923076923,
0.646153846153846,0.661538461538461,0.676923076923076,0.692307692307692,
0.707692307692307,0.723076923076922,0.738461538461538,0.753846153846153,
0.769230769230768,0.784615384615384,0.799999999999999,0.815384615384614,
0.83076923076923,0.846153846153845,0.86153846153846,0.876923076923076,0.892307692307691,
0.907692307692306,0.923076923076922,0.938461538461537,0.953846153846152,
0.969230769230768,0.984615384615383,1.),.UNSPECIFIED.)
CURVE()
GEOMETRIC_REPRESENTATION_ITEM()
RATIONAL_B_SPLINE_CURVE((1.,1.,1.,1.,1.,1.,1.,1.,1.,1.,1.,1.,1.,1.,1.,1.,
1.,1.,1.,1.,1.,1.,1.,1.,1.,1.,1.,1.,1.,1.,1.,1.,1.,1.,1.,1.,1.,1.,1.,1.,
1.,1.,1.,1.,1.,1.,1.,1.,1.,1.,1.,1.,1.,1.,1.,1.,1.,1.,1.,1.,1.,1.,1.,1.,
1.,1.,1.,1.,1.,1.))
REPRESENTATION_ITEM('')
);
#222=(
BOUNDED_CURVE()
B_SPLINE_CURVE(5,(#34918,#34919,#34920,#34921,#34922,#34923,#34924,#34925,
#34926,#34927,#34928,#34929,#34930,#34931,#34932,#34933,#34934,#34935,#34936,
#34937,#34938,#34939,#34940,#34941,#34942,#34943,#34944,#34945,#34946,#34947,
#34948,#34949,#34950,#34951,#34952,#34953,#34954,#34955,#34956,#34957,#34958,
#34959,#34960,#34961,#34962,#34963,#34964,#34965,#34966,#34967,#34968,#34969,
#34970,#34971,#34972,#34973,#34974,#34975,#34976,#34977,#34978,#34979,#34980,
#34981,#34982,#34983,#34984,#34985,#34986,#34987),.UNSPECIFIED.,.F.,.F.)
B_SPLINE_CURVE_WITH_KNOTS((6,1,1,1,1,1,1,1,1,1,1,1,1,1,1,1,1,1,1,1,1,1,
1,1,1,1,1,1,1,1,1,1,1,1,1,1,1,1,1,1,1,1,1,1,1,1,1,1,1,1,1,1,1,1,1,1,1,1,
1,1,1,1,1,1,1,6),(0.,0.0153846153846154,0.0307692307692308,0.0461538461538462,
0.0615384615384615,0.0769230769230769,0.0923076923076923,0.107692307692308,
0.123076923076923,0.138461538461538,0.153846153846154,0.169230769230769,
0.184615384615385,0.2,0.215384615384615,0.230769230769231,0.246153846153846,
0.261538461538462,0.276923076923077,0.292307692307692,0.307692307692308,
0.323076923076923,0.338461538461538,0.353846153846154,0.369230769230769,
0.384615384615385,0.4,0.415384615384615,0.430769230769231,0.446153846153846,
0.461538461538462,0.476923076923077,0.492307692307692,0.507692307692308,
0.523076923076923,0.538461538461538,0.553846153846154,0.569230769230769,
0.584615384615384,0.6,0.615384615384615,0.63076923076923,0.646153846153846,
0.661538461538461,0.676923076923076,0.692307692307692,0.707692307692307,
0.723076923076922,0.738461538461538,0.753846153846153,0.769230769230768,
0.784615384615384,0.799999999999999,0.815384615384614,0.83076923076923,
0.846153846153845,0.86153846153846,0.876923076923076,0.892307692307691,
0.907692307692306,0.923076923076922,0.938461538461537,0.953846153846152,
0.969230769230768,0.984615384615383,0.994228156739688),.UNSPECIFIED.)
CURVE()
GEOMETRIC_REPRESENTATION_ITEM()
RATIONAL_B_SPLINE_CURVE((1.,1.,1.,1.,1.,1.,1.,1.,1.,1.,1.,1.,1.,1.,1.,1.,
1.,1.,1.,1.,1.,1.,1.,1.,1.,1.,1.,1.,1.,1.,1.,1.,1.,1.,1.,1.,1.,1.,1.,1.,
1.,1.,1.,1.,1.,1.,1.,1.,1.,1.,1.,1.,1.,1.,1.,1.,1.,1.,1.,1.,1.,1.,1.,1.,
1.,1.,1.,1.,1.,1.))
REPRESENTATION_ITEM('')
);
#223=(
BOUNDED_CURVE()
B_SPLINE_CURVE(5,(#34991,#34992,#34993,#34994,#34995,#34996,#34997,#34998,
#34999,#35000,#35001,#35002,#35003,#35004,#35005,#35006,#35007,#35008,#35009,
#35010,#35011,#35012,#35013,#35014,#35015,#35016,#35017,#35018,#35019,#35020,
#35021,#35022,#35023,#35024,#35025,#35026,#35027,#35028,#35029,#35030,#35031,
#35032,#35033,#35034,#35035,#35036,#35037,#35038,#35039,#35040,#35041,#35042,
#35043,#35044,#35045,#35046,#35047,#35048,#35049,#35050,#35051,#35052,#35053,
#35054,#35055,#35056,#35057,#35058,#35059,#35060),.UNSPECIFIED.,.F.,.F.)
B_SPLINE_CURVE_WITH_KNOTS((6,1,1,1,1,1,1,1,1,1,1,1,1,1,1,1,1,1,1,1,1,1,
1,1,1,1,1,1,1,1,1,1,1,1,1,1,1,1,1,1,1,1,1,1,1,1,1,1,1,1,1,1,1,1,1,1,1,1,
1,1,1,1,1,1,1,6),(0.00577184337449862,0.0153846153846154,0.0307692307692308,
0.0461538461538462,0.0615384615384615,0.0769230769230769,0.0923076923076923,
0.107692307692308,0.123076923076923,0.138461538461538,0.153846153846154,
0.169230769230769,0.184615384615385,0.2,0.215384615384615,0.230769230769231,
0.246153846153846,0.261538461538462,0.276923076923077,0.292307692307692,
0.307692307692308,0.323076923076923,0.338461538461538,0.353846153846154,
0.369230769230769,0.384615384615385,0.4,0.415384615384615,0.430769230769231,
0.446153846153846,0.461538461538462,0.476923076923077,0.492307692307692,
0.507692307692308,0.523076923076923,0.538461538461538,0.553846153846154,
0.569230769230769,0.584615384615384,0.6,0.615384615384615,0.63076923076923,
0.646153846153846,0.661538461538461,0.676923076923076,0.692307692307692,
0.707692307692307,0.723076923076922,0.738461538461538,0.753846153846153,
0.769230769230768,0.784615384615384,0.799999999999999,0.815384615384614,
0.83076923076923,0.846153846153845,0.86153846153846,0.876923076923076,0.892307692307691,
0.907692307692306,0.923076923076922,0.938461538461537,0.953846153846152,
0.969230769230768,0.984615384615383,1.),.UNSPECIFIED.)
CURVE()
GEOMETRIC_REPRESENTATION_ITEM()
RATIONAL_B_SPLINE_CURVE((1.,1.,1.,1.,1.,1.,1.,1.,1.,1.,1.,1.,1.,1.,1.,1.,
1.,1.,1.,1.,1.,1.,1.,1.,1.,1.,1.,1.,1.,1.,1.,1.,1.,1.,1.,1.,1.,1.,1.,1.,
1.,1.,1.,1.,1.,1.,1.,1.,1.,1.,1.,1.,1.,1.,1.,1.,1.,1.,1.,1.,1.,1.,1.,1.,
1.,1.,1.,1.,1.,1.))
REPRESENTATION_ITEM('')
);
#224=(
BOUNDED_CURVE()
B_SPLINE_CURVE(5,(#35064,#35065,#35066,#35067,#35068,#35069,#35070,#35071,
#35072,#35073,#35074,#35075,#35076,#35077,#35078,#35079,#35080,#35081,#35082,
#35083,#35084,#35085,#35086,#35087,#35088,#35089,#35090,#35091,#35092,#35093,
#35094,#35095,#35096,#35097,#35098,#35099,#35100,#35101,#35102,#35103,#35104,
#35105,#35106,#35107,#35108,#35109,#35110,#35111,#35112,#35113,#35114,#35115,
#35116,#35117,#35118,#35119,#35120,#35121,#35122,#35123,#35124,#35125,#35126,
#35127,#35128,#35129,#35130,#35131,#35132,#35133),.UNSPECIFIED.,.F.,.F.)
B_SPLINE_CURVE_WITH_KNOTS((6,1,1,1,1,1,1,1,1,1,1,1,1,1,1,1,1,1,1,1,1,1,
1,1,1,1,1,1,1,1,1,1,1,1,1,1,1,1,1,1,1,1,1,1,1,1,1,1,1,1,1,1,1,1,1,1,1,1,
1,1,1,1,1,1,1,6),(0.,0.0153846153846154,0.0307692307692308,0.0461538461538462,
0.0615384615384615,0.0769230769230769,0.0923076923076923,0.107692307692308,
0.123076923076923,0.138461538461538,0.153846153846154,0.169230769230769,
0.184615384615385,0.2,0.215384615384615,0.230769230769231,0.246153846153846,
0.261538461538462,0.276923076923077,0.292307692307692,0.307692307692308,
0.323076923076923,0.338461538461538,0.353846153846154,0.369230769230769,
0.384615384615385,0.4,0.415384615384615,0.430769230769231,0.446153846153846,
0.461538461538462,0.476923076923077,0.492307692307692,0.507692307692308,
0.523076923076923,0.538461538461538,0.553846153846154,0.569230769230769,
0.584615384615384,0.6,0.615384615384615,0.63076923076923,0.646153846153846,
0.661538461538461,0.676923076923076,0.692307692307692,0.707692307692307,
0.723076923076922,0.738461538461538,0.753846153846153,0.769230769230768,
0.784615384615384,0.799999999999999,0.815384615384614,0.83076923076923,
0.846153846153845,0.86153846153846,0.876923076923076,0.892307692307691,
0.907692307692306,0.923076923076922,0.938461538461537,0.953846153846152,
0.969230769230768,0.984615384615383,0.994228156739696),.UNSPECIFIED.)
CURVE()
GEOMETRIC_REPRESENTATION_ITEM()
RATIONAL_B_SPLINE_CURVE((1.,1.,1.,1.,1.,1.,1.,1.,1.,1.,1.,1.,1.,1.,1.,1.,
1.,1.,1.,1.,1.,1.,1.,1.,1.,1.,1.,1.,1.,1.,1.,1.,1.,1.,1.,1.,1.,1.,1.,1.,
1.,1.,1.,1.,1.,1.,1.,1.,1.,1.,1.,1.,1.,1.,1.,1.,1.,1.,1.,1.,1.,1.,1.,1.,
1.,1.,1.,1.,1.,1.))
REPRESENTATION_ITEM('')
);
#225=(
BOUNDED_CURVE()
B_SPLINE_CURVE(5,(#35137,#35138,#35139,#35140,#35141,#35142,#35143,#35144,
#35145,#35146,#35147,#35148,#35149,#35150,#35151,#35152,#35153,#35154,#35155,
#35156,#35157,#35158,#35159,#35160,#35161,#35162,#35163,#35164,#35165,#35166,
#35167,#35168,#35169,#35170,#35171,#35172,#35173,#35174,#35175,#35176,#35177,
#35178,#35179,#35180,#35181,#35182,#35183,#35184,#35185,#35186,#35187,#35188,
#35189,#35190,#35191,#35192,#35193,#35194,#35195,#35196,#35197,#35198,#35199,
#35200,#35201,#35202,#35203,#35204,#35205,#35206),.UNSPECIFIED.,.F.,.F.)
B_SPLINE_CURVE_WITH_KNOTS((6,1,1,1,1,1,1,1,1,1,1,1,1,1,1,1,1,1,1,1,1,1,
1,1,1,1,1,1,1,1,1,1,1,1,1,1,1,1,1,1,1,1,1,1,1,1,1,1,1,1,1,1,1,1,1,1,1,1,
1,1,1,1,1,1,1,6),(0.00577184337452068,0.0153846153846154,0.0307692307692308,
0.0461538461538462,0.0615384615384615,0.0769230769230769,0.0923076923076923,
0.107692307692308,0.123076923076923,0.138461538461538,0.153846153846154,
0.169230769230769,0.184615384615385,0.2,0.215384615384615,0.230769230769231,
0.246153846153846,0.261538461538462,0.276923076923077,0.292307692307692,
0.307692307692308,0.323076923076923,0.338461538461538,0.353846153846154,
0.369230769230769,0.384615384615385,0.4,0.415384615384615,0.430769230769231,
0.446153846153846,0.461538461538462,0.476923076923077,0.492307692307692,
0.507692307692308,0.523076923076923,0.538461538461538,0.553846153846154,
0.569230769230769,0.584615384615384,0.6,0.615384615384615,0.63076923076923,
0.646153846153846,0.661538461538461,0.676923076923076,0.692307692307692,
0.707692307692307,0.723076923076922,0.738461538461538,0.753846153846153,
0.769230769230768,0.784615384615384,0.799999999999999,0.815384615384614,
0.83076923076923,0.846153846153845,0.86153846153846,0.876923076923076,0.892307692307691,
0.907692307692306,0.923076923076922,0.938461538461537,0.953846153846152,
0.969230769230768,0.984615384615383,1.),.UNSPECIFIED.)
CURVE()
GEOMETRIC_REPRESENTATION_ITEM()
RATIONAL_B_SPLINE_CURVE((1.,1.,1.,1.,1.,1.,1.,1.,1.,1.,1.,1.,1.,1.,1.,1.,
1.,1.,1.,1.,1.,1.,1.,1.,1.,1.,1.,1.,1.,1.,1.,1.,1.,1.,1.,1.,1.,1.,1.,1.,
1.,1.,1.,1.,1.,1.,1.,1.,1.,1.,1.,1.,1.,1.,1.,1.,1.,1.,1.,1.,1.,1.,1.,1.,
1.,1.,1.,1.,1.,1.))
REPRESENTATION_ITEM('')
);
#226=(
BOUNDED_CURVE()
B_SPLINE_CURVE(5,(#35210,#35211,#35212,#35213,#35214,#35215,#35216,#35217,
#35218,#35219,#35220,#35221,#35222,#35223,#35224,#35225,#35226,#35227,#35228,
#35229,#35230,#35231,#35232,#35233,#35234,#35235,#35236,#35237,#35238,#35239,
#35240,#35241,#35242,#35243,#35244,#35245,#35246,#35247,#35248,#35249,#35250,
#35251,#35252,#35253,#35254,#35255,#35256,#35257,#35258,#35259,#35260,#35261,
#35262,#35263,#35264,#35265,#35266,#35267,#35268,#35269,#35270,#35271,#35272,
#35273,#35274,#35275,#35276,#35277,#35278,#35279),.UNSPECIFIED.,.F.,.F.)
B_SPLINE_CURVE_WITH_KNOTS((6,1,1,1,1,1,1,1,1,1,1,1,1,1,1,1,1,1,1,1,1,1,
1,1,1,1,1,1,1,1,1,1,1,1,1,1,1,1,1,1,1,1,1,1,1,1,1,1,1,1,1,1,1,1,1,1,1,1,
1,1,1,1,1,1,1,6),(0.,0.0153846153846154,0.0307692307692308,0.0461538461538462,
0.0615384615384615,0.0769230769230769,0.0923076923076923,0.107692307692308,
0.123076923076923,0.138461538461538,0.153846153846154,0.169230769230769,
0.184615384615385,0.2,0.215384615384615,0.230769230769231,0.246153846153846,
0.261538461538462,0.276923076923077,0.292307692307692,0.307692307692308,
0.323076923076923,0.338461538461538,0.353846153846154,0.369230769230769,
0.384615384615385,0.4,0.415384615384615,0.430769230769231,0.446153846153846,
0.461538461538462,0.476923076923077,0.492307692307692,0.507692307692308,
0.523076923076923,0.538461538461538,0.553846153846154,0.569230769230769,
0.584615384615384,0.6,0.615384615384615,0.63076923076923,0.646153846153846,
0.661538461538461,0.676923076923076,0.692307692307692,0.707692307692307,
0.723076923076922,0.738461538461538,0.753846153846153,0.769230769230768,
0.784615384615384,0.799999999999999,0.815384615384614,0.83076923076923,
0.846153846153845,0.86153846153846,0.876923076923076,0.892307692307691,
0.907692307692306,0.923076923076922,0.938461538461537,0.953846153846152,
0.969230769230768,0.984615384615383,0.994228156739698),.UNSPECIFIED.)
CURVE()
GEOMETRIC_REPRESENTATION_ITEM()
RATIONAL_B_SPLINE_CURVE((1.,1.,1.,1.,1.,1.,1.,1.,1.,1.,1.,1.,1.,1.,1.,1.,
1.,1.,1.,1.,1.,1.,1.,1.,1.,1.,1.,1.,1.,1.,1.,1.,1.,1.,1.,1.,1.,1.,1.,1.,
1.,1.,1.,1.,1.,1.,1.,1.,1.,1.,1.,1.,1.,1.,1.,1.,1.,1.,1.,1.,1.,1.,1.,1.,
1.,1.,1.,1.,1.,1.))
REPRESENTATION_ITEM('')
);
#227=(
BOUNDED_CURVE()
B_SPLINE_CURVE(5,(#35283,#35284,#35285,#35286,#35287,#35288,#35289,#35290,
#35291,#35292,#35293,#35294,#35295,#35296,#35297,#35298,#35299,#35300,#35301,
#35302,#35303,#35304,#35305,#35306,#35307,#35308,#35309,#35310,#35311,#35312,
#35313,#35314,#35315,#35316,#35317,#35318,#35319,#35320,#35321,#35322,#35323,
#35324,#35325,#35326,#35327,#35328,#35329,#35330,#35331,#35332,#35333,#35334,
#35335,#35336,#35337,#35338,#35339,#35340,#35341,#35342,#35343,#35344,#35345,
#35346,#35347,#35348,#35349,#35350,#35351,#35352),.UNSPECIFIED.,.F.,.F.)
B_SPLINE_CURVE_WITH_KNOTS((6,1,1,1,1,1,1,1,1,1,1,1,1,1,1,1,1,1,1,1,1,1,
1,1,1,1,1,1,1,1,1,1,1,1,1,1,1,1,1,1,1,1,1,1,1,1,1,1,1,1,1,1,1,1,1,1,1,1,
1,1,1,1,1,1,1,6),(0.00577184337451607,0.0153846153846154,0.0307692307692308,
0.0461538461538462,0.0615384615384615,0.0769230769230769,0.0923076923076923,
0.107692307692308,0.123076923076923,0.138461538461538,0.153846153846154,
0.169230769230769,0.184615384615385,0.2,0.215384615384615,0.230769230769231,
0.246153846153846,0.261538461538462,0.276923076923077,0.292307692307692,
0.307692307692308,0.323076923076923,0.338461538461538,0.353846153846154,
0.369230769230769,0.384615384615385,0.4,0.415384615384615,0.430769230769231,
0.446153846153846,0.461538461538462,0.476923076923077,0.492307692307692,
0.507692307692308,0.523076923076923,0.538461538461538,0.553846153846154,
0.569230769230769,0.584615384615384,0.6,0.615384615384615,0.63076923076923,
0.646153846153846,0.661538461538461,0.676923076923076,0.692307692307692,
0.707692307692307,0.723076923076922,0.738461538461538,0.753846153846153,
0.769230769230768,0.784615384615384,0.799999999999999,0.815384615384614,
0.83076923076923,0.846153846153845,0.86153846153846,0.876923076923076,0.892307692307691,
0.907692307692306,0.923076923076922,0.938461538461537,0.953846153846152,
0.969230769230768,0.984615384615383,1.),.UNSPECIFIED.)
CURVE()
GEOMETRIC_REPRESENTATION_ITEM()
RATIONAL_B_SPLINE_CURVE((1.,1.,1.,1.,1.,1.,1.,1.,1.,1.,1.,1.,1.,1.,1.,1.,
1.,1.,1.,1.,1.,1.,1.,1.,1.,1.,1.,1.,1.,1.,1.,1.,1.,1.,1.,1.,1.,1.,1.,1.,
1.,1.,1.,1.,1.,1.,1.,1.,1.,1.,1.,1.,1.,1.,1.,1.,1.,1.,1.,1.,1.,1.,1.,1.,
1.,1.,1.,1.,1.,1.))
REPRESENTATION_ITEM('')
);
#228=(
BOUNDED_CURVE()
B_SPLINE_CURVE(5,(#35356,#35357,#35358,#35359,#35360,#35361,#35362,#35363,
#35364,#35365,#35366,#35367,#35368,#35369,#35370,#35371,#35372,#35373,#35374,
#35375,#35376,#35377,#35378,#35379,#35380,#35381,#35382,#35383,#35384,#35385,
#35386,#35387,#35388,#35389,#35390,#35391,#35392,#35393,#35394,#35395,#35396,
#35397,#35398,#35399,#35400,#35401,#35402,#35403,#35404,#35405,#35406,#35407,
#35408,#35409,#35410,#35411,#35412,#35413,#35414,#35415,#35416,#35417,#35418,
#35419,#35420,#35421,#35422,#35423,#35424,#35425),.UNSPECIFIED.,.F.,.F.)
B_SPLINE_CURVE_WITH_KNOTS((6,1,1,1,1,1,1,1,1,1,1,1,1,1,1,1,1,1,1,1,1,1,
1,1,1,1,1,1,1,1,1,1,1,1,1,1,1,1,1,1,1,1,1,1,1,1,1,1,1,1,1,1,1,1,1,1,1,1,
1,1,1,1,1,1,1,6),(0.,0.0153846153846154,0.0307692307692308,0.0461538461538462,
0.0615384615384615,0.0769230769230769,0.0923076923076923,0.107692307692308,
0.123076923076923,0.138461538461538,0.153846153846154,0.169230769230769,
0.184615384615385,0.2,0.215384615384615,0.230769230769231,0.246153846153846,
0.261538461538462,0.276923076923077,0.292307692307692,0.307692307692308,
0.323076923076923,0.338461538461538,0.353846153846154,0.369230769230769,
0.384615384615385,0.4,0.415384615384615,0.430769230769231,0.446153846153846,
0.461538461538462,0.476923076923077,0.492307692307692,0.507692307692308,
0.523076923076923,0.538461538461538,0.553846153846154,0.569230769230769,
0.584615384615384,0.6,0.615384615384615,0.63076923076923,0.646153846153846,
0.661538461538461,0.676923076923076,0.692307692307692,0.707692307692307,
0.723076923076922,0.738461538461538,0.753846153846153,0.769230769230768,
0.784615384615384,0.799999999999999,0.815384615384614,0.83076923076923,
0.846153846153845,0.86153846153846,0.876923076923076,0.892307692307691,
0.907692307692306,0.923076923076922,0.938461538461537,0.953846153846152,
0.969230769230768,0.984615384615383,0.994228156739704),.UNSPECIFIED.)
CURVE()
GEOMETRIC_REPRESENTATION_ITEM()
RATIONAL_B_SPLINE_CURVE((1.,1.,1.,1.,1.,1.,1.,1.,1.,1.,1.,1.,1.,1.,1.,1.,
1.,1.,1.,1.,1.,1.,1.,1.,1.,1.,1.,1.,1.,1.,1.,1.,1.,1.,1.,1.,1.,1.,1.,1.,
1.,1.,1.,1.,1.,1.,1.,1.,1.,1.,1.,1.,1.,1.,1.,1.,1.,1.,1.,1.,1.,1.,1.,1.,
1.,1.,1.,1.,1.,1.))
REPRESENTATION_ITEM('')
);
#229=(
BOUNDED_CURVE()
B_SPLINE_CURVE(5,(#35429,#35430,#35431,#35432,#35433,#35434,#35435,#35436,
#35437,#35438,#35439,#35440,#35441,#35442,#35443,#35444,#35445,#35446,#35447,
#35448,#35449,#35450,#35451,#35452,#35453,#35454,#35455,#35456,#35457,#35458,
#35459,#35460,#35461,#35462,#35463,#35464,#35465,#35466,#35467,#35468,#35469,
#35470,#35471,#35472,#35473,#35474,#35475,#35476,#35477,#35478,#35479,#35480,
#35481,#35482,#35483,#35484,#35485,#35486,#35487,#35488,#35489,#35490,#35491,
#35492,#35493,#35494,#35495,#35496,#35497,#35498),.UNSPECIFIED.,.F.,.F.)
B_SPLINE_CURVE_WITH_KNOTS((6,1,1,1,1,1,1,1,1,1,1,1,1,1,1,1,1,1,1,1,1,1,
1,1,1,1,1,1,1,1,1,1,1,1,1,1,1,1,1,1,1,1,1,1,1,1,1,1,1,1,1,1,1,1,1,1,1,1,
1,1,1,1,1,1,1,6),(0.00577184337449692,0.0153846153846154,0.0307692307692308,
0.0461538461538462,0.0615384615384615,0.0769230769230769,0.0923076923076923,
0.107692307692308,0.123076923076923,0.138461538461538,0.153846153846154,
0.169230769230769,0.184615384615385,0.2,0.215384615384615,0.230769230769231,
0.246153846153846,0.261538461538462,0.276923076923077,0.292307692307692,
0.307692307692308,0.323076923076923,0.338461538461538,0.353846153846154,
0.369230769230769,0.384615384615385,0.4,0.415384615384615,0.430769230769231,
0.446153846153846,0.461538461538462,0.476923076923077,0.492307692307692,
0.507692307692308,0.523076923076923,0.538461538461538,0.553846153846154,
0.569230769230769,0.584615384615384,0.6,0.615384615384615,0.63076923076923,
0.646153846153846,0.661538461538461,0.676923076923076,0.692307692307692,
0.707692307692307,0.723076923076922,0.738461538461538,0.753846153846153,
0.769230769230768,0.784615384615384,0.799999999999999,0.815384615384614,
0.83076923076923,0.846153846153845,0.86153846153846,0.876923076923076,0.892307692307691,
0.907692307692306,0.923076923076922,0.938461538461537,0.953846153846152,
0.969230769230768,0.984615384615383,1.),.UNSPECIFIED.)
CURVE()
GEOMETRIC_REPRESENTATION_ITEM()
RATIONAL_B_SPLINE_CURVE((1.,1.,1.,1.,1.,1.,1.,1.,1.,1.,1.,1.,1.,1.,1.,1.,
1.,1.,1.,1.,1.,1.,1.,1.,1.,1.,1.,1.,1.,1.,1.,1.,1.,1.,1.,1.,1.,1.,1.,1.,
1.,1.,1.,1.,1.,1.,1.,1.,1.,1.,1.,1.,1.,1.,1.,1.,1.,1.,1.,1.,1.,1.,1.,1.,
1.,1.,1.,1.,1.,1.))
REPRESENTATION_ITEM('')
);
#230=(
BOUNDED_CURVE()
B_SPLINE_CURVE(5,(#35502,#35503,#35504,#35505,#35506,#35507,#35508,#35509,
#35510,#35511,#35512,#35513,#35514,#35515,#35516,#35517,#35518,#35519,#35520,
#35521,#35522,#35523,#35524,#35525,#35526,#35527,#35528,#35529,#35530,#35531,
#35532,#35533,#35534,#35535,#35536,#35537,#35538,#35539,#35540,#35541,#35542,
#35543,#35544,#35545,#35546,#35547,#35548,#35549,#35550,#35551,#35552,#35553,
#35554,#35555,#35556,#35557,#35558,#35559,#35560,#35561,#35562,#35563,#35564,
#35565,#35566,#35567,#35568,#35569,#35570,#35571),.UNSPECIFIED.,.F.,.F.)
B_SPLINE_CURVE_WITH_KNOTS((6,1,1,1,1,1,1,1,1,1,1,1,1,1,1,1,1,1,1,1,1,1,
1,1,1,1,1,1,1,1,1,1,1,1,1,1,1,1,1,1,1,1,1,1,1,1,1,1,1,1,1,1,1,1,1,1,1,1,
1,1,1,1,1,1,1,6),(0.,0.0153846153846154,0.0307692307692308,0.0461538461538462,
0.0615384615384615,0.0769230769230769,0.0923076923076923,0.107692307692308,
0.123076923076923,0.138461538461538,0.153846153846154,0.169230769230769,
0.184615384615385,0.2,0.215384615384615,0.230769230769231,0.246153846153846,
0.261538461538462,0.276923076923077,0.292307692307692,0.307692307692308,
0.323076923076923,0.338461538461538,0.353846153846154,0.369230769230769,
0.384615384615385,0.4,0.415384615384615,0.430769230769231,0.446153846153846,
0.461538461538462,0.476923076923077,0.492307692307692,0.507692307692308,
0.523076923076923,0.538461538461538,0.553846153846154,0.569230769230769,
0.584615384615384,0.6,0.615384615384615,0.63076923076923,0.646153846153846,
0.661538461538461,0.676923076923076,0.692307692307692,0.707692307692307,
0.723076923076922,0.738461538461538,0.753846153846153,0.769230769230768,
0.784615384615384,0.799999999999999,0.815384615384614,0.83076923076923,
0.846153846153845,0.86153846153846,0.876923076923076,0.892307692307691,
0.907692307692306,0.923076923076922,0.938461538461537,0.953846153846152,
0.969230769230768,0.984615384615383,0.994228156739711),.UNSPECIFIED.)
CURVE()
GEOMETRIC_REPRESENTATION_ITEM()
RATIONAL_B_SPLINE_CURVE((1.,1.,1.,1.,1.,1.,1.,1.,1.,1.,1.,1.,1.,1.,1.,1.,
1.,1.,1.,1.,1.,1.,1.,1.,1.,1.,1.,1.,1.,1.,1.,1.,1.,1.,1.,1.,1.,1.,1.,1.,
1.,1.,1.,1.,1.,1.,1.,1.,1.,1.,1.,1.,1.,1.,1.,1.,1.,1.,1.,1.,1.,1.,1.,1.,
1.,1.,1.,1.,1.,1.))
REPRESENTATION_ITEM('')
);
#231=(
BOUNDED_CURVE()
B_SPLINE_CURVE(5,(#35575,#35576,#35577,#35578,#35579,#35580,#35581,#35582,
#35583,#35584,#35585,#35586,#35587,#35588,#35589,#35590,#35591,#35592,#35593,
#35594,#35595,#35596,#35597,#35598,#35599,#35600,#35601,#35602,#35603,#35604,
#35605,#35606,#35607,#35608,#35609,#35610,#35611,#35612,#35613,#35614,#35615,
#35616,#35617,#35618,#35619,#35620,#35621,#35622,#35623,#35624,#35625,#35626,
#35627,#35628,#35629,#35630,#35631,#35632,#35633,#35634,#35635,#35636,#35637,
#35638,#35639,#35640,#35641,#35642,#35643,#35644),.UNSPECIFIED.,.F.,.F.)
B_SPLINE_CURVE_WITH_KNOTS((6,1,1,1,1,1,1,1,1,1,1,1,1,1,1,1,1,1,1,1,1,1,
1,1,1,1,1,1,1,1,1,1,1,1,1,1,1,1,1,1,1,1,1,1,1,1,1,1,1,1,1,1,1,1,1,1,1,1,
1,1,1,1,1,1,1,6),(0.00577184337450058,0.0153846153846154,0.0307692307692308,
0.0461538461538462,0.0615384615384615,0.0769230769230769,0.0923076923076923,
0.107692307692308,0.123076923076923,0.138461538461538,0.153846153846154,
0.169230769230769,0.184615384615385,0.2,0.215384615384615,0.230769230769231,
0.246153846153846,0.261538461538462,0.276923076923077,0.292307692307692,
0.307692307692308,0.323076923076923,0.338461538461538,0.353846153846154,
0.369230769230769,0.384615384615385,0.4,0.415384615384615,0.430769230769231,
0.446153846153846,0.461538461538462,0.476923076923077,0.492307692307692,
0.507692307692308,0.523076923076923,0.538461538461538,0.553846153846154,
0.569230769230769,0.584615384615384,0.6,0.615384615384615,0.63076923076923,
0.646153846153846,0.661538461538461,0.676923076923076,0.692307692307692,
0.707692307692307,0.723076923076922,0.738461538461538,0.753846153846153,
0.769230769230768,0.784615384615384,0.799999999999999,0.815384615384614,
0.83076923076923,0.846153846153845,0.86153846153846,0.876923076923076,0.892307692307691,
0.907692307692306,0.923076923076922,0.938461538461537,0.953846153846152,
0.969230769230768,0.984615384615383,1.),.UNSPECIFIED.)
CURVE()
GEOMETRIC_REPRESENTATION_ITEM()
RATIONAL_B_SPLINE_CURVE((1.,1.,1.,1.,1.,1.,1.,1.,1.,1.,1.,1.,1.,1.,1.,1.,
1.,1.,1.,1.,1.,1.,1.,1.,1.,1.,1.,1.,1.,1.,1.,1.,1.,1.,1.,1.,1.,1.,1.,1.,
1.,1.,1.,1.,1.,1.,1.,1.,1.,1.,1.,1.,1.,1.,1.,1.,1.,1.,1.,1.,1.,1.,1.,1.,
1.,1.,1.,1.,1.,1.))
REPRESENTATION_ITEM('')
);
#232=(
BOUNDED_CURVE()
B_SPLINE_CURVE(5,(#35648,#35649,#35650,#35651,#35652,#35653,#35654,#35655,
#35656,#35657,#35658,#35659,#35660,#35661,#35662,#35663,#35664,#35665,#35666,
#35667,#35668,#35669,#35670,#35671,#35672,#35673,#35674,#35675,#35676,#35677,
#35678,#35679,#35680,#35681,#35682,#35683,#35684,#35685,#35686,#35687,#35688,
#35689,#35690,#35691,#35692,#35693,#35694,#35695,#35696,#35697,#35698,#35699,
#35700,#35701,#35702,#35703,#35704,#35705,#35706,#35707,#35708,#35709,#35710,
#35711,#35712,#35713,#35714,#35715,#35716,#35717),.UNSPECIFIED.,.F.,.F.)
B_SPLINE_CURVE_WITH_KNOTS((6,1,1,1,1,1,1,1,1,1,1,1,1,1,1,1,1,1,1,1,1,1,
1,1,1,1,1,1,1,1,1,1,1,1,1,1,1,1,1,1,1,1,1,1,1,1,1,1,1,1,1,1,1,1,1,1,1,1,
1,1,1,1,1,1,1,6),(0.,0.0153846153846154,0.0307692307692308,0.0461538461538462,
0.0615384615384615,0.0769230769230769,0.0923076923076923,0.107692307692308,
0.123076923076923,0.138461538461538,0.153846153846154,0.169230769230769,
0.184615384615385,0.2,0.215384615384615,0.230769230769231,0.246153846153846,
0.261538461538462,0.276923076923077,0.292307692307692,0.307692307692308,
0.323076923076923,0.338461538461538,0.353846153846154,0.369230769230769,
0.384615384615385,0.4,0.415384615384615,0.430769230769231,0.446153846153846,
0.461538461538462,0.476923076923077,0.492307692307692,0.507692307692308,
0.523076923076923,0.538461538461538,0.553846153846154,0.569230769230769,
0.584615384615384,0.6,0.615384615384615,0.63076923076923,0.646153846153846,
0.661538461538461,0.676923076923076,0.692307692307692,0.707692307692307,
0.723076923076922,0.738461538461538,0.753846153846153,0.769230769230768,
0.784615384615384,0.799999999999999,0.815384615384614,0.83076923076923,
0.846153846153845,0.86153846153846,0.876923076923076,0.892307692307691,
0.907692307692306,0.923076923076922,0.938461538461537,0.953846153846152,
0.969230769230768,0.984615384615383,0.994228156739701),.UNSPECIFIED.)
CURVE()
GEOMETRIC_REPRESENTATION_ITEM()
RATIONAL_B_SPLINE_CURVE((1.,1.,1.,1.,1.,1.,1.,1.,1.,1.,1.,1.,1.,1.,1.,1.,
1.,1.,1.,1.,1.,1.,1.,1.,1.,1.,1.,1.,1.,1.,1.,1.,1.,1.,1.,1.,1.,1.,1.,1.,
1.,1.,1.,1.,1.,1.,1.,1.,1.,1.,1.,1.,1.,1.,1.,1.,1.,1.,1.,1.,1.,1.,1.,1.,
1.,1.,1.,1.,1.,1.))
REPRESENTATION_ITEM('')
);
#233=(
BOUNDED_CURVE()
B_SPLINE_CURVE(5,(#35721,#35722,#35723,#35724,#35725,#35726,#35727,#35728,
#35729,#35730,#35731,#35732,#35733,#35734,#35735,#35736,#35737,#35738,#35739,
#35740,#35741,#35742,#35743,#35744,#35745,#35746,#35747,#35748,#35749,#35750,
#35751,#35752,#35753,#35754,#35755,#35756,#35757,#35758,#35759,#35760,#35761,
#35762,#35763,#35764,#35765,#35766,#35767,#35768,#35769,#35770,#35771,#35772,
#35773,#35774,#35775,#35776,#35777,#35778,#35779,#35780,#35781,#35782,#35783,
#35784,#35785,#35786,#35787,#35788,#35789,#35790),.UNSPECIFIED.,.F.,.F.)
B_SPLINE_CURVE_WITH_KNOTS((6,1,1,1,1,1,1,1,1,1,1,1,1,1,1,1,1,1,1,1,1,1,
1,1,1,1,1,1,1,1,1,1,1,1,1,1,1,1,1,1,1,1,1,1,1,1,1,1,1,1,1,1,1,1,1,1,1,1,
1,1,1,1,1,1,1,6),(0.0057718433745091,0.0153846153846154,0.0307692307692308,
0.0461538461538462,0.0615384615384615,0.0769230769230769,0.0923076923076923,
0.107692307692308,0.123076923076923,0.138461538461538,0.153846153846154,
0.169230769230769,0.184615384615385,0.2,0.215384615384615,0.230769230769231,
0.246153846153846,0.261538461538462,0.276923076923077,0.292307692307692,
0.307692307692308,0.323076923076923,0.338461538461538,0.353846153846154,
0.369230769230769,0.384615384615385,0.4,0.415384615384615,0.430769230769231,
0.446153846153846,0.461538461538462,0.476923076923077,0.492307692307692,
0.507692307692308,0.523076923076923,0.538461538461538,0.553846153846154,
0.569230769230769,0.584615384615384,0.6,0.615384615384615,0.63076923076923,
0.646153846153846,0.661538461538461,0.676923076923076,0.692307692307692,
0.707692307692307,0.723076923076922,0.738461538461538,0.753846153846153,
0.769230769230768,0.784615384615384,0.799999999999999,0.815384615384614,
0.83076923076923,0.846153846153845,0.86153846153846,0.876923076923076,0.892307692307691,
0.907692307692306,0.923076923076922,0.938461538461537,0.953846153846152,
0.969230769230768,0.984615384615383,1.),.UNSPECIFIED.)
CURVE()
GEOMETRIC_REPRESENTATION_ITEM()
RATIONAL_B_SPLINE_CURVE((1.,1.,1.,1.,1.,1.,1.,1.,1.,1.,1.,1.,1.,1.,1.,1.,
1.,1.,1.,1.,1.,1.,1.,1.,1.,1.,1.,1.,1.,1.,1.,1.,1.,1.,1.,1.,1.,1.,1.,1.,
1.,1.,1.,1.,1.,1.,1.,1.,1.,1.,1.,1.,1.,1.,1.,1.,1.,1.,1.,1.,1.,1.,1.,1.,
1.,1.,1.,1.,1.,1.))
REPRESENTATION_ITEM('')
);
#234=(
BOUNDED_CURVE()
B_SPLINE_CURVE(5,(#35794,#35795,#35796,#35797,#35798,#35799,#35800,#35801,
#35802,#35803,#35804,#35805,#35806,#35807,#35808,#35809,#35810,#35811,#35812,
#35813,#35814,#35815,#35816,#35817,#35818,#35819,#35820,#35821,#35822,#35823,
#35824,#35825,#35826,#35827,#35828,#35829,#35830,#35831,#35832,#35833,#35834,
#35835,#35836,#35837,#35838,#35839,#35840,#35841,#35842,#35843,#35844,#35845,
#35846,#35847,#35848,#35849,#35850,#35851,#35852,#35853,#35854,#35855,#35856,
#35857,#35858,#35859,#35860,#35861,#35862,#35863),.UNSPECIFIED.,.F.,.F.)
B_SPLINE_CURVE_WITH_KNOTS((6,1,1,1,1,1,1,1,1,1,1,1,1,1,1,1,1,1,1,1,1,1,
1,1,1,1,1,1,1,1,1,1,1,1,1,1,1,1,1,1,1,1,1,1,1,1,1,1,1,1,1,1,1,1,1,1,1,1,
1,1,1,1,1,1,1,6),(0.,0.0153846153846154,0.0307692307692308,0.0461538461538462,
0.0615384615384615,0.0769230769230769,0.0923076923076923,0.107692307692308,
0.123076923076923,0.138461538461538,0.153846153846154,0.169230769230769,
0.184615384615385,0.2,0.215384615384615,0.230769230769231,0.246153846153846,
0.261538461538462,0.276923076923077,0.292307692307692,0.307692307692308,
0.323076923076923,0.338461538461538,0.353846153846154,0.369230769230769,
0.384615384615385,0.4,0.415384615384615,0.430769230769231,0.446153846153846,
0.461538461538462,0.476923076923077,0.492307692307692,0.507692307692308,
0.523076923076923,0.538461538461538,0.553846153846154,0.569230769230769,
0.584615384615384,0.6,0.615384615384615,0.63076923076923,0.646153846153846,
0.661538461538461,0.676923076923076,0.692307692307692,0.707692307692307,
0.723076923076922,0.738461538461538,0.753846153846153,0.769230769230768,
0.784615384615384,0.799999999999999,0.815384615384614,0.83076923076923,
0.846153846153845,0.86153846153846,0.876923076923076,0.892307692307691,
0.907692307692306,0.923076923076922,0.938461538461537,0.953846153846152,
0.969230769230768,0.984615384615383,0.994228156739689),.UNSPECIFIED.)
CURVE()
GEOMETRIC_REPRESENTATION_ITEM()
RATIONAL_B_SPLINE_CURVE((1.,1.,1.,1.,1.,1.,1.,1.,1.,1.,1.,1.,1.,1.,1.,1.,
1.,1.,1.,1.,1.,1.,1.,1.,1.,1.,1.,1.,1.,1.,1.,1.,1.,1.,1.,1.,1.,1.,1.,1.,
1.,1.,1.,1.,1.,1.,1.,1.,1.,1.,1.,1.,1.,1.,1.,1.,1.,1.,1.,1.,1.,1.,1.,1.,
1.,1.,1.,1.,1.,1.))
REPRESENTATION_ITEM('')
);
#235=(
BOUNDED_CURVE()
B_SPLINE_CURVE(5,(#35867,#35868,#35869,#35870,#35871,#35872,#35873,#35874,
#35875,#35876,#35877,#35878,#35879,#35880,#35881,#35882,#35883,#35884,#35885,
#35886,#35887,#35888,#35889,#35890,#35891,#35892,#35893,#35894,#35895,#35896,
#35897,#35898,#35899,#35900,#35901,#35902,#35903,#35904,#35905,#35906,#35907,
#35908,#35909,#35910,#35911,#35912,#35913,#35914,#35915,#35916,#35917,#35918,
#35919,#35920,#35921,#35922,#35923,#35924,#35925,#35926,#35927,#35928,#35929,
#35930,#35931,#35932,#35933,#35934,#35935,#35936),.UNSPECIFIED.,.F.,.F.)
B_SPLINE_CURVE_WITH_KNOTS((6,1,1,1,1,1,1,1,1,1,1,1,1,1,1,1,1,1,1,1,1,1,
1,1,1,1,1,1,1,1,1,1,1,1,1,1,1,1,1,1,1,1,1,1,1,1,1,1,1,1,1,1,1,1,1,1,1,1,
1,1,1,1,1,1,1,6),(0.00577184337450777,0.0153846153846154,0.0307692307692308,
0.0461538461538462,0.0615384615384615,0.0769230769230769,0.0923076923076923,
0.107692307692308,0.123076923076923,0.138461538461538,0.153846153846154,
0.169230769230769,0.184615384615385,0.2,0.215384615384615,0.230769230769231,
0.246153846153846,0.261538461538462,0.276923076923077,0.292307692307692,
0.307692307692308,0.323076923076923,0.338461538461538,0.353846153846154,
0.369230769230769,0.384615384615385,0.4,0.415384615384615,0.430769230769231,
0.446153846153846,0.461538461538462,0.476923076923077,0.492307692307692,
0.507692307692308,0.523076923076923,0.538461538461538,0.553846153846154,
0.569230769230769,0.584615384615384,0.6,0.615384615384615,0.63076923076923,
0.646153846153846,0.661538461538461,0.676923076923076,0.692307692307692,
0.707692307692307,0.723076923076922,0.738461538461538,0.753846153846153,
0.769230769230768,0.784615384615384,0.799999999999999,0.815384615384614,
0.83076923076923,0.846153846153845,0.86153846153846,0.876923076923076,0.892307692307691,
0.907692307692306,0.923076923076922,0.938461538461537,0.953846153846152,
0.969230769230768,0.984615384615383,1.),.UNSPECIFIED.)
CURVE()
GEOMETRIC_REPRESENTATION_ITEM()
RATIONAL_B_SPLINE_CURVE((1.,1.,1.,1.,1.,1.,1.,1.,1.,1.,1.,1.,1.,1.,1.,1.,
1.,1.,1.,1.,1.,1.,1.,1.,1.,1.,1.,1.,1.,1.,1.,1.,1.,1.,1.,1.,1.,1.,1.,1.,
1.,1.,1.,1.,1.,1.,1.,1.,1.,1.,1.,1.,1.,1.,1.,1.,1.,1.,1.,1.,1.,1.,1.,1.,
1.,1.,1.,1.,1.,1.))
REPRESENTATION_ITEM('')
);
#236=(
BOUNDED_CURVE()
B_SPLINE_CURVE(5,(#35940,#35941,#35942,#35943,#35944,#35945,#35946,#35947,
#35948,#35949,#35950,#35951,#35952,#35953,#35954,#35955,#35956,#35957,#35958,
#35959,#35960,#35961,#35962,#35963,#35964,#35965,#35966,#35967,#35968,#35969,
#35970,#35971,#35972,#35973,#35974,#35975,#35976,#35977,#35978,#35979,#35980,
#35981,#35982,#35983,#35984,#35985,#35986,#35987,#35988,#35989,#35990,#35991,
#35992,#35993,#35994,#35995,#35996,#35997,#35998,#35999,#36000,#36001,#36002,
#36003,#36004,#36005,#36006,#36007,#36008,#36009),.UNSPECIFIED.,.F.,.F.)
B_SPLINE_CURVE_WITH_KNOTS((6,1,1,1,1,1,1,1,1,1,1,1,1,1,1,1,1,1,1,1,1,1,
1,1,1,1,1,1,1,1,1,1,1,1,1,1,1,1,1,1,1,1,1,1,1,1,1,1,1,1,1,1,1,1,1,1,1,1,
1,1,1,1,1,1,1,6),(0.,0.0153846153846154,0.0307692307692308,0.0461538461538462,
0.0615384615384615,0.0769230769230769,0.0923076923076923,0.107692307692308,
0.123076923076923,0.138461538461538,0.153846153846154,0.169230769230769,
0.184615384615385,0.2,0.215384615384615,0.230769230769231,0.246153846153846,
0.261538461538462,0.276923076923077,0.292307692307692,0.307692307692308,
0.323076923076923,0.338461538461538,0.353846153846154,0.369230769230769,
0.384615384615385,0.4,0.415384615384615,0.430769230769231,0.446153846153846,
0.461538461538462,0.476923076923077,0.492307692307692,0.507692307692308,
0.523076923076923,0.538461538461538,0.553846153846154,0.569230769230769,
0.584615384615384,0.6,0.615384615384615,0.63076923076923,0.646153846153846,
0.661538461538461,0.676923076923076,0.692307692307692,0.707692307692307,
0.723076923076922,0.738461538461538,0.753846153846153,0.769230769230768,
0.784615384615384,0.799999999999999,0.815384615384614,0.83076923076923,
0.846153846153845,0.86153846153846,0.876923076923076,0.892307692307691,
0.907692307692306,0.923076923076922,0.938461538461537,0.953846153846152,
0.969230769230768,0.984615384615383,0.994228156739701),.UNSPECIFIED.)
CURVE()
GEOMETRIC_REPRESENTATION_ITEM()
RATIONAL_B_SPLINE_CURVE((1.,1.,1.,1.,1.,1.,1.,1.,1.,1.,1.,1.,1.,1.,1.,1.,
1.,1.,1.,1.,1.,1.,1.,1.,1.,1.,1.,1.,1.,1.,1.,1.,1.,1.,1.,1.,1.,1.,1.,1.,
1.,1.,1.,1.,1.,1.,1.,1.,1.,1.,1.,1.,1.,1.,1.,1.,1.,1.,1.,1.,1.,1.,1.,1.,
1.,1.,1.,1.,1.,1.))
REPRESENTATION_ITEM('')
);
#237=(
BOUNDED_CURVE()
B_SPLINE_CURVE(5,(#36013,#36014,#36015,#36016,#36017,#36018,#36019,#36020,
#36021,#36022,#36023,#36024,#36025,#36026,#36027,#36028,#36029,#36030,#36031,
#36032,#36033,#36034,#36035,#36036,#36037,#36038,#36039,#36040,#36041,#36042,
#36043,#36044,#36045,#36046,#36047,#36048,#36049,#36050,#36051,#36052,#36053,
#36054,#36055,#36056,#36057,#36058,#36059,#36060,#36061,#36062,#36063,#36064,
#36065,#36066,#36067,#36068,#36069,#36070,#36071,#36072,#36073,#36074,#36075,
#36076,#36077,#36078,#36079,#36080,#36081,#36082),.UNSPECIFIED.,.F.,.F.)
B_SPLINE_CURVE_WITH_KNOTS((6,1,1,1,1,1,1,1,1,1,1,1,1,1,1,1,1,1,1,1,1,1,
1,1,1,1,1,1,1,1,1,1,1,1,1,1,1,1,1,1,1,1,1,1,1,1,1,1,1,1,1,1,1,1,1,1,1,1,
1,1,1,1,1,1,1,6),(0.00577184337450172,0.0153846153846154,0.0307692307692308,
0.0461538461538462,0.0615384615384615,0.0769230769230769,0.0923076923076923,
0.107692307692308,0.123076923076923,0.138461538461538,0.153846153846154,
0.169230769230769,0.184615384615385,0.2,0.215384615384615,0.230769230769231,
0.246153846153846,0.261538461538462,0.276923076923077,0.292307692307692,
0.307692307692308,0.323076923076923,0.338461538461538,0.353846153846154,
0.369230769230769,0.384615384615385,0.4,0.415384615384615,0.430769230769231,
0.446153846153846,0.461538461538462,0.476923076923077,0.492307692307692,
0.507692307692308,0.523076923076923,0.538461538461538,0.553846153846154,
0.569230769230769,0.584615384615384,0.6,0.615384615384615,0.63076923076923,
0.646153846153846,0.661538461538461,0.676923076923076,0.692307692307692,
0.707692307692307,0.723076923076922,0.738461538461538,0.753846153846153,
0.769230769230768,0.784615384615384,0.799999999999999,0.815384615384614,
0.83076923076923,0.846153846153845,0.86153846153846,0.876923076923076,0.892307692307691,
0.907692307692306,0.923076923076922,0.938461538461537,0.953846153846152,
0.969230769230768,0.984615384615383,1.),.UNSPECIFIED.)
CURVE()
GEOMETRIC_REPRESENTATION_ITEM()
RATIONAL_B_SPLINE_CURVE((1.,1.,1.,1.,1.,1.,1.,1.,1.,1.,1.,1.,1.,1.,1.,1.,
1.,1.,1.,1.,1.,1.,1.,1.,1.,1.,1.,1.,1.,1.,1.,1.,1.,1.,1.,1.,1.,1.,1.,1.,
1.,1.,1.,1.,1.,1.,1.,1.,1.,1.,1.,1.,1.,1.,1.,1.,1.,1.,1.,1.,1.,1.,1.,1.,
1.,1.,1.,1.,1.,1.))
REPRESENTATION_ITEM('')
);
#238=(
BOUNDED_CURVE()
B_SPLINE_CURVE(5,(#36086,#36087,#36088,#36089,#36090,#36091,#36092,#36093,
#36094,#36095,#36096,#36097,#36098,#36099,#36100,#36101,#36102,#36103,#36104,
#36105,#36106,#36107,#36108,#36109,#36110,#36111,#36112,#36113,#36114,#36115,
#36116,#36117,#36118,#36119,#36120,#36121,#36122,#36123,#36124,#36125,#36126,
#36127,#36128,#36129,#36130,#36131,#36132,#36133,#36134,#36135,#36136,#36137,
#36138,#36139,#36140,#36141,#36142,#36143,#36144,#36145,#36146,#36147,#36148,
#36149,#36150,#36151,#36152,#36153,#36154,#36155),.UNSPECIFIED.,.F.,.F.)
B_SPLINE_CURVE_WITH_KNOTS((6,1,1,1,1,1,1,1,1,1,1,1,1,1,1,1,1,1,1,1,1,1,
1,1,1,1,1,1,1,1,1,1,1,1,1,1,1,1,1,1,1,1,1,1,1,1,1,1,1,1,1,1,1,1,1,1,1,1,
1,1,1,1,1,1,1,6),(0.,0.0153846153846154,0.0307692307692308,0.0461538461538462,
0.0615384615384615,0.0769230769230769,0.0923076923076923,0.107692307692308,
0.123076923076923,0.138461538461538,0.153846153846154,0.169230769230769,
0.184615384615385,0.2,0.215384615384615,0.230769230769231,0.246153846153846,
0.261538461538462,0.276923076923077,0.292307692307692,0.307692307692308,
0.323076923076923,0.338461538461538,0.353846153846154,0.369230769230769,
0.384615384615385,0.4,0.415384615384615,0.430769230769231,0.446153846153846,
0.461538461538462,0.476923076923077,0.492307692307692,0.507692307692308,
0.523076923076923,0.538461538461538,0.553846153846154,0.569230769230769,
0.584615384615384,0.6,0.615384615384615,0.63076923076923,0.646153846153846,
0.661538461538461,0.676923076923076,0.692307692307692,0.707692307692307,
0.723076923076922,0.738461538461538,0.753846153846153,0.769230769230768,
0.784615384615384,0.799999999999999,0.815384615384614,0.83076923076923,
0.846153846153845,0.86153846153846,0.876923076923076,0.892307692307691,
0.907692307692306,0.923076923076922,0.938461538461537,0.953846153846152,
0.969230769230768,0.984615384615383,0.99422815673971),.UNSPECIFIED.)
CURVE()
GEOMETRIC_REPRESENTATION_ITEM()
RATIONAL_B_SPLINE_CURVE((1.,1.,1.,1.,1.,1.,1.,1.,1.,1.,1.,1.,1.,1.,1.,1.,
1.,1.,1.,1.,1.,1.,1.,1.,1.,1.,1.,1.,1.,1.,1.,1.,1.,1.,1.,1.,1.,1.,1.,1.,
1.,1.,1.,1.,1.,1.,1.,1.,1.,1.,1.,1.,1.,1.,1.,1.,1.,1.,1.,1.,1.,1.,1.,1.,
1.,1.,1.,1.,1.,1.))
REPRESENTATION_ITEM('')
);
#239=(
BOUNDED_CURVE()
B_SPLINE_CURVE(5,(#36159,#36160,#36161,#36162,#36163,#36164,#36165,#36166,
#36167,#36168,#36169,#36170,#36171,#36172,#36173,#36174,#36175,#36176,#36177,
#36178,#36179,#36180,#36181,#36182,#36183,#36184,#36185,#36186,#36187,#36188,
#36189,#36190,#36191,#36192,#36193,#36194,#36195,#36196,#36197,#36198,#36199,
#36200,#36201,#36202,#36203,#36204,#36205,#36206,#36207,#36208,#36209,#36210,
#36211,#36212,#36213,#36214,#36215,#36216,#36217,#36218,#36219,#36220,#36221,
#36222,#36223,#36224,#36225,#36226,#36227,#36228),.UNSPECIFIED.,.F.,.F.)
B_SPLINE_CURVE_WITH_KNOTS((6,1,1,1,1,1,1,1,1,1,1,1,1,1,1,1,1,1,1,1,1,1,
1,1,1,1,1,1,1,1,1,1,1,1,1,1,1,1,1,1,1,1,1,1,1,1,1,1,1,1,1,1,1,1,1,1,1,1,
1,1,1,1,1,1,1,6),(0.00577184337448657,0.0153846153846154,0.0307692307692308,
0.0461538461538462,0.0615384615384615,0.0769230769230769,0.0923076923076923,
0.107692307692308,0.123076923076923,0.138461538461538,0.153846153846154,
0.169230769230769,0.184615384615385,0.2,0.215384615384615,0.230769230769231,
0.246153846153846,0.261538461538462,0.276923076923077,0.292307692307692,
0.307692307692308,0.323076923076923,0.338461538461538,0.353846153846154,
0.369230769230769,0.384615384615385,0.4,0.415384615384615,0.430769230769231,
0.446153846153846,0.461538461538462,0.476923076923077,0.492307692307692,
0.507692307692308,0.523076923076923,0.538461538461538,0.553846153846154,
0.569230769230769,0.584615384615384,0.6,0.615384615384615,0.63076923076923,
0.646153846153846,0.661538461538461,0.676923076923076,0.692307692307692,
0.707692307692307,0.723076923076922,0.738461538461538,0.753846153846153,
0.769230769230768,0.784615384615384,0.799999999999999,0.815384615384614,
0.83076923076923,0.846153846153845,0.86153846153846,0.876923076923076,0.892307692307691,
0.907692307692306,0.923076923076922,0.938461538461537,0.953846153846152,
0.969230769230768,0.984615384615383,1.),.UNSPECIFIED.)
CURVE()
GEOMETRIC_REPRESENTATION_ITEM()
RATIONAL_B_SPLINE_CURVE((1.,1.,1.,1.,1.,1.,1.,1.,1.,1.,1.,1.,1.,1.,1.,1.,
1.,1.,1.,1.,1.,1.,1.,1.,1.,1.,1.,1.,1.,1.,1.,1.,1.,1.,1.,1.,1.,1.,1.,1.,
1.,1.,1.,1.,1.,1.,1.,1.,1.,1.,1.,1.,1.,1.,1.,1.,1.,1.,1.,1.,1.,1.,1.,1.,
1.,1.,1.,1.,1.,1.))
REPRESENTATION_ITEM('')
);
#240=(
BOUNDED_CURVE()
B_SPLINE_CURVE(5,(#36232,#36233,#36234,#36235,#36236,#36237,#36238,#36239,
#36240,#36241,#36242,#36243,#36244,#36245,#36246,#36247,#36248,#36249,#36250,
#36251,#36252,#36253,#36254,#36255,#36256,#36257,#36258,#36259,#36260,#36261,
#36262,#36263,#36264,#36265,#36266,#36267,#36268,#36269,#36270,#36271,#36272,
#36273,#36274,#36275,#36276,#36277,#36278,#36279,#36280,#36281,#36282,#36283,
#36284,#36285,#36286,#36287,#36288,#36289,#36290,#36291,#36292,#36293,#36294,
#36295,#36296,#36297,#36298,#36299,#36300,#36301),.UNSPECIFIED.,.F.,.F.)
B_SPLINE_CURVE_WITH_KNOTS((6,1,1,1,1,1,1,1,1,1,1,1,1,1,1,1,1,1,1,1,1,1,
1,1,1,1,1,1,1,1,1,1,1,1,1,1,1,1,1,1,1,1,1,1,1,1,1,1,1,1,1,1,1,1,1,1,1,1,
1,1,1,1,1,1,1,6),(0.,0.0153846153846154,0.0307692307692308,0.0461538461538462,
0.0615384615384615,0.0769230769230769,0.0923076923076923,0.107692307692308,
0.123076923076923,0.138461538461538,0.153846153846154,0.169230769230769,
0.184615384615385,0.2,0.215384615384615,0.230769230769231,0.246153846153846,
0.261538461538462,0.276923076923077,0.292307692307692,0.307692307692308,
0.323076923076923,0.338461538461538,0.353846153846154,0.369230769230769,
0.384615384615385,0.4,0.415384615384615,0.430769230769231,0.446153846153846,
0.461538461538462,0.476923076923077,0.492307692307692,0.507692307692308,
0.523076923076923,0.538461538461538,0.553846153846154,0.569230769230769,
0.584615384615384,0.6,0.615384615384615,0.63076923076923,0.646153846153846,
0.661538461538461,0.676923076923076,0.692307692307692,0.707692307692307,
0.723076923076922,0.738461538461538,0.753846153846153,0.769230769230768,
0.784615384615384,0.799999999999999,0.815384615384614,0.83076923076923,
0.846153846153845,0.86153846153846,0.876923076923076,0.892307692307691,
0.907692307692306,0.923076923076922,0.938461538461537,0.953846153846152,
0.969230769230768,0.984615384615383,0.994228156739709),.UNSPECIFIED.)
CURVE()
GEOMETRIC_REPRESENTATION_ITEM()
RATIONAL_B_SPLINE_CURVE((1.,1.,1.,1.,1.,1.,1.,1.,1.,1.,1.,1.,1.,1.,1.,1.,
1.,1.,1.,1.,1.,1.,1.,1.,1.,1.,1.,1.,1.,1.,1.,1.,1.,1.,1.,1.,1.,1.,1.,1.,
1.,1.,1.,1.,1.,1.,1.,1.,1.,1.,1.,1.,1.,1.,1.,1.,1.,1.,1.,1.,1.,1.,1.,1.,
1.,1.,1.,1.,1.,1.))
REPRESENTATION_ITEM('')
);
#241=(
BOUNDED_CURVE()
B_SPLINE_CURVE(5,(#36305,#36306,#36307,#36308,#36309,#36310,#36311,#36312,
#36313,#36314,#36315,#36316,#36317,#36318,#36319,#36320,#36321,#36322,#36323,
#36324,#36325,#36326,#36327,#36328,#36329,#36330,#36331,#36332,#36333,#36334,
#36335,#36336,#36337,#36338,#36339,#36340,#36341,#36342,#36343,#36344,#36345,
#36346,#36347,#36348,#36349,#36350,#36351,#36352,#36353,#36354,#36355,#36356,
#36357,#36358,#36359,#36360,#36361,#36362,#36363,#36364,#36365,#36366,#36367,
#36368,#36369,#36370,#36371,#36372,#36373,#36374),.UNSPECIFIED.,.F.,.F.)
B_SPLINE_CURVE_WITH_KNOTS((6,1,1,1,1,1,1,1,1,1,1,1,1,1,1,1,1,1,1,1,1,1,
1,1,1,1,1,1,1,1,1,1,1,1,1,1,1,1,1,1,1,1,1,1,1,1,1,1,1,1,1,1,1,1,1,1,1,1,
1,1,1,1,1,1,1,6),(0.00577184337451094,0.0153846153846154,0.0307692307692308,
0.0461538461538462,0.0615384615384615,0.0769230769230769,0.0923076923076923,
0.107692307692308,0.123076923076923,0.138461538461538,0.153846153846154,
0.169230769230769,0.184615384615385,0.2,0.215384615384615,0.230769230769231,
0.246153846153846,0.261538461538462,0.276923076923077,0.292307692307692,
0.307692307692308,0.323076923076923,0.338461538461538,0.353846153846154,
0.369230769230769,0.384615384615385,0.4,0.415384615384615,0.430769230769231,
0.446153846153846,0.461538461538462,0.476923076923077,0.492307692307692,
0.507692307692308,0.523076923076923,0.538461538461538,0.553846153846154,
0.569230769230769,0.584615384615384,0.6,0.615384615384615,0.63076923076923,
0.646153846153846,0.661538461538461,0.676923076923076,0.692307692307692,
0.707692307692307,0.723076923076922,0.738461538461538,0.753846153846153,
0.769230769230768,0.784615384615384,0.799999999999999,0.815384615384614,
0.83076923076923,0.846153846153845,0.86153846153846,0.876923076923076,0.892307692307691,
0.907692307692306,0.923076923076922,0.938461538461537,0.953846153846152,
0.969230769230768,0.984615384615383,1.),.UNSPECIFIED.)
CURVE()
GEOMETRIC_REPRESENTATION_ITEM()
RATIONAL_B_SPLINE_CURVE((1.,1.,1.,1.,1.,1.,1.,1.,1.,1.,1.,1.,1.,1.,1.,1.,
1.,1.,1.,1.,1.,1.,1.,1.,1.,1.,1.,1.,1.,1.,1.,1.,1.,1.,1.,1.,1.,1.,1.,1.,
1.,1.,1.,1.,1.,1.,1.,1.,1.,1.,1.,1.,1.,1.,1.,1.,1.,1.,1.,1.,1.,1.,1.,1.,
1.,1.,1.,1.,1.,1.))
REPRESENTATION_ITEM('')
);
#242=(
BOUNDED_CURVE()
B_SPLINE_CURVE(5,(#36378,#36379,#36380,#36381,#36382,#36383,#36384,#36385,
#36386,#36387,#36388,#36389,#36390,#36391,#36392,#36393,#36394,#36395,#36396,
#36397,#36398,#36399,#36400,#36401,#36402,#36403,#36404,#36405,#36406,#36407,
#36408,#36409,#36410,#36411,#36412,#36413,#36414,#36415,#36416,#36417,#36418,
#36419,#36420,#36421,#36422,#36423,#36424,#36425,#36426,#36427,#36428,#36429,
#36430,#36431,#36432,#36433,#36434,#36435,#36436,#36437,#36438,#36439,#36440,
#36441,#36442,#36443,#36444,#36445,#36446,#36447),.UNSPECIFIED.,.F.,.F.)
B_SPLINE_CURVE_WITH_KNOTS((6,1,1,1,1,1,1,1,1,1,1,1,1,1,1,1,1,1,1,1,1,1,
1,1,1,1,1,1,1,1,1,1,1,1,1,1,1,1,1,1,1,1,1,1,1,1,1,1,1,1,1,1,1,1,1,1,1,1,
1,1,1,1,1,1,1,6),(0.,0.0153846153846154,0.0307692307692308,0.0461538461538462,
0.0615384615384615,0.0769230769230769,0.0923076923076923,0.107692307692308,
0.123076923076923,0.138461538461538,0.153846153846154,0.169230769230769,
0.184615384615385,0.2,0.215384615384615,0.230769230769231,0.246153846153846,
0.261538461538462,0.276923076923077,0.292307692307692,0.307692307692308,
0.323076923076923,0.338461538461538,0.353846153846154,0.369230769230769,
0.384615384615385,0.4,0.415384615384615,0.430769230769231,0.446153846153846,
0.461538461538462,0.476923076923077,0.492307692307692,0.507692307692308,
0.523076923076923,0.538461538461538,0.553846153846154,0.569230769230769,
0.584615384615384,0.6,0.615384615384615,0.63076923076923,0.646153846153846,
0.661538461538461,0.676923076923076,0.692307692307692,0.707692307692307,
0.723076923076922,0.738461538461538,0.753846153846153,0.769230769230768,
0.784615384615384,0.799999999999999,0.815384615384614,0.83076923076923,
0.846153846153845,0.86153846153846,0.876923076923076,0.892307692307691,
0.907692307692306,0.923076923076922,0.938461538461537,0.953846153846152,
0.969230769230768,0.984615384615383,0.994228156739701),.UNSPECIFIED.)
CURVE()
GEOMETRIC_REPRESENTATION_ITEM()
RATIONAL_B_SPLINE_CURVE((1.,1.,1.,1.,1.,1.,1.,1.,1.,1.,1.,1.,1.,1.,1.,1.,
1.,1.,1.,1.,1.,1.,1.,1.,1.,1.,1.,1.,1.,1.,1.,1.,1.,1.,1.,1.,1.,1.,1.,1.,
1.,1.,1.,1.,1.,1.,1.,1.,1.,1.,1.,1.,1.,1.,1.,1.,1.,1.,1.,1.,1.,1.,1.,1.,
1.,1.,1.,1.,1.,1.))
REPRESENTATION_ITEM('')
);
#243=(
BOUNDED_CURVE()
B_SPLINE_CURVE(5,(#36451,#36452,#36453,#36454,#36455,#36456,#36457,#36458,
#36459,#36460,#36461,#36462,#36463,#36464,#36465,#36466,#36467,#36468,#36469,
#36470,#36471,#36472,#36473,#36474,#36475,#36476,#36477,#36478,#36479,#36480,
#36481,#36482,#36483,#36484,#36485,#36486,#36487,#36488,#36489,#36490,#36491,
#36492,#36493,#36494,#36495,#36496,#36497,#36498,#36499,#36500,#36501,#36502,
#36503,#36504,#36505,#36506,#36507,#36508,#36509,#36510,#36511,#36512,#36513,
#36514,#36515,#36516,#36517,#36518,#36519,#36520),.UNSPECIFIED.,.F.,.F.)
B_SPLINE_CURVE_WITH_KNOTS((6,1,1,1,1,1,1,1,1,1,1,1,1,1,1,1,1,1,1,1,1,1,
1,1,1,1,1,1,1,1,1,1,1,1,1,1,1,1,1,1,1,1,1,1,1,1,1,1,1,1,1,1,1,1,1,1,1,1,
1,1,1,1,1,1,1,6),(0.0057718433745102,0.0153846153846154,0.0307692307692308,
0.0461538461538462,0.0615384615384615,0.0769230769230769,0.0923076923076923,
0.107692307692308,0.123076923076923,0.138461538461538,0.153846153846154,
0.169230769230769,0.184615384615385,0.2,0.215384615384615,0.230769230769231,
0.246153846153846,0.261538461538462,0.276923076923077,0.292307692307692,
0.307692307692308,0.323076923076923,0.338461538461538,0.353846153846154,
0.369230769230769,0.384615384615385,0.4,0.415384615384615,0.430769230769231,
0.446153846153846,0.461538461538462,0.476923076923077,0.492307692307692,
0.507692307692308,0.523076923076923,0.538461538461538,0.553846153846154,
0.569230769230769,0.584615384615384,0.6,0.615384615384615,0.63076923076923,
0.646153846153846,0.661538461538461,0.676923076923076,0.692307692307692,
0.707692307692307,0.723076923076922,0.738461538461538,0.753846153846153,
0.769230769230768,0.784615384615384,0.799999999999999,0.815384615384614,
0.83076923076923,0.846153846153845,0.86153846153846,0.876923076923076,0.892307692307691,
0.907692307692306,0.923076923076922,0.938461538461537,0.953846153846152,
0.969230769230768,0.984615384615383,1.),.UNSPECIFIED.)
CURVE()
GEOMETRIC_REPRESENTATION_ITEM()
RATIONAL_B_SPLINE_CURVE((1.,1.,1.,1.,1.,1.,1.,1.,1.,1.,1.,1.,1.,1.,1.,1.,
1.,1.,1.,1.,1.,1.,1.,1.,1.,1.,1.,1.,1.,1.,1.,1.,1.,1.,1.,1.,1.,1.,1.,1.,
1.,1.,1.,1.,1.,1.,1.,1.,1.,1.,1.,1.,1.,1.,1.,1.,1.,1.,1.,1.,1.,1.,1.,1.,
1.,1.,1.,1.,1.,1.))
REPRESENTATION_ITEM('')
);
#244=(
BOUNDED_CURVE()
B_SPLINE_CURVE(5,(#36524,#36525,#36526,#36527,#36528,#36529,#36530,#36531,
#36532,#36533,#36534,#36535,#36536,#36537,#36538,#36539,#36540,#36541,#36542,
#36543,#36544,#36545,#36546,#36547,#36548,#36549,#36550,#36551,#36552,#36553,
#36554,#36555,#36556,#36557,#36558,#36559,#36560,#36561,#36562,#36563,#36564,
#36565,#36566,#36567,#36568,#36569,#36570,#36571,#36572,#36573,#36574,#36575,
#36576,#36577,#36578,#36579,#36580,#36581,#36582,#36583,#36584,#36585,#36586,
#36587,#36588,#36589,#36590,#36591,#36592,#36593),.UNSPECIFIED.,.F.,.F.)
B_SPLINE_CURVE_WITH_KNOTS((6,1,1,1,1,1,1,1,1,1,1,1,1,1,1,1,1,1,1,1,1,1,
1,1,1,1,1,1,1,1,1,1,1,1,1,1,1,1,1,1,1,1,1,1,1,1,1,1,1,1,1,1,1,1,1,1,1,1,
1,1,1,1,1,1,1,6),(0.,0.0153846153846154,0.0307692307692308,0.0461538461538462,
0.0615384615384615,0.0769230769230769,0.0923076923076923,0.107692307692308,
0.123076923076923,0.138461538461538,0.153846153846154,0.169230769230769,
0.184615384615385,0.2,0.215384615384615,0.230769230769231,0.246153846153846,
0.261538461538462,0.276923076923077,0.292307692307692,0.307692307692308,
0.323076923076923,0.338461538461538,0.353846153846154,0.369230769230769,
0.384615384615385,0.4,0.415384615384615,0.430769230769231,0.446153846153846,
0.461538461538462,0.476923076923077,0.492307692307692,0.507692307692308,
0.523076923076923,0.538461538461538,0.553846153846154,0.569230769230769,
0.584615384615384,0.6,0.615384615384615,0.63076923076923,0.646153846153846,
0.661538461538461,0.676923076923076,0.692307692307692,0.707692307692307,
0.723076923076922,0.738461538461538,0.753846153846153,0.769230769230768,
0.784615384615384,0.799999999999999,0.815384615384614,0.83076923076923,
0.846153846153845,0.86153846153846,0.876923076923076,0.892307692307691,
0.907692307692306,0.923076923076922,0.938461538461537,0.953846153846152,
0.969230769230768,0.984615384615383,0.994228156739694),.UNSPECIFIED.)
CURVE()
GEOMETRIC_REPRESENTATION_ITEM()
RATIONAL_B_SPLINE_CURVE((1.,1.,1.,1.,1.,1.,1.,1.,1.,1.,1.,1.,1.,1.,1.,1.,
1.,1.,1.,1.,1.,1.,1.,1.,1.,1.,1.,1.,1.,1.,1.,1.,1.,1.,1.,1.,1.,1.,1.,1.,
1.,1.,1.,1.,1.,1.,1.,1.,1.,1.,1.,1.,1.,1.,1.,1.,1.,1.,1.,1.,1.,1.,1.,1.,
1.,1.,1.,1.,1.,1.))
REPRESENTATION_ITEM('')
);
#245=(
BOUNDED_CURVE()
B_SPLINE_CURVE(5,(#36597,#36598,#36599,#36600,#36601,#36602,#36603,#36604,
#36605,#36606,#36607,#36608,#36609,#36610,#36611,#36612,#36613,#36614,#36615,
#36616,#36617,#36618,#36619,#36620,#36621,#36622,#36623,#36624,#36625,#36626,
#36627,#36628,#36629,#36630,#36631,#36632,#36633,#36634,#36635,#36636,#36637,
#36638,#36639,#36640,#36641,#36642,#36643,#36644,#36645,#36646,#36647,#36648,
#36649,#36650,#36651,#36652,#36653,#36654,#36655,#36656,#36657,#36658,#36659,
#36660,#36661,#36662,#36663,#36664,#36665,#36666),.UNSPECIFIED.,.F.,.F.)
B_SPLINE_CURVE_WITH_KNOTS((6,1,1,1,1,1,1,1,1,1,1,1,1,1,1,1,1,1,1,1,1,1,
1,1,1,1,1,1,1,1,1,1,1,1,1,1,1,1,1,1,1,1,1,1,1,1,1,1,1,1,1,1,1,1,1,1,1,1,
1,1,1,1,1,1,1,6),(0.00577184337452044,0.0153846153846154,0.0307692307692308,
0.0461538461538462,0.0615384615384615,0.0769230769230769,0.0923076923076923,
0.107692307692308,0.123076923076923,0.138461538461538,0.153846153846154,
0.169230769230769,0.184615384615385,0.2,0.215384615384615,0.230769230769231,
0.246153846153846,0.261538461538462,0.276923076923077,0.292307692307692,
0.307692307692308,0.323076923076923,0.338461538461538,0.353846153846154,
0.369230769230769,0.384615384615385,0.4,0.415384615384615,0.430769230769231,
0.446153846153846,0.461538461538462,0.476923076923077,0.492307692307692,
0.507692307692308,0.523076923076923,0.538461538461538,0.553846153846154,
0.569230769230769,0.584615384615384,0.6,0.615384615384615,0.63076923076923,
0.646153846153846,0.661538461538461,0.676923076923076,0.692307692307692,
0.707692307692307,0.723076923076922,0.738461538461538,0.753846153846153,
0.769230769230768,0.784615384615384,0.799999999999999,0.815384615384614,
0.83076923076923,0.846153846153845,0.86153846153846,0.876923076923076,0.892307692307691,
0.907692307692306,0.923076923076922,0.938461538461537,0.953846153846152,
0.969230769230768,0.984615384615383,1.),.UNSPECIFIED.)
CURVE()
GEOMETRIC_REPRESENTATION_ITEM()
RATIONAL_B_SPLINE_CURVE((1.,1.,1.,1.,1.,1.,1.,1.,1.,1.,1.,1.,1.,1.,1.,1.,
1.,1.,1.,1.,1.,1.,1.,1.,1.,1.,1.,1.,1.,1.,1.,1.,1.,1.,1.,1.,1.,1.,1.,1.,
1.,1.,1.,1.,1.,1.,1.,1.,1.,1.,1.,1.,1.,1.,1.,1.,1.,1.,1.,1.,1.,1.,1.,1.,
1.,1.,1.,1.,1.,1.))
REPRESENTATION_ITEM('')
);
#246=(
BOUNDED_CURVE()
B_SPLINE_CURVE(5,(#36670,#36671,#36672,#36673,#36674,#36675,#36676,#36677,
#36678,#36679,#36680,#36681,#36682,#36683,#36684,#36685,#36686,#36687,#36688,
#36689,#36690,#36691,#36692,#36693,#36694,#36695,#36696,#36697,#36698,#36699,
#36700,#36701,#36702,#36703,#36704,#36705,#36706,#36707,#36708,#36709,#36710,
#36711,#36712,#36713,#36714,#36715,#36716,#36717,#36718,#36719,#36720,#36721,
#36722,#36723,#36724,#36725,#36726,#36727,#36728,#36729,#36730,#36731,#36732,
#36733,#36734,#36735,#36736,#36737,#36738,#36739),.UNSPECIFIED.,.F.,.F.)
B_SPLINE_CURVE_WITH_KNOTS((6,1,1,1,1,1,1,1,1,1,1,1,1,1,1,1,1,1,1,1,1,1,
1,1,1,1,1,1,1,1,1,1,1,1,1,1,1,1,1,1,1,1,1,1,1,1,1,1,1,1,1,1,1,1,1,1,1,1,
1,1,1,1,1,1,1,6),(0.,0.0153846153846154,0.0307692307692308,0.0461538461538462,
0.0615384615384615,0.0769230769230769,0.0923076923076923,0.107692307692308,
0.123076923076923,0.138461538461538,0.153846153846154,0.169230769230769,
0.184615384615385,0.2,0.215384615384615,0.230769230769231,0.246153846153846,
0.261538461538462,0.276923076923077,0.292307692307692,0.307692307692308,
0.323076923076923,0.338461538461538,0.353846153846154,0.369230769230769,
0.384615384615385,0.4,0.415384615384615,0.430769230769231,0.446153846153846,
0.461538461538462,0.476923076923077,0.492307692307692,0.507692307692308,
0.523076923076923,0.538461538461538,0.553846153846154,0.569230769230769,
0.584615384615384,0.6,0.615384615384615,0.63076923076923,0.646153846153846,
0.661538461538461,0.676923076923076,0.692307692307692,0.707692307692307,
0.723076923076922,0.738461538461538,0.753846153846153,0.769230769230768,
0.784615384615384,0.799999999999999,0.815384615384614,0.83076923076923,
0.846153846153845,0.86153846153846,0.876923076923076,0.892307692307691,
0.907692307692306,0.923076923076922,0.938461538461537,0.953846153846152,
0.969230769230768,0.984615384615383,0.994228156739698),.UNSPECIFIED.)
CURVE()
GEOMETRIC_REPRESENTATION_ITEM()
RATIONAL_B_SPLINE_CURVE((1.,1.,1.,1.,1.,1.,1.,1.,1.,1.,1.,1.,1.,1.,1.,1.,
1.,1.,1.,1.,1.,1.,1.,1.,1.,1.,1.,1.,1.,1.,1.,1.,1.,1.,1.,1.,1.,1.,1.,1.,
1.,1.,1.,1.,1.,1.,1.,1.,1.,1.,1.,1.,1.,1.,1.,1.,1.,1.,1.,1.,1.,1.,1.,1.,
1.,1.,1.,1.,1.,1.))
REPRESENTATION_ITEM('')
);
#247=(
BOUNDED_CURVE()
B_SPLINE_CURVE(5,(#36743,#36744,#36745,#36746,#36747,#36748,#36749,#36750,
#36751,#36752,#36753,#36754,#36755,#36756,#36757,#36758,#36759,#36760,#36761,
#36762,#36763,#36764,#36765,#36766,#36767,#36768,#36769,#36770,#36771,#36772,
#36773,#36774,#36775,#36776,#36777,#36778,#36779,#36780,#36781,#36782,#36783,
#36784,#36785,#36786,#36787,#36788,#36789,#36790,#36791,#36792,#36793,#36794,
#36795,#36796,#36797,#36798,#36799,#36800,#36801,#36802,#36803,#36804,#36805,
#36806,#36807,#36808,#36809,#36810,#36811,#36812),.UNSPECIFIED.,.F.,.F.)
B_SPLINE_CURVE_WITH_KNOTS((6,1,1,1,1,1,1,1,1,1,1,1,1,1,1,1,1,1,1,1,1,1,
1,1,1,1,1,1,1,1,1,1,1,1,1,1,1,1,1,1,1,1,1,1,1,1,1,1,1,1,1,1,1,1,1,1,1,1,
1,1,1,1,1,1,1,6),(0.00577184337451607,0.0153846153846154,0.0307692307692308,
0.0461538461538462,0.0615384615384615,0.0769230769230769,0.0923076923076923,
0.107692307692308,0.123076923076923,0.138461538461538,0.153846153846154,
0.169230769230769,0.184615384615385,0.2,0.215384615384615,0.230769230769231,
0.246153846153846,0.261538461538462,0.276923076923077,0.292307692307692,
0.307692307692308,0.323076923076923,0.338461538461538,0.353846153846154,
0.369230769230769,0.384615384615385,0.4,0.415384615384615,0.430769230769231,
0.446153846153846,0.461538461538462,0.476923076923077,0.492307692307692,
0.507692307692308,0.523076923076923,0.538461538461538,0.553846153846154,
0.569230769230769,0.584615384615384,0.6,0.615384615384615,0.63076923076923,
0.646153846153846,0.661538461538461,0.676923076923076,0.692307692307692,
0.707692307692307,0.723076923076922,0.738461538461538,0.753846153846153,
0.769230769230768,0.784615384615384,0.799999999999999,0.815384615384614,
0.83076923076923,0.846153846153845,0.86153846153846,0.876923076923076,0.892307692307691,
0.907692307692306,0.923076923076922,0.938461538461537,0.953846153846152,
0.969230769230768,0.984615384615383,1.),.UNSPECIFIED.)
CURVE()
GEOMETRIC_REPRESENTATION_ITEM()
RATIONAL_B_SPLINE_CURVE((1.,1.,1.,1.,1.,1.,1.,1.,1.,1.,1.,1.,1.,1.,1.,1.,
1.,1.,1.,1.,1.,1.,1.,1.,1.,1.,1.,1.,1.,1.,1.,1.,1.,1.,1.,1.,1.,1.,1.,1.,
1.,1.,1.,1.,1.,1.,1.,1.,1.,1.,1.,1.,1.,1.,1.,1.,1.,1.,1.,1.,1.,1.,1.,1.,
1.,1.,1.,1.,1.,1.))
REPRESENTATION_ITEM('')
);
#248=(
BOUNDED_CURVE()
B_SPLINE_CURVE(5,(#36816,#36817,#36818,#36819,#36820,#36821,#36822,#36823,
#36824,#36825,#36826,#36827,#36828,#36829,#36830,#36831,#36832,#36833,#36834,
#36835,#36836,#36837,#36838,#36839,#36840,#36841,#36842,#36843,#36844,#36845,
#36846,#36847,#36848,#36849,#36850,#36851,#36852,#36853,#36854,#36855,#36856,
#36857,#36858,#36859,#36860,#36861,#36862,#36863,#36864,#36865,#36866,#36867,
#36868,#36869,#36870,#36871,#36872,#36873,#36874,#36875,#36876,#36877,#36878,
#36879,#36880,#36881,#36882,#36883,#36884,#36885),.UNSPECIFIED.,.F.,.F.)
B_SPLINE_CURVE_WITH_KNOTS((6,1,1,1,1,1,1,1,1,1,1,1,1,1,1,1,1,1,1,1,1,1,
1,1,1,1,1,1,1,1,1,1,1,1,1,1,1,1,1,1,1,1,1,1,1,1,1,1,1,1,1,1,1,1,1,1,1,1,
1,1,1,1,1,1,1,6),(0.,0.0153846153846154,0.0307692307692308,0.0461538461538462,
0.0615384615384615,0.0769230769230769,0.0923076923076923,0.107692307692308,
0.123076923076923,0.138461538461538,0.153846153846154,0.169230769230769,
0.184615384615385,0.2,0.215384615384615,0.230769230769231,0.246153846153846,
0.261538461538462,0.276923076923077,0.292307692307692,0.307692307692308,
0.323076923076923,0.338461538461538,0.353846153846154,0.369230769230769,
0.384615384615385,0.4,0.415384615384615,0.430769230769231,0.446153846153846,
0.461538461538462,0.476923076923077,0.492307692307692,0.507692307692308,
0.523076923076923,0.538461538461538,0.553846153846154,0.569230769230769,
0.584615384615384,0.6,0.615384615384615,0.63076923076923,0.646153846153846,
0.661538461538461,0.676923076923076,0.692307692307692,0.707692307692307,
0.723076923076922,0.738461538461538,0.753846153846153,0.769230769230768,
0.784615384615384,0.799999999999999,0.815384615384614,0.83076923076923,
0.846153846153845,0.86153846153846,0.876923076923076,0.892307692307691,
0.907692307692306,0.923076923076922,0.938461538461537,0.953846153846152,
0.969230769230768,0.984615384615383,0.994228156739704),.UNSPECIFIED.)
CURVE()
GEOMETRIC_REPRESENTATION_ITEM()
RATIONAL_B_SPLINE_CURVE((1.,1.,1.,1.,1.,1.,1.,1.,1.,1.,1.,1.,1.,1.,1.,1.,
1.,1.,1.,1.,1.,1.,1.,1.,1.,1.,1.,1.,1.,1.,1.,1.,1.,1.,1.,1.,1.,1.,1.,1.,
1.,1.,1.,1.,1.,1.,1.,1.,1.,1.,1.,1.,1.,1.,1.,1.,1.,1.,1.,1.,1.,1.,1.,1.,
1.,1.,1.,1.,1.,1.))
REPRESENTATION_ITEM('')
);
#249=(
BOUNDED_CURVE()
B_SPLINE_CURVE(5,(#36889,#36890,#36891,#36892,#36893,#36894,#36895,#36896,
#36897,#36898,#36899,#36900,#36901,#36902,#36903,#36904,#36905,#36906,#36907,
#36908,#36909,#36910,#36911,#36912,#36913,#36914,#36915,#36916,#36917,#36918,
#36919,#36920,#36921,#36922,#36923,#36924,#36925,#36926,#36927,#36928,#36929,
#36930,#36931,#36932,#36933,#36934,#36935,#36936,#36937,#36938,#36939,#36940,
#36941,#36942,#36943,#36944,#36945,#36946,#36947,#36948,#36949,#36950,#36951,
#36952,#36953,#36954,#36955,#36956,#36957,#36958),.UNSPECIFIED.,.F.,.F.)
B_SPLINE_CURVE_WITH_KNOTS((6,1,1,1,1,1,1,1,1,1,1,1,1,1,1,1,1,1,1,1,1,1,
1,1,1,1,1,1,1,1,1,1,1,1,1,1,1,1,1,1,1,1,1,1,1,1,1,1,1,1,1,1,1,1,1,1,1,1,
1,1,1,1,1,1,1,6),(0.00577184337449682,0.0153846153846154,0.0307692307692308,
0.0461538461538462,0.0615384615384615,0.0769230769230769,0.0923076923076923,
0.107692307692308,0.123076923076923,0.138461538461538,0.153846153846154,
0.169230769230769,0.184615384615385,0.2,0.215384615384615,0.230769230769231,
0.246153846153846,0.261538461538462,0.276923076923077,0.292307692307692,
0.307692307692308,0.323076923076923,0.338461538461538,0.353846153846154,
0.369230769230769,0.384615384615385,0.4,0.415384615384615,0.430769230769231,
0.446153846153846,0.461538461538462,0.476923076923077,0.492307692307692,
0.507692307692308,0.523076923076923,0.538461538461538,0.553846153846154,
0.569230769230769,0.584615384615384,0.6,0.615384615384615,0.63076923076923,
0.646153846153846,0.661538461538461,0.676923076923076,0.692307692307692,
0.707692307692307,0.723076923076922,0.738461538461538,0.753846153846153,
0.769230769230768,0.784615384615384,0.799999999999999,0.815384615384614,
0.83076923076923,0.846153846153845,0.86153846153846,0.876923076923076,0.892307692307691,
0.907692307692306,0.923076923076922,0.938461538461537,0.953846153846152,
0.969230769230768,0.984615384615383,1.),.UNSPECIFIED.)
CURVE()
GEOMETRIC_REPRESENTATION_ITEM()
RATIONAL_B_SPLINE_CURVE((1.,1.,1.,1.,1.,1.,1.,1.,1.,1.,1.,1.,1.,1.,1.,1.,
1.,1.,1.,1.,1.,1.,1.,1.,1.,1.,1.,1.,1.,1.,1.,1.,1.,1.,1.,1.,1.,1.,1.,1.,
1.,1.,1.,1.,1.,1.,1.,1.,1.,1.,1.,1.,1.,1.,1.,1.,1.,1.,1.,1.,1.,1.,1.,1.,
1.,1.,1.,1.,1.,1.))
REPRESENTATION_ITEM('')
);
#250=(
BOUNDED_CURVE()
B_SPLINE_CURVE(5,(#36962,#36963,#36964,#36965,#36966,#36967,#36968,#36969,
#36970,#36971,#36972,#36973,#36974,#36975,#36976,#36977,#36978,#36979,#36980,
#36981,#36982,#36983,#36984,#36985,#36986,#36987,#36988,#36989,#36990,#36991,
#36992,#36993,#36994,#36995,#36996,#36997,#36998,#36999,#37000,#37001,#37002,
#37003,#37004,#37005,#37006,#37007,#37008,#37009,#37010,#37011,#37012,#37013,
#37014,#37015,#37016,#37017,#37018,#37019,#37020,#37021,#37022,#37023,#37024,
#37025,#37026,#37027,#37028,#37029,#37030,#37031),.UNSPECIFIED.,.F.,.F.)
B_SPLINE_CURVE_WITH_KNOTS((6,1,1,1,1,1,1,1,1,1,1,1,1,1,1,1,1,1,1,1,1,1,
1,1,1,1,1,1,1,1,1,1,1,1,1,1,1,1,1,1,1,1,1,1,1,1,1,1,1,1,1,1,1,1,1,1,1,1,
1,1,1,1,1,1,1,6),(0.,0.0153846153846154,0.0307692307692308,0.0461538461538462,
0.0615384615384615,0.0769230769230769,0.0923076923076923,0.107692307692308,
0.123076923076923,0.138461538461538,0.153846153846154,0.169230769230769,
0.184615384615385,0.2,0.215384615384615,0.230769230769231,0.246153846153846,
0.261538461538462,0.276923076923077,0.292307692307692,0.307692307692308,
0.323076923076923,0.338461538461538,0.353846153846154,0.369230769230769,
0.384615384615385,0.4,0.415384615384615,0.430769230769231,0.446153846153846,
0.461538461538462,0.476923076923077,0.492307692307692,0.507692307692308,
0.523076923076923,0.538461538461538,0.553846153846154,0.569230769230769,
0.584615384615384,0.6,0.615384615384615,0.63076923076923,0.646153846153846,
0.661538461538461,0.676923076923076,0.692307692307692,0.707692307692307,
0.723076923076922,0.738461538461538,0.753846153846153,0.769230769230768,
0.784615384615384,0.799999999999999,0.815384615384614,0.83076923076923,
0.846153846153845,0.86153846153846,0.876923076923076,0.892307692307691,
0.907692307692306,0.923076923076922,0.938461538461537,0.953846153846152,
0.969230769230768,0.984615384615383,0.994228156739711),.UNSPECIFIED.)
CURVE()
GEOMETRIC_REPRESENTATION_ITEM()
RATIONAL_B_SPLINE_CURVE((1.,1.,1.,1.,1.,1.,1.,1.,1.,1.,1.,1.,1.,1.,1.,1.,
1.,1.,1.,1.,1.,1.,1.,1.,1.,1.,1.,1.,1.,1.,1.,1.,1.,1.,1.,1.,1.,1.,1.,1.,
1.,1.,1.,1.,1.,1.,1.,1.,1.,1.,1.,1.,1.,1.,1.,1.,1.,1.,1.,1.,1.,1.,1.,1.,
1.,1.,1.,1.,1.,1.))
REPRESENTATION_ITEM('')
);
#251=(
BOUNDED_CURVE()
B_SPLINE_CURVE(5,(#37035,#37036,#37037,#37038,#37039,#37040,#37041,#37042,
#37043,#37044,#37045,#37046,#37047,#37048,#37049,#37050,#37051,#37052,#37053,
#37054,#37055,#37056,#37057,#37058,#37059,#37060,#37061,#37062,#37063,#37064,
#37065,#37066,#37067,#37068,#37069,#37070,#37071,#37072,#37073,#37074,#37075,
#37076,#37077,#37078,#37079,#37080,#37081,#37082,#37083,#37084,#37085,#37086,
#37087,#37088,#37089,#37090,#37091,#37092,#37093,#37094,#37095,#37096,#37097,
#37098,#37099,#37100,#37101,#37102,#37103,#37104),.UNSPECIFIED.,.F.,.F.)
B_SPLINE_CURVE_WITH_KNOTS((6,1,1,1,1,1,1,1,1,1,1,1,1,1,1,1,1,1,1,1,1,1,
1,1,1,1,1,1,1,1,1,1,1,1,1,1,1,1,1,1,1,1,1,1,1,1,1,1,1,1,1,1,1,1,1,1,1,1,
1,1,1,1,1,1,1,6),(0.00577184337450313,0.0153846153846154,0.0307692307692308,
0.0461538461538462,0.0615384615384615,0.0769230769230769,0.0923076923076923,
0.107692307692308,0.123076923076923,0.138461538461538,0.153846153846154,
0.169230769230769,0.184615384615385,0.2,0.215384615384615,0.230769230769231,
0.246153846153846,0.261538461538462,0.276923076923077,0.292307692307692,
0.307692307692308,0.323076923076923,0.338461538461538,0.353846153846154,
0.369230769230769,0.384615384615385,0.4,0.415384615384615,0.430769230769231,
0.446153846153846,0.461538461538462,0.476923076923077,0.492307692307692,
0.507692307692308,0.523076923076923,0.538461538461538,0.553846153846154,
0.569230769230769,0.584615384615384,0.6,0.615384615384615,0.63076923076923,
0.646153846153846,0.661538461538461,0.676923076923076,0.692307692307692,
0.707692307692307,0.723076923076922,0.738461538461538,0.753846153846153,
0.769230769230768,0.784615384615384,0.799999999999999,0.815384615384614,
0.83076923076923,0.846153846153845,0.86153846153846,0.876923076923076,0.892307692307691,
0.907692307692306,0.923076923076922,0.938461538461537,0.953846153846152,
0.969230769230768,0.984615384615383,1.),.UNSPECIFIED.)
CURVE()
GEOMETRIC_REPRESENTATION_ITEM()
RATIONAL_B_SPLINE_CURVE((1.,1.,1.,1.,1.,1.,1.,1.,1.,1.,1.,1.,1.,1.,1.,1.,
1.,1.,1.,1.,1.,1.,1.,1.,1.,1.,1.,1.,1.,1.,1.,1.,1.,1.,1.,1.,1.,1.,1.,1.,
1.,1.,1.,1.,1.,1.,1.,1.,1.,1.,1.,1.,1.,1.,1.,1.,1.,1.,1.,1.,1.,1.,1.,1.,
1.,1.,1.,1.,1.,1.))
REPRESENTATION_ITEM('')
);
#252=(
BOUNDED_CURVE()
B_SPLINE_CURVE(5,(#37108,#37109,#37110,#37111,#37112,#37113,#37114,#37115,
#37116,#37117,#37118,#37119,#37120,#37121,#37122,#37123,#37124,#37125,#37126,
#37127,#37128,#37129,#37130,#37131,#37132,#37133,#37134,#37135,#37136,#37137,
#37138,#37139,#37140,#37141,#37142,#37143,#37144,#37145,#37146,#37147,#37148,
#37149,#37150,#37151,#37152,#37153,#37154,#37155,#37156,#37157,#37158,#37159,
#37160,#37161,#37162,#37163,#37164,#37165,#37166,#37167,#37168,#37169,#37170,
#37171,#37172,#37173,#37174,#37175,#37176,#37177),.UNSPECIFIED.,.F.,.F.)
B_SPLINE_CURVE_WITH_KNOTS((6,1,1,1,1,1,1,1,1,1,1,1,1,1,1,1,1,1,1,1,1,1,
1,1,1,1,1,1,1,1,1,1,1,1,1,1,1,1,1,1,1,1,1,1,1,1,1,1,1,1,1,1,1,1,1,1,1,1,
1,1,1,1,1,1,1,6),(0.,0.0153846153846154,0.0307692307692308,0.0461538461538462,
0.0615384615384615,0.0769230769230769,0.0923076923076923,0.107692307692308,
0.123076923076923,0.138461538461538,0.153846153846154,0.169230769230769,
0.184615384615385,0.2,0.215384615384615,0.230769230769231,0.246153846153846,
0.261538461538462,0.276923076923077,0.292307692307692,0.307692307692308,
0.323076923076923,0.338461538461538,0.353846153846154,0.369230769230769,
0.384615384615385,0.4,0.415384615384615,0.430769230769231,0.446153846153846,
0.461538461538462,0.476923076923077,0.492307692307692,0.507692307692308,
0.523076923076923,0.538461538461538,0.553846153846154,0.569230769230769,
0.584615384615384,0.6,0.615384615384615,0.63076923076923,0.646153846153846,
0.661538461538461,0.676923076923076,0.692307692307692,0.707692307692307,
0.723076923076922,0.738461538461538,0.753846153846153,0.769230769230768,
0.784615384615384,0.799999999999999,0.815384615384614,0.83076923076923,
0.846153846153845,0.86153846153846,0.876923076923076,0.892307692307691,
0.907692307692306,0.923076923076922,0.938461538461537,0.953846153846152,
0.969230769230768,0.984615384615383,0.9942281567397),.UNSPECIFIED.)
CURVE()
GEOMETRIC_REPRESENTATION_ITEM()
RATIONAL_B_SPLINE_CURVE((1.,1.,1.,1.,1.,1.,1.,1.,1.,1.,1.,1.,1.,1.,1.,1.,
1.,1.,1.,1.,1.,1.,1.,1.,1.,1.,1.,1.,1.,1.,1.,1.,1.,1.,1.,1.,1.,1.,1.,1.,
1.,1.,1.,1.,1.,1.,1.,1.,1.,1.,1.,1.,1.,1.,1.,1.,1.,1.,1.,1.,1.,1.,1.,1.,
1.,1.,1.,1.,1.,1.))
REPRESENTATION_ITEM('')
);
#253=(
BOUNDED_CURVE()
B_SPLINE_CURVE(5,(#37181,#37182,#37183,#37184,#37185,#37186,#37187,#37188,
#37189,#37190,#37191,#37192,#37193,#37194,#37195,#37196,#37197,#37198,#37199,
#37200,#37201,#37202,#37203,#37204,#37205,#37206,#37207,#37208,#37209,#37210,
#37211,#37212,#37213,#37214,#37215,#37216,#37217,#37218,#37219,#37220,#37221,
#37222,#37223,#37224,#37225,#37226,#37227,#37228,#37229,#37230,#37231,#37232,
#37233,#37234,#37235,#37236,#37237,#37238,#37239,#37240,#37241,#37242,#37243,
#37244,#37245,#37246,#37247,#37248,#37249,#37250),.UNSPECIFIED.,.F.,.F.)
B_SPLINE_CURVE_WITH_KNOTS((6,1,1,1,1,1,1,1,1,1,1,1,1,1,1,1,1,1,1,1,1,1,
1,1,1,1,1,1,1,1,1,1,1,1,1,1,1,1,1,1,1,1,1,1,1,1,1,1,1,1,1,1,1,1,1,1,1,1,
1,1,1,1,1,1,1,6),(0.00577184337452087,0.0153846153846154,0.0307692307692308,
0.0461538461538462,0.0615384615384615,0.0769230769230769,0.0923076923076923,
0.107692307692308,0.123076923076923,0.138461538461538,0.153846153846154,
0.169230769230769,0.184615384615385,0.2,0.215384615384615,0.230769230769231,
0.246153846153846,0.261538461538462,0.276923076923077,0.292307692307692,
0.307692307692308,0.323076923076923,0.338461538461538,0.353846153846154,
0.369230769230769,0.384615384615385,0.4,0.415384615384615,0.430769230769231,
0.446153846153846,0.461538461538462,0.476923076923077,0.492307692307692,
0.507692307692308,0.523076923076923,0.538461538461538,0.553846153846154,
0.569230769230769,0.584615384615384,0.6,0.615384615384615,0.63076923076923,
0.646153846153846,0.661538461538461,0.676923076923076,0.692307692307692,
0.707692307692307,0.723076923076922,0.738461538461538,0.753846153846153,
0.769230769230768,0.784615384615384,0.799999999999999,0.815384615384614,
0.83076923076923,0.846153846153845,0.86153846153846,0.876923076923076,0.892307692307691,
0.907692307692306,0.923076923076922,0.938461538461537,0.953846153846152,
0.969230769230768,0.984615384615383,1.),.UNSPECIFIED.)
CURVE()
GEOMETRIC_REPRESENTATION_ITEM()
RATIONAL_B_SPLINE_CURVE((1.,1.,1.,1.,1.,1.,1.,1.,1.,1.,1.,1.,1.,1.,1.,1.,
1.,1.,1.,1.,1.,1.,1.,1.,1.,1.,1.,1.,1.,1.,1.,1.,1.,1.,1.,1.,1.,1.,1.,1.,
1.,1.,1.,1.,1.,1.,1.,1.,1.,1.,1.,1.,1.,1.,1.,1.,1.,1.,1.,1.,1.,1.,1.,1.,
1.,1.,1.,1.,1.,1.))
REPRESENTATION_ITEM('')
);
#254=(
BOUNDED_CURVE()
B_SPLINE_CURVE(5,(#37254,#37255,#37256,#37257,#37258,#37259,#37260,#37261,
#37262,#37263,#37264,#37265,#37266,#37267,#37268,#37269,#37270,#37271,#37272,
#37273,#37274,#37275,#37276,#37277,#37278,#37279,#37280,#37281,#37282,#37283,
#37284,#37285,#37286,#37287,#37288,#37289,#37290,#37291,#37292,#37293,#37294,
#37295,#37296,#37297,#37298,#37299,#37300,#37301,#37302,#37303,#37304,#37305,
#37306,#37307,#37308,#37309,#37310,#37311,#37312,#37313,#37314,#37315,#37316,
#37317,#37318,#37319,#37320,#37321,#37322,#37323),.UNSPECIFIED.,.F.,.F.)
B_SPLINE_CURVE_WITH_KNOTS((6,1,1,1,1,1,1,1,1,1,1,1,1,1,1,1,1,1,1,1,1,1,
1,1,1,1,1,1,1,1,1,1,1,1,1,1,1,1,1,1,1,1,1,1,1,1,1,1,1,1,1,1,1,1,1,1,1,1,
1,1,1,1,1,1,1,6),(0.,0.0153846153846154,0.0307692307692308,0.0461538461538462,
0.0615384615384615,0.0769230769230769,0.0923076923076923,0.107692307692308,
0.123076923076923,0.138461538461538,0.153846153846154,0.169230769230769,
0.184615384615385,0.2,0.215384615384615,0.230769230769231,0.246153846153846,
0.261538461538462,0.276923076923077,0.292307692307692,0.307692307692308,
0.323076923076923,0.338461538461538,0.353846153846154,0.369230769230769,
0.384615384615385,0.4,0.415384615384615,0.430769230769231,0.446153846153846,
0.461538461538462,0.476923076923077,0.492307692307692,0.507692307692308,
0.523076923076923,0.538461538461538,0.553846153846154,0.569230769230769,
0.584615384615384,0.6,0.615384615384615,0.63076923076923,0.646153846153846,
0.661538461538461,0.676923076923076,0.692307692307692,0.707692307692307,
0.723076923076922,0.738461538461538,0.753846153846153,0.769230769230768,
0.784615384615384,0.799999999999999,0.815384615384614,0.83076923076923,
0.846153846153845,0.86153846153846,0.876923076923076,0.892307692307691,
0.907692307692306,0.923076923076922,0.938461538461537,0.953846153846152,
0.969230769230768,0.984615384615383,0.994228156739692),.UNSPECIFIED.)
CURVE()
GEOMETRIC_REPRESENTATION_ITEM()
RATIONAL_B_SPLINE_CURVE((1.,1.,1.,1.,1.,1.,1.,1.,1.,1.,1.,1.,1.,1.,1.,1.,
1.,1.,1.,1.,1.,1.,1.,1.,1.,1.,1.,1.,1.,1.,1.,1.,1.,1.,1.,1.,1.,1.,1.,1.,
1.,1.,1.,1.,1.,1.,1.,1.,1.,1.,1.,1.,1.,1.,1.,1.,1.,1.,1.,1.,1.,1.,1.,1.,
1.,1.,1.,1.,1.,1.))
REPRESENTATION_ITEM('')
);
#255=(
BOUNDED_CURVE()
B_SPLINE_CURVE(5,(#37327,#37328,#37329,#37330,#37331,#37332,#37333,#37334,
#37335,#37336,#37337,#37338,#37339,#37340,#37341,#37342,#37343,#37344,#37345,
#37346,#37347,#37348,#37349,#37350,#37351,#37352,#37353,#37354,#37355,#37356,
#37357,#37358,#37359,#37360,#37361,#37362,#37363,#37364,#37365,#37366,#37367,
#37368,#37369,#37370,#37371,#37372,#37373,#37374,#37375,#37376,#37377,#37378,
#37379,#37380,#37381,#37382,#37383,#37384,#37385,#37386,#37387,#37388,#37389,
#37390,#37391,#37392,#37393,#37394,#37395,#37396),.UNSPECIFIED.,.F.,.F.)
B_SPLINE_CURVE_WITH_KNOTS((6,1,1,1,1,1,1,1,1,1,1,1,1,1,1,1,1,1,1,1,1,1,
1,1,1,1,1,1,1,1,1,1,1,1,1,1,1,1,1,1,1,1,1,1,1,1,1,1,1,1,1,1,1,1,1,1,1,1,
1,1,1,1,1,1,1,6),(0.00577184337450777,0.0153846153846154,0.0307692307692308,
0.0461538461538462,0.0615384615384615,0.0769230769230769,0.0923076923076923,
0.107692307692308,0.123076923076923,0.138461538461538,0.153846153846154,
0.169230769230769,0.184615384615385,0.2,0.215384615384615,0.230769230769231,
0.246153846153846,0.261538461538462,0.276923076923077,0.292307692307692,
0.307692307692308,0.323076923076923,0.338461538461538,0.353846153846154,
0.369230769230769,0.384615384615385,0.4,0.415384615384615,0.430769230769231,
0.446153846153846,0.461538461538462,0.476923076923077,0.492307692307692,
0.507692307692308,0.523076923076923,0.538461538461538,0.553846153846154,
0.569230769230769,0.584615384615384,0.6,0.615384615384615,0.63076923076923,
0.646153846153846,0.661538461538461,0.676923076923076,0.692307692307692,
0.707692307692307,0.723076923076922,0.738461538461538,0.753846153846153,
0.769230769230768,0.784615384615384,0.799999999999999,0.815384615384614,
0.83076923076923,0.846153846153845,0.86153846153846,0.876923076923076,0.892307692307691,
0.907692307692306,0.923076923076922,0.938461538461537,0.953846153846152,
0.969230769230768,0.984615384615383,1.),.UNSPECIFIED.)
CURVE()
GEOMETRIC_REPRESENTATION_ITEM()
RATIONAL_B_SPLINE_CURVE((1.,1.,1.,1.,1.,1.,1.,1.,1.,1.,1.,1.,1.,1.,1.,1.,
1.,1.,1.,1.,1.,1.,1.,1.,1.,1.,1.,1.,1.,1.,1.,1.,1.,1.,1.,1.,1.,1.,1.,1.,
1.,1.,1.,1.,1.,1.,1.,1.,1.,1.,1.,1.,1.,1.,1.,1.,1.,1.,1.,1.,1.,1.,1.,1.,
1.,1.,1.,1.,1.,1.))
REPRESENTATION_ITEM('')
);
#256=(
BOUNDED_CURVE()
B_SPLINE_CURVE(5,(#37400,#37401,#37402,#37403,#37404,#37405,#37406,#37407,
#37408,#37409,#37410,#37411,#37412,#37413,#37414,#37415,#37416,#37417,#37418,
#37419,#37420,#37421,#37422,#37423,#37424,#37425,#37426,#37427,#37428,#37429,
#37430,#37431,#37432,#37433,#37434,#37435,#37436,#37437,#37438,#37439,#37440,
#37441,#37442,#37443,#37444,#37445,#37446,#37447,#37448,#37449,#37450,#37451,
#37452,#37453,#37454,#37455,#37456,#37457,#37458,#37459,#37460,#37461,#37462,
#37463,#37464,#37465,#37466,#37467,#37468,#37469),.UNSPECIFIED.,.F.,.F.)
B_SPLINE_CURVE_WITH_KNOTS((6,1,1,1,1,1,1,1,1,1,1,1,1,1,1,1,1,1,1,1,1,1,
1,1,1,1,1,1,1,1,1,1,1,1,1,1,1,1,1,1,1,1,1,1,1,1,1,1,1,1,1,1,1,1,1,1,1,1,
1,1,1,1,1,1,1,6),(0.,0.0153846153846154,0.0307692307692308,0.0461538461538462,
0.0615384615384615,0.0769230769230769,0.0923076923076923,0.107692307692308,
0.123076923076923,0.138461538461538,0.153846153846154,0.169230769230769,
0.184615384615385,0.2,0.215384615384615,0.230769230769231,0.246153846153846,
0.261538461538462,0.276923076923077,0.292307692307692,0.307692307692308,
0.323076923076923,0.338461538461538,0.353846153846154,0.369230769230769,
0.384615384615385,0.4,0.415384615384615,0.430769230769231,0.446153846153846,
0.461538461538462,0.476923076923077,0.492307692307692,0.507692307692308,
0.523076923076923,0.538461538461538,0.553846153846154,0.569230769230769,
0.584615384615384,0.6,0.615384615384615,0.63076923076923,0.646153846153846,
0.661538461538461,0.676923076923076,0.692307692307692,0.707692307692307,
0.723076923076922,0.738461538461538,0.753846153846153,0.769230769230768,
0.784615384615384,0.799999999999999,0.815384615384614,0.83076923076923,
0.846153846153845,0.86153846153846,0.876923076923076,0.892307692307691,
0.907692307692306,0.923076923076922,0.938461538461537,0.953846153846152,
0.969230769230768,0.984615384615383,0.994228156739701),.UNSPECIFIED.)
CURVE()
GEOMETRIC_REPRESENTATION_ITEM()
RATIONAL_B_SPLINE_CURVE((1.,1.,1.,1.,1.,1.,1.,1.,1.,1.,1.,1.,1.,1.,1.,1.,
1.,1.,1.,1.,1.,1.,1.,1.,1.,1.,1.,1.,1.,1.,1.,1.,1.,1.,1.,1.,1.,1.,1.,1.,
1.,1.,1.,1.,1.,1.,1.,1.,1.,1.,1.,1.,1.,1.,1.,1.,1.,1.,1.,1.,1.,1.,1.,1.,
1.,1.,1.,1.,1.,1.))
REPRESENTATION_ITEM('')
);
#257=(
BOUNDED_CURVE()
B_SPLINE_CURVE(5,(#37473,#37474,#37475,#37476,#37477,#37478,#37479,#37480,
#37481,#37482,#37483,#37484,#37485,#37486,#37487,#37488,#37489,#37490,#37491,
#37492,#37493,#37494,#37495,#37496,#37497,#37498,#37499,#37500,#37501,#37502,
#37503,#37504,#37505,#37506,#37507,#37508,#37509,#37510,#37511,#37512,#37513,
#37514,#37515,#37516,#37517,#37518,#37519,#37520,#37521,#37522,#37523,#37524,
#37525,#37526,#37527,#37528,#37529,#37530,#37531,#37532,#37533,#37534,#37535,
#37536,#37537,#37538,#37539,#37540,#37541,#37542),.UNSPECIFIED.,.F.,.F.)
B_SPLINE_CURVE_WITH_KNOTS((6,1,1,1,1,1,1,1,1,1,1,1,1,1,1,1,1,1,1,1,1,1,
1,1,1,1,1,1,1,1,1,1,1,1,1,1,1,1,1,1,1,1,1,1,1,1,1,1,1,1,1,1,1,1,1,1,1,1,
1,1,1,1,1,1,1,6),(0.00577184337450943,0.0153846153846154,0.0307692307692308,
0.0461538461538462,0.0615384615384615,0.0769230769230769,0.0923076923076923,
0.107692307692308,0.123076923076923,0.138461538461538,0.153846153846154,
0.169230769230769,0.184615384615385,0.2,0.215384615384615,0.230769230769231,
0.246153846153846,0.261538461538462,0.276923076923077,0.292307692307692,
0.307692307692308,0.323076923076923,0.338461538461538,0.353846153846154,
0.369230769230769,0.384615384615385,0.4,0.415384615384615,0.430769230769231,
0.446153846153846,0.461538461538462,0.476923076923077,0.492307692307692,
0.507692307692308,0.523076923076923,0.538461538461538,0.553846153846154,
0.569230769230769,0.584615384615384,0.6,0.615384615384615,0.63076923076923,
0.646153846153846,0.661538461538461,0.676923076923076,0.692307692307692,
0.707692307692307,0.723076923076922,0.738461538461538,0.753846153846153,
0.769230769230768,0.784615384615384,0.799999999999999,0.815384615384614,
0.83076923076923,0.846153846153845,0.86153846153846,0.876923076923076,0.892307692307691,
0.907692307692306,0.923076923076922,0.938461538461537,0.953846153846152,
0.969230769230768,0.984615384615383,1.),.UNSPECIFIED.)
CURVE()
GEOMETRIC_REPRESENTATION_ITEM()
RATIONAL_B_SPLINE_CURVE((1.,1.,1.,1.,1.,1.,1.,1.,1.,1.,1.,1.,1.,1.,1.,1.,
1.,1.,1.,1.,1.,1.,1.,1.,1.,1.,1.,1.,1.,1.,1.,1.,1.,1.,1.,1.,1.,1.,1.,1.,
1.,1.,1.,1.,1.,1.,1.,1.,1.,1.,1.,1.,1.,1.,1.,1.,1.,1.,1.,1.,1.,1.,1.,1.,
1.,1.,1.,1.,1.,1.))
REPRESENTATION_ITEM('')
);
#258=(
BOUNDED_CURVE()
B_SPLINE_CURVE(5,(#37546,#37547,#37548,#37549,#37550,#37551,#37552,#37553,
#37554,#37555,#37556,#37557,#37558,#37559,#37560,#37561,#37562,#37563,#37564,
#37565,#37566,#37567,#37568,#37569,#37570,#37571,#37572,#37573,#37574,#37575,
#37576,#37577,#37578,#37579,#37580,#37581,#37582,#37583,#37584,#37585,#37586,
#37587,#37588,#37589,#37590,#37591,#37592,#37593,#37594,#37595,#37596,#37597,
#37598,#37599,#37600,#37601,#37602,#37603,#37604,#37605,#37606,#37607,#37608,
#37609,#37610,#37611,#37612,#37613,#37614,#37615),.UNSPECIFIED.,.F.,.F.)
B_SPLINE_CURVE_WITH_KNOTS((6,1,1,1,1,1,1,1,1,1,1,1,1,1,1,1,1,1,1,1,1,1,
1,1,1,1,1,1,1,1,1,1,1,1,1,1,1,1,1,1,1,1,1,1,1,1,1,1,1,1,1,1,1,1,1,1,1,1,
1,1,1,1,1,1,1,6),(0.,0.0153846153846154,0.0307692307692308,0.0461538461538462,
0.0615384615384615,0.0769230769230769,0.0923076923076923,0.107692307692308,
0.123076923076923,0.138461538461538,0.153846153846154,0.169230769230769,
0.184615384615385,0.2,0.215384615384615,0.230769230769231,0.246153846153846,
0.261538461538462,0.276923076923077,0.292307692307692,0.307692307692308,
0.323076923076923,0.338461538461538,0.353846153846154,0.369230769230769,
0.384615384615385,0.4,0.415384615384615,0.430769230769231,0.446153846153846,
0.461538461538462,0.476923076923077,0.492307692307692,0.507692307692308,
0.523076923076923,0.538461538461538,0.553846153846154,0.569230769230769,
0.584615384615384,0.6,0.615384615384615,0.63076923076923,0.646153846153846,
0.661538461538461,0.676923076923076,0.692307692307692,0.707692307692307,
0.723076923076922,0.738461538461538,0.753846153846153,0.769230769230768,
0.784615384615384,0.799999999999999,0.815384615384614,0.83076923076923,
0.846153846153845,0.86153846153846,0.876923076923076,0.892307692307691,
0.907692307692306,0.923076923076922,0.938461538461537,0.953846153846152,
0.969230769230768,0.984615384615383,0.994228156739699),.UNSPECIFIED.)
CURVE()
GEOMETRIC_REPRESENTATION_ITEM()
RATIONAL_B_SPLINE_CURVE((1.,1.,1.,1.,1.,1.,1.,1.,1.,1.,1.,1.,1.,1.,1.,1.,
1.,1.,1.,1.,1.,1.,1.,1.,1.,1.,1.,1.,1.,1.,1.,1.,1.,1.,1.,1.,1.,1.,1.,1.,
1.,1.,1.,1.,1.,1.,1.,1.,1.,1.,1.,1.,1.,1.,1.,1.,1.,1.,1.,1.,1.,1.,1.,1.,
1.,1.,1.,1.,1.,1.))
REPRESENTATION_ITEM('')
);
#259=(
BOUNDED_CURVE()
B_SPLINE_CURVE(5,(#37619,#37620,#37621,#37622,#37623,#37624,#37625,#37626,
#37627,#37628,#37629,#37630,#37631,#37632,#37633,#37634,#37635,#37636,#37637,
#37638,#37639,#37640,#37641,#37642,#37643,#37644,#37645,#37646,#37647,#37648,
#37649,#37650,#37651,#37652,#37653,#37654,#37655,#37656,#37657,#37658,#37659,
#37660,#37661,#37662,#37663,#37664,#37665,#37666,#37667,#37668,#37669,#37670,
#37671,#37672,#37673,#37674,#37675,#37676,#37677,#37678,#37679,#37680,#37681,
#37682,#37683,#37684,#37685,#37686,#37687,#37688),.UNSPECIFIED.,.F.,.F.)
B_SPLINE_CURVE_WITH_KNOTS((6,1,1,1,1,1,1,1,1,1,1,1,1,1,1,1,1,1,1,1,1,1,
1,1,1,1,1,1,1,1,1,1,1,1,1,1,1,1,1,1,1,1,1,1,1,1,1,1,1,1,1,1,1,1,1,1,1,1,
1,1,1,1,1,1,1,6),(0.00577184337448657,0.0153846153846154,0.0307692307692308,
0.0461538461538462,0.0615384615384615,0.0769230769230769,0.0923076923076923,
0.107692307692308,0.123076923076923,0.138461538461538,0.153846153846154,
0.169230769230769,0.184615384615385,0.2,0.215384615384615,0.230769230769231,
0.246153846153846,0.261538461538462,0.276923076923077,0.292307692307692,
0.307692307692308,0.323076923076923,0.338461538461538,0.353846153846154,
0.369230769230769,0.384615384615385,0.4,0.415384615384615,0.430769230769231,
0.446153846153846,0.461538461538462,0.476923076923077,0.492307692307692,
0.507692307692308,0.523076923076923,0.538461538461538,0.553846153846154,
0.569230769230769,0.584615384615384,0.6,0.615384615384615,0.63076923076923,
0.646153846153846,0.661538461538461,0.676923076923076,0.692307692307692,
0.707692307692307,0.723076923076922,0.738461538461538,0.753846153846153,
0.769230769230768,0.784615384615384,0.799999999999999,0.815384615384614,
0.83076923076923,0.846153846153845,0.86153846153846,0.876923076923076,0.892307692307691,
0.907692307692306,0.923076923076922,0.938461538461537,0.953846153846152,
0.969230769230768,0.984615384615383,1.),.UNSPECIFIED.)
CURVE()
GEOMETRIC_REPRESENTATION_ITEM()
RATIONAL_B_SPLINE_CURVE((1.,1.,1.,1.,1.,1.,1.,1.,1.,1.,1.,1.,1.,1.,1.,1.,
1.,1.,1.,1.,1.,1.,1.,1.,1.,1.,1.,1.,1.,1.,1.,1.,1.,1.,1.,1.,1.,1.,1.,1.,
1.,1.,1.,1.,1.,1.,1.,1.,1.,1.,1.,1.,1.,1.,1.,1.,1.,1.,1.,1.,1.,1.,1.,1.,
1.,1.,1.,1.,1.,1.))
REPRESENTATION_ITEM('')
);
#260=(
BOUNDED_CURVE()
B_SPLINE_CURVE(5,(#37692,#37693,#37694,#37695,#37696,#37697,#37698,#37699,
#37700,#37701,#37702,#37703,#37704,#37705,#37706,#37707,#37708,#37709,#37710,
#37711,#37712,#37713,#37714,#37715,#37716,#37717,#37718,#37719,#37720,#37721,
#37722,#37723,#37724,#37725,#37726,#37727,#37728,#37729,#37730,#37731,#37732,
#37733,#37734,#37735,#37736,#37737,#37738,#37739,#37740,#37741,#37742,#37743,
#37744,#37745,#37746,#37747,#37748,#37749,#37750,#37751,#37752,#37753,#37754,
#37755,#37756,#37757,#37758,#37759,#37760,#37761),.UNSPECIFIED.,.F.,.F.)
B_SPLINE_CURVE_WITH_KNOTS((6,1,1,1,1,1,1,1,1,1,1,1,1,1,1,1,1,1,1,1,1,1,
1,1,1,1,1,1,1,1,1,1,1,1,1,1,1,1,1,1,1,1,1,1,1,1,1,1,1,1,1,1,1,1,1,1,1,1,
1,1,1,1,1,1,1,6),(0.,0.0153846153846154,0.0307692307692308,0.0461538461538462,
0.0615384615384615,0.0769230769230769,0.0923076923076923,0.107692307692308,
0.123076923076923,0.138461538461538,0.153846153846154,0.169230769230769,
0.184615384615385,0.2,0.215384615384615,0.230769230769231,0.246153846153846,
0.261538461538462,0.276923076923077,0.292307692307692,0.307692307692308,
0.323076923076923,0.338461538461538,0.353846153846154,0.369230769230769,
0.384615384615385,0.4,0.415384615384615,0.430769230769231,0.446153846153846,
0.461538461538462,0.476923076923077,0.492307692307692,0.507692307692308,
0.523076923076923,0.538461538461538,0.553846153846154,0.569230769230769,
0.584615384615384,0.6,0.615384615384615,0.63076923076923,0.646153846153846,
0.661538461538461,0.676923076923076,0.692307692307692,0.707692307692307,
0.723076923076922,0.738461538461538,0.753846153846153,0.769230769230768,
0.784615384615384,0.799999999999999,0.815384615384614,0.83076923076923,
0.846153846153845,0.86153846153846,0.876923076923076,0.892307692307691,
0.907692307692306,0.923076923076922,0.938461538461537,0.953846153846152,
0.969230769230768,0.984615384615383,0.994228156739709),.UNSPECIFIED.)
CURVE()
GEOMETRIC_REPRESENTATION_ITEM()
RATIONAL_B_SPLINE_CURVE((1.,1.,1.,1.,1.,1.,1.,1.,1.,1.,1.,1.,1.,1.,1.,1.,
1.,1.,1.,1.,1.,1.,1.,1.,1.,1.,1.,1.,1.,1.,1.,1.,1.,1.,1.,1.,1.,1.,1.,1.,
1.,1.,1.,1.,1.,1.,1.,1.,1.,1.,1.,1.,1.,1.,1.,1.,1.,1.,1.,1.,1.,1.,1.,1.,
1.,1.,1.,1.,1.,1.))
REPRESENTATION_ITEM('')
);
#261=(
BOUNDED_CURVE()
B_SPLINE_CURVE(5,(#37765,#37766,#37767,#37768,#37769,#37770,#37771,#37772,
#37773,#37774,#37775,#37776,#37777,#37778,#37779,#37780,#37781,#37782,#37783,
#37784,#37785,#37786,#37787,#37788,#37789,#37790,#37791,#37792,#37793,#37794,
#37795,#37796,#37797,#37798,#37799,#37800,#37801,#37802,#37803,#37804,#37805,
#37806,#37807,#37808,#37809,#37810,#37811,#37812,#37813,#37814,#37815,#37816,
#37817,#37818,#37819,#37820,#37821,#37822,#37823,#37824,#37825,#37826,#37827,
#37828,#37829,#37830,#37831,#37832,#37833,#37834),.UNSPECIFIED.,.F.,.F.)
B_SPLINE_CURVE_WITH_KNOTS((6,1,1,1,1,1,1,1,1,1,1,1,1,1,1,1,1,1,1,1,1,1,
1,1,1,1,1,1,1,1,1,1,1,1,1,1,1,1,1,1,1,1,1,1,1,1,1,1,1,1,1,1,1,1,1,1,1,1,
1,1,1,1,1,1,1,6),(0.00577184337451132,0.0153846153846154,0.0307692307692308,
0.0461538461538462,0.0615384615384615,0.0769230769230769,0.0923076923076923,
0.107692307692308,0.123076923076923,0.138461538461538,0.153846153846154,
0.169230769230769,0.184615384615385,0.2,0.215384615384615,0.230769230769231,
0.246153846153846,0.261538461538462,0.276923076923077,0.292307692307692,
0.307692307692308,0.323076923076923,0.338461538461538,0.353846153846154,
0.369230769230769,0.384615384615385,0.4,0.415384615384615,0.430769230769231,
0.446153846153846,0.461538461538462,0.476923076923077,0.492307692307692,
0.507692307692308,0.523076923076923,0.538461538461538,0.553846153846154,
0.569230769230769,0.584615384615384,0.6,0.615384615384615,0.63076923076923,
0.646153846153846,0.661538461538461,0.676923076923076,0.692307692307692,
0.707692307692307,0.723076923076922,0.738461538461538,0.753846153846153,
0.769230769230768,0.784615384615384,0.799999999999999,0.815384615384614,
0.83076923076923,0.846153846153845,0.86153846153846,0.876923076923076,0.892307692307691,
0.907692307692306,0.923076923076922,0.938461538461537,0.953846153846152,
0.969230769230768,0.984615384615383,1.),.UNSPECIFIED.)
CURVE()
GEOMETRIC_REPRESENTATION_ITEM()
RATIONAL_B_SPLINE_CURVE((1.,1.,1.,1.,1.,1.,1.,1.,1.,1.,1.,1.,1.,1.,1.,1.,
1.,1.,1.,1.,1.,1.,1.,1.,1.,1.,1.,1.,1.,1.,1.,1.,1.,1.,1.,1.,1.,1.,1.,1.,
1.,1.,1.,1.,1.,1.,1.,1.,1.,1.,1.,1.,1.,1.,1.,1.,1.,1.,1.,1.,1.,1.,1.,1.,
1.,1.,1.,1.,1.,1.))
REPRESENTATION_ITEM('')
);
#262=(
BOUNDED_CURVE()
B_SPLINE_CURVE(5,(#37838,#37839,#37840,#37841,#37842,#37843,#37844,#37845,
#37846,#37847,#37848,#37849,#37850,#37851,#37852,#37853,#37854,#37855,#37856,
#37857,#37858,#37859,#37860,#37861,#37862,#37863,#37864,#37865,#37866,#37867,
#37868,#37869,#37870,#37871,#37872,#37873,#37874,#37875,#37876,#37877,#37878,
#37879,#37880,#37881,#37882,#37883,#37884,#37885,#37886,#37887,#37888,#37889,
#37890,#37891,#37892,#37893,#37894,#37895,#37896,#37897,#37898,#37899,#37900,
#37901,#37902,#37903,#37904,#37905,#37906,#37907),.UNSPECIFIED.,.F.,.F.)
B_SPLINE_CURVE_WITH_KNOTS((6,1,1,1,1,1,1,1,1,1,1,1,1,1,1,1,1,1,1,1,1,1,
1,1,1,1,1,1,1,1,1,1,1,1,1,1,1,1,1,1,1,1,1,1,1,1,1,1,1,1,1,1,1,1,1,1,1,1,
1,1,1,1,1,1,1,6),(0.,0.0153846153846154,0.0307692307692308,0.0461538461538462,
0.0615384615384615,0.0769230769230769,0.0923076923076923,0.107692307692308,
0.123076923076923,0.138461538461538,0.153846153846154,0.169230769230769,
0.184615384615385,0.2,0.215384615384615,0.230769230769231,0.246153846153846,
0.261538461538462,0.276923076923077,0.292307692307692,0.307692307692308,
0.323076923076923,0.338461538461538,0.353846153846154,0.369230769230769,
0.384615384615385,0.4,0.415384615384615,0.430769230769231,0.446153846153846,
0.461538461538462,0.476923076923077,0.492307692307692,0.507692307692308,
0.523076923076923,0.538461538461538,0.553846153846154,0.569230769230769,
0.584615384615384,0.6,0.615384615384615,0.63076923076923,0.646153846153846,
0.661538461538461,0.676923076923076,0.692307692307692,0.707692307692307,
0.723076923076922,0.738461538461538,0.753846153846153,0.769230769230768,
0.784615384615384,0.799999999999999,0.815384615384614,0.83076923076923,
0.846153846153845,0.86153846153846,0.876923076923076,0.892307692307691,
0.907692307692306,0.923076923076922,0.938461538461537,0.953846153846152,
0.969230769230768,0.984615384615383,0.994228156739705),.UNSPECIFIED.)
CURVE()
GEOMETRIC_REPRESENTATION_ITEM()
RATIONAL_B_SPLINE_CURVE((1.,1.,1.,1.,1.,1.,1.,1.,1.,1.,1.,1.,1.,1.,1.,1.,
1.,1.,1.,1.,1.,1.,1.,1.,1.,1.,1.,1.,1.,1.,1.,1.,1.,1.,1.,1.,1.,1.,1.,1.,
1.,1.,1.,1.,1.,1.,1.,1.,1.,1.,1.,1.,1.,1.,1.,1.,1.,1.,1.,1.,1.,1.,1.,1.,
1.,1.,1.,1.,1.,1.))
REPRESENTATION_ITEM('')
);
#263=(
BOUNDED_CURVE()
B_SPLINE_CURVE(5,(#37911,#37912,#37913,#37914,#37915,#37916,#37917,#37918,
#37919,#37920,#37921,#37922,#37923,#37924,#37925,#37926,#37927,#37928,#37929,
#37930,#37931,#37932,#37933,#37934,#37935,#37936,#37937,#37938,#37939,#37940,
#37941,#37942,#37943,#37944,#37945,#37946,#37947,#37948,#37949,#37950,#37951,
#37952,#37953,#37954,#37955,#37956,#37957,#37958,#37959,#37960,#37961,#37962,
#37963,#37964,#37965,#37966,#37967,#37968,#37969,#37970,#37971,#37972,#37973,
#37974,#37975,#37976,#37977,#37978,#37979,#37980),.UNSPECIFIED.,.F.,.F.)
B_SPLINE_CURVE_WITH_KNOTS((6,1,1,1,1,1,1,1,1,1,1,1,1,1,1,1,1,1,1,1,1,1,
1,1,1,1,1,1,1,1,1,1,1,1,1,1,1,1,1,1,1,1,1,1,1,1,1,1,1,1,1,1,1,1,1,1,1,1,
1,1,1,1,1,1,1,6),(0.00577184337450072,0.0153846153846154,0.0307692307692308,
0.0461538461538462,0.0615384615384615,0.0769230769230769,0.0923076923076923,
0.107692307692308,0.123076923076923,0.138461538461538,0.153846153846154,
0.169230769230769,0.184615384615385,0.2,0.215384615384615,0.230769230769231,
0.246153846153846,0.261538461538462,0.276923076923077,0.292307692307692,
0.307692307692308,0.323076923076923,0.338461538461538,0.353846153846154,
0.369230769230769,0.384615384615385,0.4,0.415384615384615,0.430769230769231,
0.446153846153846,0.461538461538462,0.476923076923077,0.492307692307692,
0.507692307692308,0.523076923076923,0.538461538461538,0.553846153846154,
0.569230769230769,0.584615384615384,0.6,0.615384615384615,0.63076923076923,
0.646153846153846,0.661538461538461,0.676923076923076,0.692307692307692,
0.707692307692307,0.723076923076922,0.738461538461538,0.753846153846153,
0.769230769230768,0.784615384615384,0.799999999999999,0.815384615384614,
0.83076923076923,0.846153846153845,0.86153846153846,0.876923076923076,0.892307692307691,
0.907692307692306,0.923076923076922,0.938461538461537,0.953846153846152,
0.969230769230768,0.984615384615383,1.),.UNSPECIFIED.)
CURVE()
GEOMETRIC_REPRESENTATION_ITEM()
RATIONAL_B_SPLINE_CURVE((1.,1.,1.,1.,1.,1.,1.,1.,1.,1.,1.,1.,1.,1.,1.,1.,
1.,1.,1.,1.,1.,1.,1.,1.,1.,1.,1.,1.,1.,1.,1.,1.,1.,1.,1.,1.,1.,1.,1.,1.,
1.,1.,1.,1.,1.,1.,1.,1.,1.,1.,1.,1.,1.,1.,1.,1.,1.,1.,1.,1.,1.,1.,1.,1.,
1.,1.,1.,1.,1.,1.))
REPRESENTATION_ITEM('')
);
#264=(
BOUNDED_CURVE()
B_SPLINE_CURVE(5,(#37984,#37985,#37986,#37987,#37988,#37989,#37990,#37991,
#37992,#37993,#37994,#37995,#37996,#37997,#37998,#37999,#38000,#38001,#38002,
#38003,#38004,#38005,#38006,#38007,#38008,#38009,#38010,#38011,#38012,#38013,
#38014,#38015,#38016,#38017,#38018,#38019,#38020,#38021,#38022,#38023,#38024,
#38025,#38026,#38027,#38028,#38029,#38030,#38031,#38032,#38033,#38034,#38035,
#38036,#38037,#38038,#38039,#38040,#38041,#38042,#38043,#38044,#38045,#38046,
#38047,#38048,#38049,#38050,#38051,#38052,#38053),.UNSPECIFIED.,.F.,.F.)
B_SPLINE_CURVE_WITH_KNOTS((6,1,1,1,1,1,1,1,1,1,1,1,1,1,1,1,1,1,1,1,1,1,
1,1,1,1,1,1,1,1,1,1,1,1,1,1,1,1,1,1,1,1,1,1,1,1,1,1,1,1,1,1,1,1,1,1,1,1,
1,1,1,1,1,1,1,6),(0.,0.0153846153846154,0.0307692307692308,0.0461538461538462,
0.0615384615384615,0.0769230769230769,0.0923076923076923,0.107692307692308,
0.123076923076923,0.138461538461538,0.153846153846154,0.169230769230769,
0.184615384615385,0.2,0.215384615384615,0.230769230769231,0.246153846153846,
0.261538461538462,0.276923076923077,0.292307692307692,0.307692307692308,
0.323076923076923,0.338461538461538,0.353846153846154,0.369230769230769,
0.384615384615385,0.4,0.415384615384615,0.430769230769231,0.446153846153846,
0.461538461538462,0.476923076923077,0.492307692307692,0.507692307692308,
0.523076923076923,0.538461538461538,0.553846153846154,0.569230769230769,
0.584615384615384,0.6,0.615384615384615,0.63076923076923,0.646153846153846,
0.661538461538461,0.676923076923076,0.692307692307692,0.707692307692307,
0.723076923076922,0.738461538461538,0.753846153846153,0.769230769230768,
0.784615384615384,0.799999999999999,0.815384615384614,0.83076923076923,
0.846153846153845,0.86153846153846,0.876923076923076,0.892307692307691,
0.907692307692306,0.923076923076922,0.938461538461537,0.953846153846152,
0.969230769230768,0.984615384615383,0.994228156739706),.UNSPECIFIED.)
CURVE()
GEOMETRIC_REPRESENTATION_ITEM()
RATIONAL_B_SPLINE_CURVE((1.,1.,1.,1.,1.,1.,1.,1.,1.,1.,1.,1.,1.,1.,1.,1.,
1.,1.,1.,1.,1.,1.,1.,1.,1.,1.,1.,1.,1.,1.,1.,1.,1.,1.,1.,1.,1.,1.,1.,1.,
1.,1.,1.,1.,1.,1.,1.,1.,1.,1.,1.,1.,1.,1.,1.,1.,1.,1.,1.,1.,1.,1.,1.,1.,
1.,1.,1.,1.,1.,1.))
REPRESENTATION_ITEM('')
);
#265=(
BOUNDED_CURVE()
B_SPLINE_CURVE(5,(#38057,#38058,#38059,#38060,#38061,#38062,#38063,#38064,
#38065,#38066,#38067,#38068,#38069,#38070,#38071,#38072,#38073,#38074,#38075,
#38076,#38077,#38078,#38079,#38080,#38081,#38082,#38083,#38084,#38085,#38086,
#38087,#38088,#38089,#38090,#38091,#38092,#38093,#38094,#38095,#38096,#38097,
#38098,#38099,#38100,#38101,#38102,#38103,#38104,#38105,#38106,#38107,#38108,
#38109,#38110,#38111,#38112,#38113,#38114,#38115,#38116,#38117,#38118,#38119,
#38120,#38121,#38122,#38123,#38124,#38125,#38126),.UNSPECIFIED.,.F.,.F.)
B_SPLINE_CURVE_WITH_KNOTS((6,1,1,1,1,1,1,1,1,1,1,1,1,1,1,1,1,1,1,1,1,1,
1,1,1,1,1,1,1,1,1,1,1,1,1,1,1,1,1,1,1,1,1,1,1,1,1,1,1,1,1,1,1,1,1,1,1,1,
1,1,1,1,1,1,1,6),(0.00577184337450902,0.0153846153846154,0.0307692307692308,
0.0461538461538462,0.0615384615384615,0.0769230769230769,0.0923076923076923,
0.107692307692308,0.123076923076923,0.138461538461538,0.153846153846154,
0.169230769230769,0.184615384615385,0.2,0.215384615384615,0.230769230769231,
0.246153846153846,0.261538461538462,0.276923076923077,0.292307692307692,
0.307692307692308,0.323076923076923,0.338461538461538,0.353846153846154,
0.369230769230769,0.384615384615385,0.4,0.415384615384615,0.430769230769231,
0.446153846153846,0.461538461538462,0.476923076923077,0.492307692307692,
0.507692307692308,0.523076923076923,0.538461538461538,0.553846153846154,
0.569230769230769,0.584615384615384,0.6,0.615384615384615,0.63076923076923,
0.646153846153846,0.661538461538461,0.676923076923076,0.692307692307692,
0.707692307692307,0.723076923076922,0.738461538461538,0.753846153846153,
0.769230769230768,0.784615384615384,0.799999999999999,0.815384615384614,
0.83076923076923,0.846153846153845,0.86153846153846,0.876923076923076,0.892307692307691,
0.907692307692306,0.923076923076922,0.938461538461537,0.953846153846152,
0.969230769230768,0.984615384615383,1.),.UNSPECIFIED.)
CURVE()
GEOMETRIC_REPRESENTATION_ITEM()
RATIONAL_B_SPLINE_CURVE((1.,1.,1.,1.,1.,1.,1.,1.,1.,1.,1.,1.,1.,1.,1.,1.,
1.,1.,1.,1.,1.,1.,1.,1.,1.,1.,1.,1.,1.,1.,1.,1.,1.,1.,1.,1.,1.,1.,1.,1.,
1.,1.,1.,1.,1.,1.,1.,1.,1.,1.,1.,1.,1.,1.,1.,1.,1.,1.,1.,1.,1.,1.,1.,1.,
1.,1.,1.,1.,1.,1.))
REPRESENTATION_ITEM('')
);
#266=(
BOUNDED_CURVE()
B_SPLINE_CURVE(5,(#38130,#38131,#38132,#38133,#38134,#38135,#38136,#38137,
#38138,#38139,#38140,#38141,#38142,#38143,#38144,#38145,#38146,#38147,#38148,
#38149,#38150,#38151,#38152,#38153,#38154,#38155,#38156,#38157,#38158,#38159,
#38160,#38161,#38162,#38163,#38164,#38165,#38166,#38167,#38168,#38169,#38170,
#38171,#38172,#38173,#38174,#38175,#38176,#38177,#38178,#38179,#38180,#38181,
#38182,#38183,#38184,#38185,#38186,#38187,#38188,#38189,#38190,#38191,#38192,
#38193,#38194,#38195,#38196,#38197,#38198,#38199),.UNSPECIFIED.,.F.,.F.)
B_SPLINE_CURVE_WITH_KNOTS((6,1,1,1,1,1,1,1,1,1,1,1,1,1,1,1,1,1,1,1,1,1,
1,1,1,1,1,1,1,1,1,1,1,1,1,1,1,1,1,1,1,1,1,1,1,1,1,1,1,1,1,1,1,1,1,1,1,1,
1,1,1,1,1,1,1,6),(0.,0.0153846153846154,0.0307692307692308,0.0461538461538462,
0.0615384615384615,0.0769230769230769,0.0923076923076923,0.107692307692308,
0.123076923076923,0.138461538461538,0.153846153846154,0.169230769230769,
0.184615384615385,0.2,0.215384615384615,0.230769230769231,0.246153846153846,
0.261538461538462,0.276923076923077,0.292307692307692,0.307692307692308,
0.323076923076923,0.338461538461538,0.353846153846154,0.369230769230769,
0.384615384615385,0.4,0.415384615384615,0.430769230769231,0.446153846153846,
0.461538461538462,0.476923076923077,0.492307692307692,0.507692307692308,
0.523076923076923,0.538461538461538,0.553846153846154,0.569230769230769,
0.584615384615384,0.6,0.615384615384615,0.63076923076923,0.646153846153846,
0.661538461538461,0.676923076923076,0.692307692307692,0.707692307692307,
0.723076923076922,0.738461538461538,0.753846153846153,0.769230769230768,
0.784615384615384,0.799999999999999,0.815384615384614,0.83076923076923,
0.846153846153845,0.86153846153846,0.876923076923076,0.892307692307691,
0.907692307692306,0.923076923076922,0.938461538461537,0.953846153846152,
0.969230769230768,0.984615384615383,0.994228156739698),.UNSPECIFIED.)
CURVE()
GEOMETRIC_REPRESENTATION_ITEM()
RATIONAL_B_SPLINE_CURVE((1.,1.,1.,1.,1.,1.,1.,1.,1.,1.,1.,1.,1.,1.,1.,1.,
1.,1.,1.,1.,1.,1.,1.,1.,1.,1.,1.,1.,1.,1.,1.,1.,1.,1.,1.,1.,1.,1.,1.,1.,
1.,1.,1.,1.,1.,1.,1.,1.,1.,1.,1.,1.,1.,1.,1.,1.,1.,1.,1.,1.,1.,1.,1.,1.,
1.,1.,1.,1.,1.,1.))
REPRESENTATION_ITEM('')
);
#267=(
BOUNDED_CURVE()
B_SPLINE_CURVE(5,(#38203,#38204,#38205,#38206,#38207,#38208,#38209,#38210,
#38211,#38212,#38213,#38214,#38215,#38216,#38217,#38218,#38219,#38220,#38221,
#38222,#38223,#38224,#38225,#38226,#38227,#38228,#38229,#38230,#38231,#38232,
#38233,#38234,#38235,#38236,#38237,#38238,#38239,#38240,#38241,#38242,#38243,
#38244,#38245,#38246,#38247,#38248,#38249,#38250,#38251,#38252,#38253,#38254,
#38255,#38256,#38257,#38258,#38259,#38260,#38261,#38262,#38263,#38264,#38265,
#38266,#38267,#38268,#38269,#38270,#38271,#38272),.UNSPECIFIED.,.F.,.F.)
B_SPLINE_CURVE_WITH_KNOTS((6,1,1,1,1,1,1,1,1,1,1,1,1,1,1,1,1,1,1,1,1,1,
1,1,1,1,1,1,1,1,1,1,1,1,1,1,1,1,1,1,1,1,1,1,1,1,1,1,1,1,1,1,1,1,1,1,1,1,
1,1,1,1,1,1,1,6),(0.00577184337451611,0.0153846153846154,0.0307692307692308,
0.0461538461538462,0.0615384615384615,0.0769230769230769,0.0923076923076923,
0.107692307692308,0.123076923076923,0.138461538461538,0.153846153846154,
0.169230769230769,0.184615384615385,0.2,0.215384615384615,0.230769230769231,
0.246153846153846,0.261538461538462,0.276923076923077,0.292307692307692,
0.307692307692308,0.323076923076923,0.338461538461538,0.353846153846154,
0.369230769230769,0.384615384615385,0.4,0.415384615384615,0.430769230769231,
0.446153846153846,0.461538461538462,0.476923076923077,0.492307692307692,
0.507692307692308,0.523076923076923,0.538461538461538,0.553846153846154,
0.569230769230769,0.584615384615384,0.6,0.615384615384615,0.63076923076923,
0.646153846153846,0.661538461538461,0.676923076923076,0.692307692307692,
0.707692307692307,0.723076923076922,0.738461538461538,0.753846153846153,
0.769230769230768,0.784615384615384,0.799999999999999,0.815384615384614,
0.83076923076923,0.846153846153845,0.86153846153846,0.876923076923076,0.892307692307691,
0.907692307692306,0.923076923076922,0.938461538461537,0.953846153846152,
0.969230769230768,0.984615384615383,1.),.UNSPECIFIED.)
CURVE()
GEOMETRIC_REPRESENTATION_ITEM()
RATIONAL_B_SPLINE_CURVE((1.,1.,1.,1.,1.,1.,1.,1.,1.,1.,1.,1.,1.,1.,1.,1.,
1.,1.,1.,1.,1.,1.,1.,1.,1.,1.,1.,1.,1.,1.,1.,1.,1.,1.,1.,1.,1.,1.,1.,1.,
1.,1.,1.,1.,1.,1.,1.,1.,1.,1.,1.,1.,1.,1.,1.,1.,1.,1.,1.,1.,1.,1.,1.,1.,
1.,1.,1.,1.,1.,1.))
REPRESENTATION_ITEM('')
);
#268=(
BOUNDED_CURVE()
B_SPLINE_CURVE(5,(#38276,#38277,#38278,#38279,#38280,#38281,#38282,#38283,
#38284,#38285,#38286,#38287,#38288,#38289,#38290,#38291,#38292,#38293,#38294,
#38295,#38296,#38297,#38298,#38299,#38300,#38301,#38302,#38303,#38304,#38305,
#38306,#38307,#38308,#38309,#38310,#38311,#38312,#38313,#38314,#38315,#38316,
#38317,#38318,#38319,#38320,#38321,#38322,#38323,#38324,#38325,#38326,#38327,
#38328,#38329,#38330,#38331,#38332,#38333,#38334,#38335,#38336,#38337,#38338,
#38339,#38340,#38341,#38342,#38343,#38344,#38345),.UNSPECIFIED.,.F.,.F.)
B_SPLINE_CURVE_WITH_KNOTS((6,1,1,1,1,1,1,1,1,1,1,1,1,1,1,1,1,1,1,1,1,1,
1,1,1,1,1,1,1,1,1,1,1,1,1,1,1,1,1,1,1,1,1,1,1,1,1,1,1,1,1,1,1,1,1,1,1,1,
1,1,1,1,1,1,1,6),(0.,0.0153846153846154,0.0307692307692308,0.0461538461538462,
0.0615384615384615,0.0769230769230769,0.0923076923076923,0.107692307692308,
0.123076923076923,0.138461538461538,0.153846153846154,0.169230769230769,
0.184615384615385,0.2,0.215384615384615,0.230769230769231,0.246153846153846,
0.261538461538462,0.276923076923077,0.292307692307692,0.307692307692308,
0.323076923076923,0.338461538461538,0.353846153846154,0.369230769230769,
0.384615384615385,0.4,0.415384615384615,0.430769230769231,0.446153846153846,
0.461538461538462,0.476923076923077,0.492307692307692,0.507692307692308,
0.523076923076923,0.538461538461538,0.553846153846154,0.569230769230769,
0.584615384615384,0.6,0.615384615384615,0.63076923076923,0.646153846153846,
0.661538461538461,0.676923076923076,0.692307692307692,0.707692307692307,
0.723076923076922,0.738461538461538,0.753846153846153,0.769230769230768,
0.784615384615384,0.799999999999999,0.815384615384614,0.83076923076923,
0.846153846153845,0.86153846153846,0.876923076923076,0.892307692307691,
0.907692307692306,0.923076923076922,0.938461538461537,0.953846153846152,
0.969230769230768,0.984615384615383,0.994228156739704),.UNSPECIFIED.)
CURVE()
GEOMETRIC_REPRESENTATION_ITEM()
RATIONAL_B_SPLINE_CURVE((1.,1.,1.,1.,1.,1.,1.,1.,1.,1.,1.,1.,1.,1.,1.,1.,
1.,1.,1.,1.,1.,1.,1.,1.,1.,1.,1.,1.,1.,1.,1.,1.,1.,1.,1.,1.,1.,1.,1.,1.,
1.,1.,1.,1.,1.,1.,1.,1.,1.,1.,1.,1.,1.,1.,1.,1.,1.,1.,1.,1.,1.,1.,1.,1.,
1.,1.,1.,1.,1.,1.))
REPRESENTATION_ITEM('')
);
#269=(
BOUNDED_CURVE()
B_SPLINE_CURVE(5,(#38349,#38350,#38351,#38352,#38353,#38354,#38355,#38356,
#38357,#38358,#38359,#38360,#38361,#38362,#38363,#38364,#38365,#38366,#38367,
#38368,#38369,#38370,#38371,#38372,#38373,#38374,#38375,#38376,#38377,#38378,
#38379,#38380,#38381,#38382,#38383,#38384,#38385,#38386,#38387,#38388,#38389,
#38390,#38391,#38392,#38393,#38394,#38395,#38396,#38397,#38398,#38399,#38400,
#38401,#38402,#38403,#38404,#38405,#38406,#38407,#38408,#38409,#38410,#38411,
#38412,#38413,#38414,#38415,#38416,#38417,#38418),.UNSPECIFIED.,.F.,.F.)
B_SPLINE_CURVE_WITH_KNOTS((6,1,1,1,1,1,1,1,1,1,1,1,1,1,1,1,1,1,1,1,1,1,
1,1,1,1,1,1,1,1,1,1,1,1,1,1,1,1,1,1,1,1,1,1,1,1,1,1,1,1,1,1,1,1,1,1,1,1,
1,1,1,1,1,1,1,6),(0.00577184337449682,0.0153846153846154,0.0307692307692308,
0.0461538461538462,0.0615384615384615,0.0769230769230769,0.0923076923076923,
0.107692307692308,0.123076923076923,0.138461538461538,0.153846153846154,
0.169230769230769,0.184615384615385,0.2,0.215384615384615,0.230769230769231,
0.246153846153846,0.261538461538462,0.276923076923077,0.292307692307692,
0.307692307692308,0.323076923076923,0.338461538461538,0.353846153846154,
0.369230769230769,0.384615384615385,0.4,0.415384615384615,0.430769230769231,
0.446153846153846,0.461538461538462,0.476923076923077,0.492307692307692,
0.507692307692308,0.523076923076923,0.538461538461538,0.553846153846154,
0.569230769230769,0.584615384615384,0.6,0.615384615384615,0.63076923076923,
0.646153846153846,0.661538461538461,0.676923076923076,0.692307692307692,
0.707692307692307,0.723076923076922,0.738461538461538,0.753846153846153,
0.769230769230768,0.784615384615384,0.799999999999999,0.815384615384614,
0.83076923076923,0.846153846153845,0.86153846153846,0.876923076923076,0.892307692307691,
0.907692307692306,0.923076923076922,0.938461538461537,0.953846153846152,
0.969230769230768,0.984615384615383,1.),.UNSPECIFIED.)
CURVE()
GEOMETRIC_REPRESENTATION_ITEM()
RATIONAL_B_SPLINE_CURVE((1.,1.,1.,1.,1.,1.,1.,1.,1.,1.,1.,1.,1.,1.,1.,1.,
1.,1.,1.,1.,1.,1.,1.,1.,1.,1.,1.,1.,1.,1.,1.,1.,1.,1.,1.,1.,1.,1.,1.,1.,
1.,1.,1.,1.,1.,1.,1.,1.,1.,1.,1.,1.,1.,1.,1.,1.,1.,1.,1.,1.,1.,1.,1.,1.,
1.,1.,1.,1.,1.,1.))
REPRESENTATION_ITEM('')
);
#270=(
BOUNDED_CURVE()
B_SPLINE_CURVE(5,(#38422,#38423,#38424,#38425,#38426,#38427,#38428,#38429,
#38430,#38431,#38432,#38433,#38434,#38435,#38436,#38437,#38438,#38439,#38440,
#38441,#38442,#38443,#38444,#38445,#38446,#38447,#38448,#38449,#38450,#38451,
#38452,#38453,#38454,#38455,#38456,#38457,#38458,#38459,#38460,#38461,#38462,
#38463,#38464,#38465,#38466,#38467,#38468,#38469,#38470,#38471,#38472,#38473,
#38474,#38475,#38476,#38477,#38478,#38479,#38480,#38481,#38482,#38483,#38484,
#38485,#38486,#38487,#38488,#38489,#38490,#38491),.UNSPECIFIED.,.F.,.F.)
B_SPLINE_CURVE_WITH_KNOTS((6,1,1,1,1,1,1,1,1,1,1,1,1,1,1,1,1,1,1,1,1,1,
1,1,1,1,1,1,1,1,1,1,1,1,1,1,1,1,1,1,1,1,1,1,1,1,1,1,1,1,1,1,1,1,1,1,1,1,
1,1,1,1,1,1,1,6),(0.,0.0153846153846154,0.0307692307692308,0.0461538461538462,
0.0615384615384615,0.0769230769230769,0.0923076923076923,0.107692307692308,
0.123076923076923,0.138461538461538,0.153846153846154,0.169230769230769,
0.184615384615385,0.2,0.215384615384615,0.230769230769231,0.246153846153846,
0.261538461538462,0.276923076923077,0.292307692307692,0.307692307692308,
0.323076923076923,0.338461538461538,0.353846153846154,0.369230769230769,
0.384615384615385,0.4,0.415384615384615,0.430769230769231,0.446153846153846,
0.461538461538462,0.476923076923077,0.492307692307692,0.507692307692308,
0.523076923076923,0.538461538461538,0.553846153846154,0.569230769230769,
0.584615384615384,0.6,0.615384615384615,0.63076923076923,0.646153846153846,
0.661538461538461,0.676923076923076,0.692307692307692,0.707692307692307,
0.723076923076922,0.738461538461538,0.753846153846153,0.769230769230768,
0.784615384615384,0.799999999999999,0.815384615384614,0.83076923076923,
0.846153846153845,0.86153846153846,0.876923076923076,0.892307692307691,
0.907692307692306,0.923076923076922,0.938461538461537,0.953846153846152,
0.969230769230768,0.984615384615383,0.994228156739711),.UNSPECIFIED.)
CURVE()
GEOMETRIC_REPRESENTATION_ITEM()
RATIONAL_B_SPLINE_CURVE((1.,1.,1.,1.,1.,1.,1.,1.,1.,1.,1.,1.,1.,1.,1.,1.,
1.,1.,1.,1.,1.,1.,1.,1.,1.,1.,1.,1.,1.,1.,1.,1.,1.,1.,1.,1.,1.,1.,1.,1.,
1.,1.,1.,1.,1.,1.,1.,1.,1.,1.,1.,1.,1.,1.,1.,1.,1.,1.,1.,1.,1.,1.,1.,1.,
1.,1.,1.,1.,1.,1.))
REPRESENTATION_ITEM('')
);
#271=(
BOUNDED_CURVE()
B_SPLINE_CURVE(5,(#38495,#38496,#38497,#38498,#38499,#38500,#38501,#38502,
#38503,#38504,#38505,#38506,#38507,#38508,#38509,#38510,#38511,#38512,#38513,
#38514,#38515,#38516,#38517,#38518,#38519,#38520,#38521,#38522,#38523,#38524,
#38525,#38526,#38527,#38528,#38529,#38530,#38531,#38532,#38533,#38534,#38535,
#38536,#38537,#38538,#38539,#38540,#38541,#38542,#38543,#38544,#38545,#38546,
#38547,#38548,#38549,#38550,#38551,#38552,#38553,#38554,#38555,#38556,#38557,
#38558,#38559,#38560,#38561,#38562,#38563,#38564),.UNSPECIFIED.,.F.,.F.)
B_SPLINE_CURVE_WITH_KNOTS((6,1,1,1,1,1,1,1,1,1,1,1,1,1,1,1,1,1,1,1,1,1,
1,1,1,1,1,1,1,1,1,1,1,1,1,1,1,1,1,1,1,1,1,1,1,1,1,1,1,1,1,1,1,1,1,1,1,1,
1,1,1,1,1,1,1,6),(0.00577184337449159,0.0153846153846154,0.0307692307692308,
0.0461538461538462,0.0615384615384615,0.0769230769230769,0.0923076923076923,
0.107692307692308,0.123076923076923,0.138461538461538,0.153846153846154,
0.169230769230769,0.184615384615385,0.2,0.215384615384615,0.230769230769231,
0.246153846153846,0.261538461538462,0.276923076923077,0.292307692307692,
0.307692307692308,0.323076923076923,0.338461538461538,0.353846153846154,
0.369230769230769,0.384615384615385,0.4,0.415384615384615,0.430769230769231,
0.446153846153846,0.461538461538462,0.476923076923077,0.492307692307692,
0.507692307692308,0.523076923076923,0.538461538461538,0.553846153846154,
0.569230769230769,0.584615384615384,0.6,0.615384615384615,0.63076923076923,
0.646153846153846,0.661538461538461,0.676923076923076,0.692307692307692,
0.707692307692307,0.723076923076922,0.738461538461538,0.753846153846153,
0.769230769230768,0.784615384615384,0.799999999999999,0.815384615384614,
0.83076923076923,0.846153846153845,0.86153846153846,0.876923076923076,0.892307692307691,
0.907692307692306,0.923076923076922,0.938461538461537,0.953846153846152,
0.969230769230768,0.984615384615383,1.),.UNSPECIFIED.)
CURVE()
GEOMETRIC_REPRESENTATION_ITEM()
RATIONAL_B_SPLINE_CURVE((1.,1.,1.,1.,1.,1.,1.,1.,1.,1.,1.,1.,1.,1.,1.,1.,
1.,1.,1.,1.,1.,1.,1.,1.,1.,1.,1.,1.,1.,1.,1.,1.,1.,1.,1.,1.,1.,1.,1.,1.,
1.,1.,1.,1.,1.,1.,1.,1.,1.,1.,1.,1.,1.,1.,1.,1.,1.,1.,1.,1.,1.,1.,1.,1.,
1.,1.,1.,1.,1.,1.))
REPRESENTATION_ITEM('')
);
#272=(
BOUNDED_CURVE()
B_SPLINE_CURVE(5,(#38568,#38569,#38570,#38571,#38572,#38573,#38574,#38575,
#38576,#38577,#38578,#38579,#38580,#38581,#38582,#38583,#38584,#38585,#38586,
#38587,#38588,#38589,#38590,#38591,#38592,#38593,#38594,#38595,#38596,#38597,
#38598,#38599,#38600,#38601,#38602,#38603,#38604,#38605,#38606,#38607,#38608,
#38609,#38610,#38611,#38612,#38613,#38614,#38615,#38616,#38617,#38618,#38619,
#38620,#38621,#38622,#38623,#38624,#38625,#38626,#38627,#38628,#38629,#38630,
#38631,#38632,#38633,#38634,#38635,#38636,#38637),.UNSPECIFIED.,.F.,.F.)
B_SPLINE_CURVE_WITH_KNOTS((6,1,1,1,1,1,1,1,1,1,1,1,1,1,1,1,1,1,1,1,1,1,
1,1,1,1,1,1,1,1,1,1,1,1,1,1,1,1,1,1,1,1,1,1,1,1,1,1,1,1,1,1,1,1,1,1,1,1,
1,1,1,1,1,1,1,6),(0.,0.0153846153846154,0.0307692307692308,0.0461538461538462,
0.0615384615384615,0.0769230769230769,0.0923076923076923,0.107692307692308,
0.123076923076923,0.138461538461538,0.153846153846154,0.169230769230769,
0.184615384615385,0.2,0.215384615384615,0.230769230769231,0.246153846153846,
0.261538461538462,0.276923076923077,0.292307692307692,0.307692307692308,
0.323076923076923,0.338461538461538,0.353846153846154,0.369230769230769,
0.384615384615385,0.4,0.415384615384615,0.430769230769231,0.446153846153846,
0.461538461538462,0.476923076923077,0.492307692307692,0.507692307692308,
0.523076923076923,0.538461538461538,0.553846153846154,0.569230769230769,
0.584615384615384,0.6,0.615384615384615,0.63076923076923,0.646153846153846,
0.661538461538461,0.676923076923076,0.692307692307692,0.707692307692307,
0.723076923076922,0.738461538461538,0.753846153846153,0.769230769230768,
0.784615384615384,0.799999999999999,0.815384615384614,0.83076923076923,
0.846153846153845,0.86153846153846,0.876923076923076,0.892307692307691,
0.907692307692306,0.923076923076922,0.938461538461537,0.953846153846152,
0.969230769230768,0.984615384615383,0.994228156739723),.UNSPECIFIED.)
CURVE()
GEOMETRIC_REPRESENTATION_ITEM()
RATIONAL_B_SPLINE_CURVE((1.,1.,1.,1.,1.,1.,1.,1.,1.,1.,1.,1.,1.,1.,1.,1.,
1.,1.,1.,1.,1.,1.,1.,1.,1.,1.,1.,1.,1.,1.,1.,1.,1.,1.,1.,1.,1.,1.,1.,1.,
1.,1.,1.,1.,1.,1.,1.,1.,1.,1.,1.,1.,1.,1.,1.,1.,1.,1.,1.,1.,1.,1.,1.,1.,
1.,1.,1.,1.,1.,1.))
REPRESENTATION_ITEM('')
);
#273=(
BOUNDED_CURVE()
B_SPLINE_CURVE(5,(#38641,#38642,#38643,#38644,#38645,#38646,#38647,#38648,
#38649,#38650,#38651,#38652,#38653,#38654,#38655,#38656,#38657,#38658,#38659,
#38660,#38661,#38662,#38663,#38664,#38665,#38666,#38667,#38668,#38669,#38670,
#38671,#38672,#38673,#38674,#38675,#38676,#38677,#38678,#38679,#38680,#38681,
#38682,#38683,#38684,#38685,#38686,#38687,#38688,#38689,#38690,#38691,#38692,
#38693,#38694,#38695,#38696,#38697,#38698,#38699,#38700,#38701,#38702,#38703,
#38704,#38705,#38706,#38707,#38708,#38709,#38710),.UNSPECIFIED.,.F.,.F.)
B_SPLINE_CURVE_WITH_KNOTS((6,1,1,1,1,1,1,1,1,1,1,1,1,1,1,1,1,1,1,1,1,1,
1,1,1,1,1,1,1,1,1,1,1,1,1,1,1,1,1,1,1,1,1,1,1,1,1,1,1,1,1,1,1,1,1,1,1,1,
1,1,1,1,1,1,1,6),(0.00577184337450718,0.0153846153846154,0.0307692307692308,
0.0461538461538462,0.0615384615384615,0.0769230769230769,0.0923076923076923,
0.107692307692308,0.123076923076923,0.138461538461538,0.153846153846154,
0.169230769230769,0.184615384615385,0.2,0.215384615384615,0.230769230769231,
0.246153846153846,0.261538461538462,0.276923076923077,0.292307692307692,
0.307692307692308,0.323076923076923,0.338461538461538,0.353846153846154,
0.369230769230769,0.384615384615385,0.4,0.415384615384615,0.430769230769231,
0.446153846153846,0.461538461538462,0.476923076923077,0.492307692307692,
0.507692307692308,0.523076923076923,0.538461538461538,0.553846153846154,
0.569230769230769,0.584615384615384,0.6,0.615384615384615,0.63076923076923,
0.646153846153846,0.661538461538461,0.676923076923076,0.692307692307692,
0.707692307692307,0.723076923076922,0.738461538461538,0.753846153846153,
0.769230769230768,0.784615384615384,0.799999999999999,0.815384615384614,
0.83076923076923,0.846153846153845,0.86153846153846,0.876923076923076,0.892307692307691,
0.907692307692306,0.923076923076922,0.938461538461537,0.953846153846152,
0.969230769230768,0.984615384615383,1.),.UNSPECIFIED.)
CURVE()
GEOMETRIC_REPRESENTATION_ITEM()
RATIONAL_B_SPLINE_CURVE((1.,1.,1.,1.,1.,1.,1.,1.,1.,1.,1.,1.,1.,1.,1.,1.,
1.,1.,1.,1.,1.,1.,1.,1.,1.,1.,1.,1.,1.,1.,1.,1.,1.,1.,1.,1.,1.,1.,1.,1.,
1.,1.,1.,1.,1.,1.,1.,1.,1.,1.,1.,1.,1.,1.,1.,1.,1.,1.,1.,1.,1.,1.,1.,1.,
1.,1.,1.,1.,1.,1.))
REPRESENTATION_ITEM('')
);
#274=(
BOUNDED_CURVE()
B_SPLINE_CURVE(5,(#38714,#38715,#38716,#38717,#38718,#38719,#38720,#38721,
#38722,#38723,#38724,#38725,#38726,#38727,#38728,#38729,#38730,#38731,#38732,
#38733,#38734,#38735,#38736,#38737,#38738,#38739,#38740,#38741,#38742,#38743,
#38744,#38745,#38746,#38747,#38748,#38749,#38750,#38751,#38752,#38753,#38754,
#38755,#38756,#38757,#38758,#38759,#38760,#38761,#38762,#38763,#38764,#38765,
#38766,#38767,#38768,#38769,#38770,#38771,#38772,#38773,#38774,#38775,#38776,
#38777,#38778,#38779,#38780,#38781,#38782,#38783),.UNSPECIFIED.,.F.,.F.)
B_SPLINE_CURVE_WITH_KNOTS((6,1,1,1,1,1,1,1,1,1,1,1,1,1,1,1,1,1,1,1,1,1,
1,1,1,1,1,1,1,1,1,1,1,1,1,1,1,1,1,1,1,1,1,1,1,1,1,1,1,1,1,1,1,1,1,1,1,1,
1,1,1,1,1,1,1,6),(0.,0.0153846153846154,0.0307692307692308,0.0461538461538462,
0.0615384615384615,0.0769230769230769,0.0923076923076923,0.107692307692308,
0.123076923076923,0.138461538461538,0.153846153846154,0.169230769230769,
0.184615384615385,0.2,0.215384615384615,0.230769230769231,0.246153846153846,
0.261538461538462,0.276923076923077,0.292307692307692,0.307692307692308,
0.323076923076923,0.338461538461538,0.353846153846154,0.369230769230769,
0.384615384615385,0.4,0.415384615384615,0.430769230769231,0.446153846153846,
0.461538461538462,0.476923076923077,0.492307692307692,0.507692307692308,
0.523076923076923,0.538461538461538,0.553846153846154,0.569230769230769,
0.584615384615384,0.6,0.615384615384615,0.63076923076923,0.646153846153846,
0.661538461538461,0.676923076923076,0.692307692307692,0.707692307692307,
0.723076923076922,0.738461538461538,0.753846153846153,0.769230769230768,
0.784615384615384,0.799999999999999,0.815384615384614,0.83076923076923,
0.846153846153845,0.86153846153846,0.876923076923076,0.892307692307691,
0.907692307692306,0.923076923076922,0.938461538461537,0.953846153846152,
0.969230769230768,0.984615384615383,0.994228156739716),.UNSPECIFIED.)
CURVE()
GEOMETRIC_REPRESENTATION_ITEM()
RATIONAL_B_SPLINE_CURVE((1.,1.,1.,1.,1.,1.,1.,1.,1.,1.,1.,1.,1.,1.,1.,1.,
1.,1.,1.,1.,1.,1.,1.,1.,1.,1.,1.,1.,1.,1.,1.,1.,1.,1.,1.,1.,1.,1.,1.,1.,
1.,1.,1.,1.,1.,1.,1.,1.,1.,1.,1.,1.,1.,1.,1.,1.,1.,1.,1.,1.,1.,1.,1.,1.,
1.,1.,1.,1.,1.,1.))
REPRESENTATION_ITEM('')
);
#275=(
BOUNDED_CURVE()
B_SPLINE_CURVE(5,(#38787,#38788,#38789,#38790,#38791,#38792,#38793,#38794,
#38795,#38796,#38797,#38798,#38799,#38800,#38801,#38802,#38803,#38804,#38805,
#38806,#38807,#38808,#38809,#38810,#38811,#38812,#38813,#38814,#38815,#38816,
#38817,#38818,#38819,#38820,#38821,#38822,#38823,#38824,#38825,#38826,#38827,
#38828,#38829,#38830,#38831,#38832,#38833,#38834,#38835,#38836,#38837,#38838,
#38839,#38840,#38841,#38842,#38843,#38844,#38845,#38846,#38847,#38848,#38849,
#38850,#38851,#38852,#38853,#38854,#38855,#38856),.UNSPECIFIED.,.F.,.F.)
B_SPLINE_CURVE_WITH_KNOTS((6,1,1,1,1,1,1,1,1,1,1,1,1,1,1,1,1,1,1,1,1,1,
1,1,1,1,1,1,1,1,1,1,1,1,1,1,1,1,1,1,1,1,1,1,1,1,1,1,1,1,1,1,1,1,1,1,1,1,
1,1,1,1,1,1,1,6),(0.00577184337450174,0.0153846153846154,0.0307692307692308,
0.0461538461538462,0.0615384615384615,0.0769230769230769,0.0923076923076923,
0.107692307692308,0.123076923076923,0.138461538461538,0.153846153846154,
0.169230769230769,0.184615384615385,0.2,0.215384615384615,0.230769230769231,
0.246153846153846,0.261538461538462,0.276923076923077,0.292307692307692,
0.307692307692308,0.323076923076923,0.338461538461538,0.353846153846154,
0.369230769230769,0.384615384615385,0.4,0.415384615384615,0.430769230769231,
0.446153846153846,0.461538461538462,0.476923076923077,0.492307692307692,
0.507692307692308,0.523076923076923,0.538461538461538,0.553846153846154,
0.569230769230769,0.584615384615384,0.6,0.615384615384615,0.63076923076923,
0.646153846153846,0.661538461538461,0.676923076923076,0.692307692307692,
0.707692307692307,0.723076923076922,0.738461538461538,0.753846153846153,
0.769230769230768,0.784615384615384,0.799999999999999,0.815384615384614,
0.83076923076923,0.846153846153845,0.86153846153846,0.876923076923076,0.892307692307691,
0.907692307692306,0.923076923076922,0.938461538461537,0.953846153846152,
0.969230769230768,0.984615384615383,1.),.UNSPECIFIED.)
CURVE()
GEOMETRIC_REPRESENTATION_ITEM()
RATIONAL_B_SPLINE_CURVE((1.,1.,1.,1.,1.,1.,1.,1.,1.,1.,1.,1.,1.,1.,1.,1.,
1.,1.,1.,1.,1.,1.,1.,1.,1.,1.,1.,1.,1.,1.,1.,1.,1.,1.,1.,1.,1.,1.,1.,1.,
1.,1.,1.,1.,1.,1.,1.,1.,1.,1.,1.,1.,1.,1.,1.,1.,1.,1.,1.,1.,1.,1.,1.,1.,
1.,1.,1.,1.,1.,1.))
REPRESENTATION_ITEM('')
);
#276=(
BOUNDED_CURVE()
B_SPLINE_CURVE(5,(#38860,#38861,#38862,#38863,#38864,#38865,#38866,#38867,
#38868,#38869,#38870,#38871,#38872,#38873,#38874,#38875,#38876,#38877,#38878,
#38879,#38880,#38881,#38882,#38883,#38884,#38885,#38886,#38887,#38888,#38889,
#38890,#38891,#38892,#38893,#38894,#38895,#38896,#38897,#38898,#38899,#38900,
#38901,#38902,#38903,#38904,#38905,#38906,#38907,#38908,#38909,#38910,#38911,
#38912,#38913,#38914,#38915,#38916,#38917,#38918,#38919,#38920,#38921,#38922,
#38923,#38924,#38925,#38926,#38927,#38928,#38929),.UNSPECIFIED.,.F.,.F.)
B_SPLINE_CURVE_WITH_KNOTS((6,1,1,1,1,1,1,1,1,1,1,1,1,1,1,1,1,1,1,1,1,1,
1,1,1,1,1,1,1,1,1,1,1,1,1,1,1,1,1,1,1,1,1,1,1,1,1,1,1,1,1,1,1,1,1,1,1,1,
1,1,1,1,1,1,1,6),(0.,0.0153846153846154,0.0307692307692308,0.0461538461538462,
0.0615384615384615,0.0769230769230769,0.0923076923076923,0.107692307692308,
0.123076923076923,0.138461538461538,0.153846153846154,0.169230769230769,
0.184615384615385,0.2,0.215384615384615,0.230769230769231,0.246153846153846,
0.261538461538462,0.276923076923077,0.292307692307692,0.307692307692308,
0.323076923076923,0.338461538461538,0.353846153846154,0.369230769230769,
0.384615384615385,0.4,0.415384615384615,0.430769230769231,0.446153846153846,
0.461538461538462,0.476923076923077,0.492307692307692,0.507692307692308,
0.523076923076923,0.538461538461538,0.553846153846154,0.569230769230769,
0.584615384615384,0.6,0.615384615384615,0.63076923076923,0.646153846153846,
0.661538461538461,0.676923076923076,0.692307692307692,0.707692307692307,
0.723076923076922,0.738461538461538,0.753846153846153,0.769230769230768,
0.784615384615384,0.799999999999999,0.815384615384614,0.83076923076923,
0.846153846153845,0.86153846153846,0.876923076923076,0.892307692307691,
0.907692307692306,0.923076923076922,0.938461538461537,0.953846153846152,
0.969230769230768,0.984615384615383,0.994228156739722),.UNSPECIFIED.)
CURVE()
GEOMETRIC_REPRESENTATION_ITEM()
RATIONAL_B_SPLINE_CURVE((1.,1.,1.,1.,1.,1.,1.,1.,1.,1.,1.,1.,1.,1.,1.,1.,
1.,1.,1.,1.,1.,1.,1.,1.,1.,1.,1.,1.,1.,1.,1.,1.,1.,1.,1.,1.,1.,1.,1.,1.,
1.,1.,1.,1.,1.,1.,1.,1.,1.,1.,1.,1.,1.,1.,1.,1.,1.,1.,1.,1.,1.,1.,1.,1.,
1.,1.,1.,1.,1.,1.))
REPRESENTATION_ITEM('')
);
#277=(
BOUNDED_CURVE()
B_SPLINE_CURVE(5,(#38933,#38934,#38935,#38936,#38937,#38938,#38939,#38940,
#38941,#38942,#38943,#38944,#38945,#38946,#38947,#38948,#38949,#38950,#38951,
#38952,#38953,#38954,#38955,#38956,#38957,#38958,#38959,#38960,#38961,#38962,
#38963,#38964,#38965,#38966,#38967,#38968,#38969,#38970,#38971,#38972,#38973,
#38974,#38975,#38976,#38977,#38978,#38979,#38980,#38981,#38982,#38983,#38984,
#38985,#38986,#38987,#38988,#38989,#38990,#38991,#38992,#38993,#38994,#38995,
#38996,#38997,#38998,#38999,#39000,#39001,#39002),.UNSPECIFIED.,.F.,.F.)
B_SPLINE_CURVE_WITH_KNOTS((6,1,1,1,1,1,1,1,1,1,1,1,1,1,1,1,1,1,1,1,1,1,
1,1,1,1,1,1,1,1,1,1,1,1,1,1,1,1,1,1,1,1,1,1,1,1,1,1,1,1,1,1,1,1,1,1,1,1,
1,1,1,1,1,1,1,6),(0.00577184337450943,0.0153846153846154,0.0307692307692308,
0.0461538461538462,0.0615384615384615,0.0769230769230769,0.0923076923076923,
0.107692307692308,0.123076923076923,0.138461538461538,0.153846153846154,
0.169230769230769,0.184615384615385,0.2,0.215384615384615,0.230769230769231,
0.246153846153846,0.261538461538462,0.276923076923077,0.292307692307692,
0.307692307692308,0.323076923076923,0.338461538461538,0.353846153846154,
0.369230769230769,0.384615384615385,0.4,0.415384615384615,0.430769230769231,
0.446153846153846,0.461538461538462,0.476923076923077,0.492307692307692,
0.507692307692308,0.523076923076923,0.538461538461538,0.553846153846154,
0.569230769230769,0.584615384615384,0.6,0.615384615384615,0.63076923076923,
0.646153846153846,0.661538461538461,0.676923076923076,0.692307692307692,
0.707692307692307,0.723076923076922,0.738461538461538,0.753846153846153,
0.769230769230768,0.784615384615384,0.799999999999999,0.815384615384614,
0.83076923076923,0.846153846153845,0.86153846153846,0.876923076923076,0.892307692307691,
0.907692307692306,0.923076923076922,0.938461538461537,0.953846153846152,
0.969230769230768,0.984615384615383,1.),.UNSPECIFIED.)
CURVE()
GEOMETRIC_REPRESENTATION_ITEM()
RATIONAL_B_SPLINE_CURVE((1.,1.,1.,1.,1.,1.,1.,1.,1.,1.,1.,1.,1.,1.,1.,1.,
1.,1.,1.,1.,1.,1.,1.,1.,1.,1.,1.,1.,1.,1.,1.,1.,1.,1.,1.,1.,1.,1.,1.,1.,
1.,1.,1.,1.,1.,1.,1.,1.,1.,1.,1.,1.,1.,1.,1.,1.,1.,1.,1.,1.,1.,1.,1.,1.,
1.,1.,1.,1.,1.,1.))
REPRESENTATION_ITEM('')
);
#278=(
BOUNDED_CURVE()
B_SPLINE_CURVE(5,(#39006,#39007,#39008,#39009,#39010,#39011,#39012,#39013,
#39014,#39015,#39016,#39017,#39018,#39019,#39020,#39021,#39022,#39023,#39024,
#39025,#39026,#39027,#39028,#39029,#39030,#39031,#39032,#39033,#39034,#39035,
#39036,#39037,#39038,#39039,#39040,#39041,#39042,#39043,#39044,#39045,#39046,
#39047,#39048,#39049,#39050,#39051,#39052,#39053,#39054,#39055,#39056,#39057,
#39058,#39059,#39060,#39061,#39062,#39063,#39064,#39065,#39066,#39067,#39068,
#39069,#39070,#39071,#39072,#39073,#39074,#39075),.UNSPECIFIED.,.F.,.F.)
B_SPLINE_CURVE_WITH_KNOTS((6,1,1,1,1,1,1,1,1,1,1,1,1,1,1,1,1,1,1,1,1,1,
1,1,1,1,1,1,1,1,1,1,1,1,1,1,1,1,1,1,1,1,1,1,1,1,1,1,1,1,1,1,1,1,1,1,1,1,
1,1,1,1,1,1,1,6),(0.,0.0153846153846154,0.0307692307692308,0.0461538461538462,
0.0615384615384615,0.0769230769230769,0.0923076923076923,0.107692307692308,
0.123076923076923,0.138461538461538,0.153846153846154,0.169230769230769,
0.184615384615385,0.2,0.215384615384615,0.230769230769231,0.246153846153846,
0.261538461538462,0.276923076923077,0.292307692307692,0.307692307692308,
0.323076923076923,0.338461538461538,0.353846153846154,0.369230769230769,
0.384615384615385,0.4,0.415384615384615,0.430769230769231,0.446153846153846,
0.461538461538462,0.476923076923077,0.492307692307692,0.507692307692308,
0.523076923076923,0.538461538461538,0.553846153846154,0.569230769230769,
0.584615384615384,0.6,0.615384615384615,0.63076923076923,0.646153846153846,
0.661538461538461,0.676923076923076,0.692307692307692,0.707692307692307,
0.723076923076922,0.738461538461538,0.753846153846153,0.769230769230768,
0.784615384615384,0.799999999999999,0.815384615384614,0.83076923076923,
0.846153846153845,0.86153846153846,0.876923076923076,0.892307692307691,
0.907692307692306,0.923076923076922,0.938461538461537,0.953846153846152,
0.969230769230768,0.984615384615383,0.994228156739699),.UNSPECIFIED.)
CURVE()
GEOMETRIC_REPRESENTATION_ITEM()
RATIONAL_B_SPLINE_CURVE((1.,1.,1.,1.,1.,1.,1.,1.,1.,1.,1.,1.,1.,1.,1.,1.,
1.,1.,1.,1.,1.,1.,1.,1.,1.,1.,1.,1.,1.,1.,1.,1.,1.,1.,1.,1.,1.,1.,1.,1.,
1.,1.,1.,1.,1.,1.,1.,1.,1.,1.,1.,1.,1.,1.,1.,1.,1.,1.,1.,1.,1.,1.,1.,1.,
1.,1.,1.,1.,1.,1.))
REPRESENTATION_ITEM('')
);
#279=(
BOUNDED_CURVE()
B_SPLINE_CURVE(5,(#39079,#39080,#39081,#39082,#39083,#39084,#39085,#39086,
#39087,#39088,#39089,#39090,#39091,#39092,#39093,#39094,#39095,#39096,#39097,
#39098,#39099,#39100,#39101,#39102,#39103,#39104,#39105,#39106,#39107,#39108,
#39109,#39110,#39111,#39112,#39113,#39114,#39115,#39116,#39117,#39118,#39119,
#39120,#39121,#39122,#39123,#39124,#39125,#39126,#39127,#39128,#39129,#39130,
#39131,#39132,#39133,#39134,#39135,#39136,#39137,#39138,#39139,#39140,#39141,
#39142,#39143,#39144,#39145,#39146,#39147,#39148),.UNSPECIFIED.,.F.,.F.)
B_SPLINE_CURVE_WITH_KNOTS((6,1,1,1,1,1,1,1,1,1,1,1,1,1,1,1,1,1,1,1,1,1,
1,1,1,1,1,1,1,1,1,1,1,1,1,1,1,1,1,1,1,1,1,1,1,1,1,1,1,1,1,1,1,1,1,1,1,1,
1,1,1,1,1,1,1,6),(0.00577184337450665,0.0153846153846154,0.0307692307692308,
0.0461538461538462,0.0615384615384615,0.0769230769230769,0.0923076923076923,
0.107692307692308,0.123076923076923,0.138461538461538,0.153846153846154,
0.169230769230769,0.184615384615385,0.2,0.215384615384615,0.230769230769231,
0.246153846153846,0.261538461538462,0.276923076923077,0.292307692307692,
0.307692307692308,0.323076923076923,0.338461538461538,0.353846153846154,
0.369230769230769,0.384615384615385,0.4,0.415384615384615,0.430769230769231,
0.446153846153846,0.461538461538462,0.476923076923077,0.492307692307692,
0.507692307692308,0.523076923076923,0.538461538461538,0.553846153846154,
0.569230769230769,0.584615384615384,0.6,0.615384615384615,0.63076923076923,
0.646153846153846,0.661538461538461,0.676923076923076,0.692307692307692,
0.707692307692307,0.723076923076922,0.738461538461538,0.753846153846153,
0.769230769230768,0.784615384615384,0.799999999999999,0.815384615384614,
0.83076923076923,0.846153846153845,0.86153846153846,0.876923076923076,0.892307692307691,
0.907692307692306,0.923076923076922,0.938461538461537,0.953846153846152,
0.969230769230768,0.984615384615383,1.),.UNSPECIFIED.)
CURVE()
GEOMETRIC_REPRESENTATION_ITEM()
RATIONAL_B_SPLINE_CURVE((1.,1.,1.,1.,1.,1.,1.,1.,1.,1.,1.,1.,1.,1.,1.,1.,
1.,1.,1.,1.,1.,1.,1.,1.,1.,1.,1.,1.,1.,1.,1.,1.,1.,1.,1.,1.,1.,1.,1.,1.,
1.,1.,1.,1.,1.,1.,1.,1.,1.,1.,1.,1.,1.,1.,1.,1.,1.,1.,1.,1.,1.,1.,1.,1.,
1.,1.,1.,1.,1.,1.))
REPRESENTATION_ITEM('')
);
#280=(
BOUNDED_CURVE()
B_SPLINE_CURVE(5,(#39152,#39153,#39154,#39155,#39156,#39157,#39158,#39159,
#39160,#39161,#39162,#39163,#39164,#39165,#39166,#39167,#39168,#39169,#39170,
#39171,#39172,#39173,#39174,#39175,#39176,#39177,#39178,#39179,#39180,#39181,
#39182,#39183,#39184,#39185,#39186,#39187,#39188,#39189,#39190,#39191,#39192,
#39193,#39194,#39195,#39196,#39197,#39198,#39199,#39200,#39201,#39202,#39203,
#39204,#39205,#39206,#39207,#39208,#39209,#39210,#39211,#39212,#39213,#39214,
#39215,#39216,#39217,#39218,#39219,#39220,#39221),.UNSPECIFIED.,.F.,.F.)
B_SPLINE_CURVE_WITH_KNOTS((6,1,1,1,1,1,1,1,1,1,1,1,1,1,1,1,1,1,1,1,1,1,
1,1,1,1,1,1,1,1,1,1,1,1,1,1,1,1,1,1,1,1,1,1,1,1,1,1,1,1,1,1,1,1,1,1,1,1,
1,1,1,1,1,1,1,6),(0.,0.0153846153846154,0.0307692307692308,0.0461538461538462,
0.0615384615384615,0.0769230769230769,0.0923076923076923,0.107692307692308,
0.123076923076923,0.138461538461538,0.153846153846154,0.169230769230769,
0.184615384615385,0.2,0.215384615384615,0.230769230769231,0.246153846153846,
0.261538461538462,0.276923076923077,0.292307692307692,0.307692307692308,
0.323076923076923,0.338461538461538,0.353846153846154,0.369230769230769,
0.384615384615385,0.4,0.415384615384615,0.430769230769231,0.446153846153846,
0.461538461538462,0.476923076923077,0.492307692307692,0.507692307692308,
0.523076923076923,0.538461538461538,0.553846153846154,0.569230769230769,
0.584615384615384,0.6,0.615384615384615,0.63076923076923,0.646153846153846,
0.661538461538461,0.676923076923076,0.692307692307692,0.707692307692307,
0.723076923076922,0.738461538461538,0.753846153846153,0.769230769230768,
0.784615384615384,0.799999999999999,0.815384615384614,0.83076923076923,
0.846153846153845,0.86153846153846,0.876923076923076,0.892307692307691,
0.907692307692306,0.923076923076922,0.938461538461537,0.953846153846152,
0.969230769230768,0.984615384615383,0.994228156739691),.UNSPECIFIED.)
CURVE()
GEOMETRIC_REPRESENTATION_ITEM()
RATIONAL_B_SPLINE_CURVE((1.,1.,1.,1.,1.,1.,1.,1.,1.,1.,1.,1.,1.,1.,1.,1.,
1.,1.,1.,1.,1.,1.,1.,1.,1.,1.,1.,1.,1.,1.,1.,1.,1.,1.,1.,1.,1.,1.,1.,1.,
1.,1.,1.,1.,1.,1.,1.,1.,1.,1.,1.,1.,1.,1.,1.,1.,1.,1.,1.,1.,1.,1.,1.,1.,
1.,1.,1.,1.,1.,1.))
REPRESENTATION_ITEM('')
);
#281=(
BOUNDED_CURVE()
B_SPLINE_CURVE(5,(#39225,#39226,#39227,#39228,#39229,#39230,#39231,#39232,
#39233,#39234,#39235,#39236,#39237,#39238,#39239,#39240,#39241,#39242,#39243,
#39244,#39245,#39246,#39247,#39248,#39249,#39250,#39251,#39252,#39253,#39254,
#39255,#39256,#39257,#39258,#39259,#39260,#39261,#39262,#39263,#39264,#39265,
#39266,#39267,#39268,#39269,#39270,#39271,#39272,#39273,#39274,#39275,#39276,
#39277,#39278,#39279,#39280,#39281,#39282,#39283,#39284,#39285,#39286,#39287,
#39288,#39289,#39290,#39291,#39292,#39293,#39294),.UNSPECIFIED.,.F.,.F.)
B_SPLINE_CURVE_WITH_KNOTS((6,1,1,1,1,1,1,1,1,1,1,1,1,1,1,1,1,1,1,1,1,1,
1,1,1,1,1,1,1,1,1,1,1,1,1,1,1,1,1,1,1,1,1,1,1,1,1,1,1,1,1,1,1,1,1,1,1,1,
1,1,1,1,1,1,1,6),(0.00577184337450785,0.0153846153846154,0.0307692307692308,
0.0461538461538462,0.0615384615384615,0.0769230769230769,0.0923076923076923,
0.107692307692308,0.123076923076923,0.138461538461538,0.153846153846154,
0.169230769230769,0.184615384615385,0.2,0.215384615384615,0.230769230769231,
0.246153846153846,0.261538461538462,0.276923076923077,0.292307692307692,
0.307692307692308,0.323076923076923,0.338461538461538,0.353846153846154,
0.369230769230769,0.384615384615385,0.4,0.415384615384615,0.430769230769231,
0.446153846153846,0.461538461538462,0.476923076923077,0.492307692307692,
0.507692307692308,0.523076923076923,0.538461538461538,0.553846153846154,
0.569230769230769,0.584615384615384,0.6,0.615384615384615,0.63076923076923,
0.646153846153846,0.661538461538461,0.676923076923076,0.692307692307692,
0.707692307692307,0.723076923076922,0.738461538461538,0.753846153846153,
0.769230769230768,0.784615384615384,0.799999999999999,0.815384615384614,
0.83076923076923,0.846153846153845,0.86153846153846,0.876923076923076,0.892307692307691,
0.907692307692306,0.923076923076922,0.938461538461537,0.953846153846152,
0.969230769230768,0.984615384615383,1.),.UNSPECIFIED.)
CURVE()
GEOMETRIC_REPRESENTATION_ITEM()
RATIONAL_B_SPLINE_CURVE((1.,1.,1.,1.,1.,1.,1.,1.,1.,1.,1.,1.,1.,1.,1.,1.,
1.,1.,1.,1.,1.,1.,1.,1.,1.,1.,1.,1.,1.,1.,1.,1.,1.,1.,1.,1.,1.,1.,1.,1.,
1.,1.,1.,1.,1.,1.,1.,1.,1.,1.,1.,1.,1.,1.,1.,1.,1.,1.,1.,1.,1.,1.,1.,1.,
1.,1.,1.,1.,1.,1.))
REPRESENTATION_ITEM('')
);
#282=(
BOUNDED_CURVE()
B_SPLINE_CURVE(5,(#39298,#39299,#39300,#39301,#39302,#39303,#39304,#39305,
#39306,#39307,#39308,#39309,#39310,#39311,#39312,#39313,#39314,#39315,#39316,
#39317,#39318,#39319,#39320,#39321,#39322,#39323,#39324,#39325,#39326,#39327,
#39328,#39329,#39330,#39331,#39332,#39333,#39334,#39335,#39336,#39337,#39338,
#39339,#39340,#39341,#39342,#39343,#39344,#39345,#39346,#39347,#39348,#39349,
#39350,#39351,#39352,#39353,#39354,#39355,#39356,#39357,#39358,#39359,#39360,
#39361,#39362,#39363,#39364,#39365,#39366,#39367),.UNSPECIFIED.,.F.,.F.)
B_SPLINE_CURVE_WITH_KNOTS((6,1,1,1,1,1,1,1,1,1,1,1,1,1,1,1,1,1,1,1,1,1,
1,1,1,1,1,1,1,1,1,1,1,1,1,1,1,1,1,1,1,1,1,1,1,1,1,1,1,1,1,1,1,1,1,1,1,1,
1,1,1,1,1,1,1,6),(0.,0.0153846153846154,0.0307692307692308,0.0461538461538462,
0.0615384615384615,0.0769230769230769,0.0923076923076923,0.107692307692308,
0.123076923076923,0.138461538461538,0.153846153846154,0.169230769230769,
0.184615384615385,0.2,0.215384615384615,0.230769230769231,0.246153846153846,
0.261538461538462,0.276923076923077,0.292307692307692,0.307692307692308,
0.323076923076923,0.338461538461538,0.353846153846154,0.369230769230769,
0.384615384615385,0.4,0.415384615384615,0.430769230769231,0.446153846153846,
0.461538461538462,0.476923076923077,0.492307692307692,0.507692307692308,
0.523076923076923,0.538461538461538,0.553846153846154,0.569230769230769,
0.584615384615384,0.6,0.615384615384615,0.63076923076923,0.646153846153846,
0.661538461538461,0.676923076923076,0.692307692307692,0.707692307692307,
0.723076923076922,0.738461538461538,0.753846153846153,0.769230769230768,
0.784615384615384,0.799999999999999,0.815384615384614,0.83076923076923,
0.846153846153845,0.86153846153846,0.876923076923076,0.892307692307691,
0.907692307692306,0.923076923076922,0.938461538461537,0.953846153846152,
0.969230769230768,0.984615384615383,0.994228156739708),.UNSPECIFIED.)
CURVE()
GEOMETRIC_REPRESENTATION_ITEM()
RATIONAL_B_SPLINE_CURVE((1.,1.,1.,1.,1.,1.,1.,1.,1.,1.,1.,1.,1.,1.,1.,1.,
1.,1.,1.,1.,1.,1.,1.,1.,1.,1.,1.,1.,1.,1.,1.,1.,1.,1.,1.,1.,1.,1.,1.,1.,
1.,1.,1.,1.,1.,1.,1.,1.,1.,1.,1.,1.,1.,1.,1.,1.,1.,1.,1.,1.,1.,1.,1.,1.,
1.,1.,1.,1.,1.,1.))
REPRESENTATION_ITEM('')
);
#283=(
BOUNDED_CURVE()
B_SPLINE_CURVE(5,(#39371,#39372,#39373,#39374,#39375,#39376,#39377,#39378,
#39379,#39380,#39381,#39382,#39383,#39384,#39385,#39386,#39387,#39388,#39389,
#39390,#39391,#39392,#39393,#39394,#39395,#39396,#39397,#39398,#39399,#39400,
#39401,#39402,#39403,#39404,#39405,#39406,#39407,#39408,#39409,#39410,#39411,
#39412,#39413,#39414,#39415,#39416,#39417,#39418,#39419,#39420,#39421,#39422,
#39423,#39424,#39425,#39426,#39427,#39428,#39429,#39430,#39431,#39432,#39433,
#39434,#39435,#39436,#39437,#39438,#39439,#39440),.UNSPECIFIED.,.F.,.F.)
B_SPLINE_CURVE_WITH_KNOTS((6,1,1,1,1,1,1,1,1,1,1,1,1,1,1,1,1,1,1,1,1,1,
1,1,1,1,1,1,1,1,1,1,1,1,1,1,1,1,1,1,1,1,1,1,1,1,1,1,1,1,1,1,1,1,1,1,1,1,
1,1,1,1,1,1,1,6),(0.00577184337450072,0.0153846153846154,0.0307692307692308,
0.0461538461538462,0.0615384615384615,0.0769230769230769,0.0923076923076923,
0.107692307692308,0.123076923076923,0.138461538461538,0.153846153846154,
0.169230769230769,0.184615384615385,0.2,0.215384615384615,0.230769230769231,
0.246153846153846,0.261538461538462,0.276923076923077,0.292307692307692,
0.307692307692308,0.323076923076923,0.338461538461538,0.353846153846154,
0.369230769230769,0.384615384615385,0.4,0.415384615384615,0.430769230769231,
0.446153846153846,0.461538461538462,0.476923076923077,0.492307692307692,
0.507692307692308,0.523076923076923,0.538461538461538,0.553846153846154,
0.569230769230769,0.584615384615384,0.6,0.615384615384615,0.63076923076923,
0.646153846153846,0.661538461538461,0.676923076923076,0.692307692307692,
0.707692307692307,0.723076923076922,0.738461538461538,0.753846153846153,
0.769230769230768,0.784615384615384,0.799999999999999,0.815384615384614,
0.83076923076923,0.846153846153845,0.86153846153846,0.876923076923076,0.892307692307691,
0.907692307692306,0.923076923076922,0.938461538461537,0.953846153846152,
0.969230769230768,0.984615384615383,1.),.UNSPECIFIED.)
CURVE()
GEOMETRIC_REPRESENTATION_ITEM()
RATIONAL_B_SPLINE_CURVE((1.,1.,1.,1.,1.,1.,1.,1.,1.,1.,1.,1.,1.,1.,1.,1.,
1.,1.,1.,1.,1.,1.,1.,1.,1.,1.,1.,1.,1.,1.,1.,1.,1.,1.,1.,1.,1.,1.,1.,1.,
1.,1.,1.,1.,1.,1.,1.,1.,1.,1.,1.,1.,1.,1.,1.,1.,1.,1.,1.,1.,1.,1.,1.,1.,
1.,1.,1.,1.,1.,1.))
REPRESENTATION_ITEM('')
);
#284=(
BOUNDED_CURVE()
B_SPLINE_CURVE(5,(#39444,#39445,#39446,#39447,#39448,#39449,#39450,#39451,
#39452,#39453,#39454,#39455,#39456,#39457,#39458,#39459,#39460,#39461,#39462,
#39463,#39464,#39465,#39466,#39467,#39468,#39469,#39470,#39471,#39472,#39473,
#39474,#39475,#39476,#39477,#39478,#39479,#39480,#39481,#39482,#39483,#39484,
#39485,#39486,#39487,#39488,#39489,#39490,#39491,#39492,#39493,#39494,#39495,
#39496,#39497,#39498,#39499,#39500,#39501,#39502,#39503,#39504,#39505,#39506,
#39507,#39508,#39509,#39510,#39511,#39512,#39513),.UNSPECIFIED.,.F.,.F.)
B_SPLINE_CURVE_WITH_KNOTS((6,1,1,1,1,1,1,1,1,1,1,1,1,1,1,1,1,1,1,1,1,1,
1,1,1,1,1,1,1,1,1,1,1,1,1,1,1,1,1,1,1,1,1,1,1,1,1,1,1,1,1,1,1,1,1,1,1,1,
1,1,1,1,1,1,1,6),(0.,0.0153846153846154,0.0307692307692308,0.0461538461538462,
0.0615384615384615,0.0769230769230769,0.0923076923076923,0.107692307692308,
0.123076923076923,0.138461538461538,0.153846153846154,0.169230769230769,
0.184615384615385,0.2,0.215384615384615,0.230769230769231,0.246153846153846,
0.261538461538462,0.276923076923077,0.292307692307692,0.307692307692308,
0.323076923076923,0.338461538461538,0.353846153846154,0.369230769230769,
0.384615384615385,0.4,0.415384615384615,0.430769230769231,0.446153846153846,
0.461538461538462,0.476923076923077,0.492307692307692,0.507692307692308,
0.523076923076923,0.538461538461538,0.553846153846154,0.569230769230769,
0.584615384615384,0.6,0.615384615384615,0.63076923076923,0.646153846153846,
0.661538461538461,0.676923076923076,0.692307692307692,0.707692307692307,
0.723076923076922,0.738461538461538,0.753846153846153,0.769230769230768,
0.784615384615384,0.799999999999999,0.815384615384614,0.83076923076923,
0.846153846153845,0.86153846153846,0.876923076923076,0.892307692307691,
0.907692307692306,0.923076923076922,0.938461538461537,0.953846153846152,
0.969230769230768,0.984615384615383,0.994228156739706),.UNSPECIFIED.)
CURVE()
GEOMETRIC_REPRESENTATION_ITEM()
RATIONAL_B_SPLINE_CURVE((1.,1.,1.,1.,1.,1.,1.,1.,1.,1.,1.,1.,1.,1.,1.,1.,
1.,1.,1.,1.,1.,1.,1.,1.,1.,1.,1.,1.,1.,1.,1.,1.,1.,1.,1.,1.,1.,1.,1.,1.,
1.,1.,1.,1.,1.,1.,1.,1.,1.,1.,1.,1.,1.,1.,1.,1.,1.,1.,1.,1.,1.,1.,1.,1.,
1.,1.,1.,1.,1.,1.))
REPRESENTATION_ITEM('')
);
#285=(
BOUNDED_CURVE()
B_SPLINE_CURVE(5,(#39517,#39518,#39519,#39520,#39521,#39522,#39523,#39524,
#39525,#39526,#39527,#39528,#39529,#39530,#39531,#39532,#39533,#39534,#39535,
#39536,#39537,#39538,#39539,#39540,#39541,#39542,#39543,#39544,#39545,#39546,
#39547,#39548,#39549,#39550,#39551,#39552,#39553,#39554,#39555,#39556,#39557,
#39558,#39559,#39560,#39561,#39562,#39563,#39564,#39565,#39566,#39567,#39568,
#39569,#39570,#39571,#39572,#39573,#39574,#39575,#39576,#39577,#39578,#39579,
#39580,#39581,#39582,#39583,#39584,#39585,#39586),.UNSPECIFIED.,.F.,.F.)
B_SPLINE_CURVE_WITH_KNOTS((6,1,1,1,1,1,1,1,1,1,1,1,1,1,1,1,1,1,1,1,1,1,
1,1,1,1,1,1,1,1,1,1,1,1,1,1,1,1,1,1,1,1,1,1,1,1,1,1,1,1,1,1,1,1,1,1,1,1,
1,1,1,1,1,1,1,6),(0.00577184337450902,0.0153846153846154,0.0307692307692308,
0.0461538461538462,0.0615384615384615,0.0769230769230769,0.0923076923076923,
0.107692307692308,0.123076923076923,0.138461538461538,0.153846153846154,
0.169230769230769,0.184615384615385,0.2,0.215384615384615,0.230769230769231,
0.246153846153846,0.261538461538462,0.276923076923077,0.292307692307692,
0.307692307692308,0.323076923076923,0.338461538461538,0.353846153846154,
0.369230769230769,0.384615384615385,0.4,0.415384615384615,0.430769230769231,
0.446153846153846,0.461538461538462,0.476923076923077,0.492307692307692,
0.507692307692308,0.523076923076923,0.538461538461538,0.553846153846154,
0.569230769230769,0.584615384615384,0.6,0.615384615384615,0.63076923076923,
0.646153846153846,0.661538461538461,0.676923076923076,0.692307692307692,
0.707692307692307,0.723076923076922,0.738461538461538,0.753846153846153,
0.769230769230768,0.784615384615384,0.799999999999999,0.815384615384614,
0.83076923076923,0.846153846153845,0.86153846153846,0.876923076923076,0.892307692307691,
0.907692307692306,0.923076923076922,0.938461538461537,0.953846153846152,
0.969230769230768,0.984615384615383,1.),.UNSPECIFIED.)
CURVE()
GEOMETRIC_REPRESENTATION_ITEM()
RATIONAL_B_SPLINE_CURVE((1.,1.,1.,1.,1.,1.,1.,1.,1.,1.,1.,1.,1.,1.,1.,1.,
1.,1.,1.,1.,1.,1.,1.,1.,1.,1.,1.,1.,1.,1.,1.,1.,1.,1.,1.,1.,1.,1.,1.,1.,
1.,1.,1.,1.,1.,1.,1.,1.,1.,1.,1.,1.,1.,1.,1.,1.,1.,1.,1.,1.,1.,1.,1.,1.,
1.,1.,1.,1.,1.,1.))
REPRESENTATION_ITEM('')
);
#286=(
BOUNDED_CURVE()
B_SPLINE_CURVE(5,(#39590,#39591,#39592,#39593,#39594,#39595,#39596,#39597,
#39598,#39599,#39600,#39601,#39602,#39603,#39604,#39605,#39606,#39607,#39608,
#39609,#39610,#39611,#39612,#39613,#39614,#39615,#39616,#39617,#39618,#39619,
#39620,#39621,#39622,#39623,#39624,#39625,#39626,#39627,#39628,#39629,#39630,
#39631,#39632,#39633,#39634,#39635,#39636,#39637,#39638,#39639,#39640,#39641,
#39642,#39643,#39644,#39645,#39646,#39647,#39648,#39649,#39650,#39651,#39652,
#39653,#39654,#39655,#39656,#39657,#39658,#39659),.UNSPECIFIED.,.F.,.F.)
B_SPLINE_CURVE_WITH_KNOTS((6,1,1,1,1,1,1,1,1,1,1,1,1,1,1,1,1,1,1,1,1,1,
1,1,1,1,1,1,1,1,1,1,1,1,1,1,1,1,1,1,1,1,1,1,1,1,1,1,1,1,1,1,1,1,1,1,1,1,
1,1,1,1,1,1,1,6),(0.,0.0153846153846154,0.0307692307692308,0.0461538461538462,
0.0615384615384615,0.0769230769230769,0.0923076923076923,0.107692307692308,
0.123076923076923,0.138461538461538,0.153846153846154,0.169230769230769,
0.184615384615385,0.2,0.215384615384615,0.230769230769231,0.246153846153846,
0.261538461538462,0.276923076923077,0.292307692307692,0.307692307692308,
0.323076923076923,0.338461538461538,0.353846153846154,0.369230769230769,
0.384615384615385,0.4,0.415384615384615,0.430769230769231,0.446153846153846,
0.461538461538462,0.476923076923077,0.492307692307692,0.507692307692308,
0.523076923076923,0.538461538461538,0.553846153846154,0.569230769230769,
0.584615384615384,0.6,0.615384615384615,0.63076923076923,0.646153846153846,
0.661538461538461,0.676923076923076,0.692307692307692,0.707692307692307,
0.723076923076922,0.738461538461538,0.753846153846153,0.769230769230768,
0.784615384615384,0.799999999999999,0.815384615384614,0.83076923076923,
0.846153846153845,0.86153846153846,0.876923076923076,0.892307692307691,
0.907692307692306,0.923076923076922,0.938461538461537,0.953846153846152,
0.969230769230768,0.984615384615383,0.994228156739698),.UNSPECIFIED.)
CURVE()
GEOMETRIC_REPRESENTATION_ITEM()
RATIONAL_B_SPLINE_CURVE((1.,1.,1.,1.,1.,1.,1.,1.,1.,1.,1.,1.,1.,1.,1.,1.,
1.,1.,1.,1.,1.,1.,1.,1.,1.,1.,1.,1.,1.,1.,1.,1.,1.,1.,1.,1.,1.,1.,1.,1.,
1.,1.,1.,1.,1.,1.,1.,1.,1.,1.,1.,1.,1.,1.,1.,1.,1.,1.,1.,1.,1.,1.,1.,1.,
1.,1.,1.,1.,1.,1.))
REPRESENTATION_ITEM('')
);
#287=(
BOUNDED_CURVE()
B_SPLINE_CURVE(5,(#39663,#39664,#39665,#39666,#39667,#39668,#39669,#39670,
#39671,#39672,#39673,#39674,#39675,#39676,#39677,#39678,#39679,#39680,#39681,
#39682,#39683,#39684,#39685,#39686,#39687,#39688,#39689,#39690,#39691,#39692,
#39693,#39694,#39695,#39696,#39697,#39698,#39699,#39700,#39701,#39702,#39703,
#39704,#39705,#39706,#39707,#39708,#39709,#39710,#39711,#39712,#39713,#39714,
#39715,#39716,#39717,#39718,#39719,#39720,#39721,#39722,#39723,#39724,#39725,
#39726,#39727,#39728,#39729,#39730,#39731,#39732),.UNSPECIFIED.,.F.,.F.)
B_SPLINE_CURVE_WITH_KNOTS((6,1,1,1,1,1,1,1,1,1,1,1,1,1,1,1,1,1,1,1,1,1,
1,1,1,1,1,1,1,1,1,1,1,1,1,1,1,1,1,1,1,1,1,1,1,1,1,1,1,1,1,1,1,1,1,1,1,1,
1,1,1,1,1,1,1,6),(0.00577184337451611,0.0153846153846154,0.0307692307692308,
0.0461538461538462,0.0615384615384615,0.0769230769230769,0.0923076923076923,
0.107692307692308,0.123076923076923,0.138461538461538,0.153846153846154,
0.169230769230769,0.184615384615385,0.2,0.215384615384615,0.230769230769231,
0.246153846153846,0.261538461538462,0.276923076923077,0.292307692307692,
0.307692307692308,0.323076923076923,0.338461538461538,0.353846153846154,
0.369230769230769,0.384615384615385,0.4,0.415384615384615,0.430769230769231,
0.446153846153846,0.461538461538462,0.476923076923077,0.492307692307692,
0.507692307692308,0.523076923076923,0.538461538461538,0.553846153846154,
0.569230769230769,0.584615384615384,0.6,0.615384615384615,0.63076923076923,
0.646153846153846,0.661538461538461,0.676923076923076,0.692307692307692,
0.707692307692307,0.723076923076922,0.738461538461538,0.753846153846153,
0.769230769230768,0.784615384615384,0.799999999999999,0.815384615384614,
0.83076923076923,0.846153846153845,0.86153846153846,0.876923076923076,0.892307692307691,
0.907692307692306,0.923076923076922,0.938461538461537,0.953846153846152,
0.969230769230768,0.984615384615383,1.),.UNSPECIFIED.)
CURVE()
GEOMETRIC_REPRESENTATION_ITEM()
RATIONAL_B_SPLINE_CURVE((1.,1.,1.,1.,1.,1.,1.,1.,1.,1.,1.,1.,1.,1.,1.,1.,
1.,1.,1.,1.,1.,1.,1.,1.,1.,1.,1.,1.,1.,1.,1.,1.,1.,1.,1.,1.,1.,1.,1.,1.,
1.,1.,1.,1.,1.,1.,1.,1.,1.,1.,1.,1.,1.,1.,1.,1.,1.,1.,1.,1.,1.,1.,1.,1.,
1.,1.,1.,1.,1.,1.))
REPRESENTATION_ITEM('')
);
#288=(
BOUNDED_CURVE()
B_SPLINE_CURVE(5,(#39736,#39737,#39738,#39739,#39740,#39741,#39742,#39743,
#39744,#39745,#39746,#39747,#39748,#39749,#39750,#39751,#39752,#39753,#39754,
#39755,#39756,#39757,#39758,#39759,#39760,#39761,#39762,#39763,#39764,#39765,
#39766,#39767,#39768,#39769,#39770,#39771,#39772,#39773,#39774,#39775,#39776,
#39777,#39778,#39779,#39780,#39781,#39782,#39783,#39784,#39785,#39786,#39787,
#39788,#39789,#39790,#39791,#39792,#39793,#39794,#39795,#39796,#39797,#39798,
#39799,#39800,#39801,#39802,#39803,#39804,#39805),.UNSPECIFIED.,.F.,.F.)
B_SPLINE_CURVE_WITH_KNOTS((6,1,1,1,1,1,1,1,1,1,1,1,1,1,1,1,1,1,1,1,1,1,
1,1,1,1,1,1,1,1,1,1,1,1,1,1,1,1,1,1,1,1,1,1,1,1,1,1,1,1,1,1,1,1,1,1,1,1,
1,1,1,1,1,1,1,6),(0.,0.0153846153846154,0.0307692307692308,0.0461538461538462,
0.0615384615384615,0.0769230769230769,0.0923076923076923,0.107692307692308,
0.123076923076923,0.138461538461538,0.153846153846154,0.169230769230769,
0.184615384615385,0.2,0.215384615384615,0.230769230769231,0.246153846153846,
0.261538461538462,0.276923076923077,0.292307692307692,0.307692307692308,
0.323076923076923,0.338461538461538,0.353846153846154,0.369230769230769,
0.384615384615385,0.4,0.415384615384615,0.430769230769231,0.446153846153846,
0.461538461538462,0.476923076923077,0.492307692307692,0.507692307692308,
0.523076923076923,0.538461538461538,0.553846153846154,0.569230769230769,
0.584615384615384,0.6,0.615384615384615,0.63076923076923,0.646153846153846,
0.661538461538461,0.676923076923076,0.692307692307692,0.707692307692307,
0.723076923076922,0.738461538461538,0.753846153846153,0.769230769230768,
0.784615384615384,0.799999999999999,0.815384615384614,0.83076923076923,
0.846153846153845,0.86153846153846,0.876923076923076,0.892307692307691,
0.907692307692306,0.923076923076922,0.938461538461537,0.953846153846152,
0.969230769230768,0.984615384615383,0.994228156739704),.UNSPECIFIED.)
CURVE()
GEOMETRIC_REPRESENTATION_ITEM()
RATIONAL_B_SPLINE_CURVE((1.,1.,1.,1.,1.,1.,1.,1.,1.,1.,1.,1.,1.,1.,1.,1.,
1.,1.,1.,1.,1.,1.,1.,1.,1.,1.,1.,1.,1.,1.,1.,1.,1.,1.,1.,1.,1.,1.,1.,1.,
1.,1.,1.,1.,1.,1.,1.,1.,1.,1.,1.,1.,1.,1.,1.,1.,1.,1.,1.,1.,1.,1.,1.,1.,
1.,1.,1.,1.,1.,1.))
REPRESENTATION_ITEM('')
);
#289=(
BOUNDED_CURVE()
B_SPLINE_CURVE(5,(#39809,#39810,#39811,#39812,#39813,#39814,#39815,#39816,
#39817,#39818,#39819,#39820,#39821,#39822,#39823,#39824,#39825,#39826,#39827,
#39828,#39829,#39830,#39831,#39832,#39833,#39834,#39835,#39836,#39837,#39838,
#39839,#39840,#39841,#39842,#39843,#39844,#39845,#39846,#39847,#39848,#39849,
#39850,#39851,#39852,#39853,#39854,#39855,#39856,#39857,#39858,#39859,#39860,
#39861,#39862,#39863,#39864,#39865,#39866,#39867,#39868,#39869,#39870,#39871,
#39872,#39873,#39874,#39875,#39876,#39877,#39878),.UNSPECIFIED.,.F.,.F.)
B_SPLINE_CURVE_WITH_KNOTS((6,1,1,1,1,1,1,1,1,1,1,1,1,1,1,1,1,1,1,1,1,1,
1,1,1,1,1,1,1,1,1,1,1,1,1,1,1,1,1,1,1,1,1,1,1,1,1,1,1,1,1,1,1,1,1,1,1,1,
1,1,1,1,1,1,1,6),(0.00577184337449692,0.0153846153846154,0.0307692307692308,
0.0461538461538462,0.0615384615384615,0.0769230769230769,0.0923076923076923,
0.107692307692308,0.123076923076923,0.138461538461538,0.153846153846154,
0.169230769230769,0.184615384615385,0.2,0.215384615384615,0.230769230769231,
0.246153846153846,0.261538461538462,0.276923076923077,0.292307692307692,
0.307692307692308,0.323076923076923,0.338461538461538,0.353846153846154,
0.369230769230769,0.384615384615385,0.4,0.415384615384615,0.430769230769231,
0.446153846153846,0.461538461538462,0.476923076923077,0.492307692307692,
0.507692307692308,0.523076923076923,0.538461538461538,0.553846153846154,
0.569230769230769,0.584615384615384,0.6,0.615384615384615,0.63076923076923,
0.646153846153846,0.661538461538461,0.676923076923076,0.692307692307692,
0.707692307692307,0.723076923076922,0.738461538461538,0.753846153846153,
0.769230769230768,0.784615384615384,0.799999999999999,0.815384615384614,
0.83076923076923,0.846153846153845,0.86153846153846,0.876923076923076,0.892307692307691,
0.907692307692306,0.923076923076922,0.938461538461537,0.953846153846152,
0.969230769230768,0.984615384615383,1.),.UNSPECIFIED.)
CURVE()
GEOMETRIC_REPRESENTATION_ITEM()
RATIONAL_B_SPLINE_CURVE((1.,1.,1.,1.,1.,1.,1.,1.,1.,1.,1.,1.,1.,1.,1.,1.,
1.,1.,1.,1.,1.,1.,1.,1.,1.,1.,1.,1.,1.,1.,1.,1.,1.,1.,1.,1.,1.,1.,1.,1.,
1.,1.,1.,1.,1.,1.,1.,1.,1.,1.,1.,1.,1.,1.,1.,1.,1.,1.,1.,1.,1.,1.,1.,1.,
1.,1.,1.,1.,1.,1.))
REPRESENTATION_ITEM('')
);
#290=(
BOUNDED_CURVE()
B_SPLINE_CURVE(5,(#39881,#39882,#39883,#39884,#39885,#39886,#39887,#39888,
#39889,#39890,#39891,#39892,#39893,#39894,#39895,#39896,#39897,#39898,#39899,
#39900,#39901,#39902,#39903,#39904,#39905,#39906,#39907,#39908,#39909,#39910,
#39911,#39912,#39913,#39914,#39915,#39916,#39917,#39918,#39919,#39920,#39921,
#39922,#39923,#39924,#39925,#39926,#39927,#39928,#39929,#39930,#39931,#39932,
#39933,#39934,#39935,#39936,#39937,#39938,#39939,#39940,#39941,#39942,#39943,
#39944,#39945,#39946,#39947,#39948,#39949,#39950),.UNSPECIFIED.,.F.,.F.)
B_SPLINE_CURVE_WITH_KNOTS((6,1,1,1,1,1,1,1,1,1,1,1,1,1,1,1,1,1,1,1,1,1,
1,1,1,1,1,1,1,1,1,1,1,1,1,1,1,1,1,1,1,1,1,1,1,1,1,1,1,1,1,1,1,1,1,1,1,1,
1,1,1,1,1,1,1,6),(0.,0.0153846153846154,0.0307692307692308,0.0461538461538462,
0.0615384615384615,0.0769230769230769,0.0923076923076923,0.107692307692308,
0.123076923076923,0.138461538461538,0.153846153846154,0.169230769230769,
0.184615384615385,0.2,0.215384615384615,0.230769230769231,0.246153846153846,
0.261538461538462,0.276923076923077,0.292307692307692,0.307692307692308,
0.323076923076923,0.338461538461538,0.353846153846154,0.369230769230769,
0.384615384615385,0.4,0.415384615384615,0.430769230769231,0.446153846153846,
0.461538461538462,0.476923076923077,0.492307692307692,0.507692307692308,
0.523076923076923,0.538461538461538,0.553846153846154,0.569230769230769,
0.584615384615384,0.6,0.615384615384615,0.63076923076923,0.646153846153846,
0.661538461538461,0.676923076923076,0.692307692307692,0.707692307692307,
0.723076923076922,0.738461538461538,0.753846153846153,0.769230769230768,
0.784615384615384,0.799999999999999,0.815384615384614,0.83076923076923,
0.846153846153845,0.86153846153846,0.876923076923076,0.892307692307691,
0.907692307692306,0.923076923076922,0.938461538461537,0.953846153846152,
0.969230769230768,0.984615384615383,0.994228156739723),.UNSPECIFIED.)
CURVE()
GEOMETRIC_REPRESENTATION_ITEM()
RATIONAL_B_SPLINE_CURVE((1.,1.,1.,1.,1.,1.,1.,1.,1.,1.,1.,1.,1.,1.,1.,1.,
1.,1.,1.,1.,1.,1.,1.,1.,1.,1.,1.,1.,1.,1.,1.,1.,1.,1.,1.,1.,1.,1.,1.,1.,
1.,1.,1.,1.,1.,1.,1.,1.,1.,1.,1.,1.,1.,1.,1.,1.,1.,1.,1.,1.,1.,1.,1.,1.,
1.,1.,1.,1.,1.,1.))
REPRESENTATION_ITEM('')
);
#291=(
BOUNDED_CURVE()
B_SPLINE_CURVE(5,(#40109,#40110,#40111,#40112,#40113,#40114,#40115,#40116,
#40117,#40118,#40119,#40120,#40121,#40122,#40123,#40124,#40125,#40126,#40127,
#40128,#40129,#40130,#40131,#40132,#40133,#40134,#40135,#40136,#40137,#40138,
#40139,#40140,#40141,#40142,#40143,#40144,#40145,#40146,#40147,#40148,#40149,
#40150,#40151,#40152,#40153,#40154,#40155,#40156,#40157,#40158,#40159,#40160,
#40161,#40162,#40163,#40164,#40165,#40166,#40167,#40168,#40169,#40170,#40171,
#40172,#40173,#40174,#40175,#40176,#40177,#40178),.UNSPECIFIED.,.F.,.F.)
B_SPLINE_CURVE_WITH_KNOTS((6,1,1,1,1,1,1,1,1,1,1,1,1,1,1,1,1,1,1,1,1,1,
1,1,1,1,1,1,1,1,1,1,1,1,1,1,1,1,1,1,1,1,1,1,1,1,1,1,1,1,1,1,1,1,1,1,1,1,
1,1,1,1,1,1,1,6),(-1.,-0.984615384615383,-0.969230769230768,-0.953846153846152,
-0.938461538461537,-0.923076923076922,-0.907692307692306,-0.892307692307691,
-0.876923076923076,-0.86153846153846,-0.846153846153845,-0.83076923076923,
-0.815384615384614,-0.799999999999999,-0.784615384615384,-0.769230769230768,
-0.753846153846153,-0.738461538461538,-0.723076923076922,-0.707692307692307,
-0.692307692307692,-0.676923076923076,-0.661538461538461,-0.646153846153846,
-0.63076923076923,-0.615384615384615,-0.6,-0.584615384615384,-0.569230769230769,
-0.553846153846154,-0.538461538461538,-0.523076923076923,-0.507692307692308,
-0.492307692307692,-0.476923076923077,-0.461538461538462,-0.446153846153846,
-0.430769230769231,-0.415384615384615,-0.4,-0.384615384615385,-0.369230769230769,
-0.353846153846154,-0.338461538461538,-0.323076923076923,-0.307692307692308,
-0.292307692307692,-0.276923076923077,-0.261538461538462,-0.246153846153846,
-0.230769230769231,-0.215384615384615,-0.2,-0.184615384615385,-0.169230769230769,
-0.153846153846154,-0.138461538461538,-0.123076923076923,-0.107692307692308,
-0.0923076923076923,-0.0769230769230769,-0.0615384615384615,-0.0461538461538462,
-0.0307692307692308,-0.0153846153846154,-0.00577184337448906),
 .UNSPECIFIED.)
CURVE()
GEOMETRIC_REPRESENTATION_ITEM()
RATIONAL_B_SPLINE_CURVE((1.,1.,1.,1.,1.,1.,1.,1.,1.,1.,1.,1.,1.,1.,1.,1.,
1.,1.,1.,1.,1.,1.,1.,1.,1.,1.,1.,1.,1.,1.,1.,1.,1.,1.,1.,1.,1.,1.,1.,1.,
1.,1.,1.,1.,1.,1.,1.,1.,1.,1.,1.,1.,1.,1.,1.,1.,1.,1.,1.,1.,1.,1.,1.,1.,
1.,1.,1.,1.,1.,1.))
REPRESENTATION_ITEM('')
);
#292=(
BOUNDED_CURVE()
B_SPLINE_CURVE(5,(#40329,#40330,#40331,#40332,#40333,#40334,#40335,#40336,
#40337,#40338,#40339,#40340,#40341,#40342,#40343,#40344,#40345,#40346,#40347,
#40348,#40349,#40350,#40351,#40352,#40353,#40354,#40355,#40356,#40357,#40358,
#40359,#40360,#40361,#40362,#40363,#40364,#40365,#40366,#40367,#40368,#40369,
#40370,#40371,#40372,#40373,#40374,#40375,#40376,#40377,#40378,#40379,#40380,
#40381,#40382,#40383,#40384,#40385,#40386,#40387,#40388,#40389,#40390,#40391,
#40392,#40393,#40394,#40395,#40396,#40397,#40398),.UNSPECIFIED.,.F.,.F.)
B_SPLINE_CURVE_WITH_KNOTS((6,1,1,1,1,1,1,1,1,1,1,1,1,1,1,1,1,1,1,1,1,1,
1,1,1,1,1,1,1,1,1,1,1,1,1,1,1,1,1,1,1,1,1,1,1,1,1,1,1,1,1,1,1,1,1,1,1,1,
1,1,1,1,1,1,1,6),(-0.994228156739728,-0.984615384615383,-0.969230769230768,
-0.953846153846152,-0.938461538461537,-0.923076923076922,-0.907692307692306,
-0.892307692307691,-0.876923076923076,-0.86153846153846,-0.846153846153845,
-0.83076923076923,-0.815384615384614,-0.799999999999999,-0.784615384615384,
-0.769230769230768,-0.753846153846153,-0.738461538461538,-0.723076923076922,
-0.707692307692307,-0.692307692307692,-0.676923076923076,-0.661538461538461,
-0.646153846153846,-0.63076923076923,-0.615384615384615,-0.6,-0.584615384615384,
-0.569230769230769,-0.553846153846154,-0.538461538461538,-0.523076923076923,
-0.507692307692308,-0.492307692307692,-0.476923076923077,-0.461538461538462,
-0.446153846153846,-0.430769230769231,-0.415384615384615,-0.4,-0.384615384615385,
-0.369230769230769,-0.353846153846154,-0.338461538461538,-0.323076923076923,
-0.307692307692308,-0.292307692307692,-0.276923076923077,-0.261538461538462,
-0.246153846153846,-0.230769230769231,-0.215384615384615,-0.2,-0.184615384615385,
-0.169230769230769,-0.153846153846154,-0.138461538461538,-0.123076923076923,
-0.107692307692308,-0.0923076923076923,-0.0769230769230769,-0.0615384615384615,
-0.0461538461538462,-0.0307692307692308,-0.0153846153846154,0.),
 .UNSPECIFIED.)
CURVE()
GEOMETRIC_REPRESENTATION_ITEM()
RATIONAL_B_SPLINE_CURVE((1.,1.,1.,1.,1.,1.,1.,1.,1.,1.,1.,1.,1.,1.,1.,1.,
1.,1.,1.,1.,1.,1.,1.,1.,1.,1.,1.,1.,1.,1.,1.,1.,1.,1.,1.,1.,1.,1.,1.,1.,
1.,1.,1.,1.,1.,1.,1.,1.,1.,1.,1.,1.,1.,1.,1.,1.,1.,1.,1.,1.,1.,1.,1.,1.,
1.,1.,1.,1.,1.,1.))
REPRESENTATION_ITEM('')
);
#293=(
BOUNDED_CURVE()
B_SPLINE_CURVE(5,(#40551,#40552,#40553,#40554,#40555,#40556,#40557,#40558,
#40559,#40560,#40561,#40562,#40563,#40564,#40565,#40566,#40567,#40568,#40569,
#40570,#40571,#40572,#40573,#40574,#40575,#40576,#40577,#40578,#40579,#40580,
#40581,#40582,#40583,#40584,#40585,#40586,#40587,#40588,#40589,#40590,#40591,
#40592,#40593,#40594,#40595,#40596,#40597,#40598,#40599,#40600,#40601,#40602,
#40603,#40604,#40605,#40606,#40607,#40608,#40609,#40610,#40611,#40612,#40613,
#40614,#40615,#40616,#40617,#40618,#40619,#40620),.UNSPECIFIED.,.F.,.F.)
B_SPLINE_CURVE_WITH_KNOTS((6,1,1,1,1,1,1,1,1,1,1,1,1,1,1,1,1,1,1,1,1,1,
1,1,1,1,1,1,1,1,1,1,1,1,1,1,1,1,1,1,1,1,1,1,1,1,1,1,1,1,1,1,1,1,1,1,1,1,
1,1,1,1,1,1,1,6),(-1.,-0.984615384615383,-0.969230769230768,-0.953846153846152,
-0.938461538461537,-0.923076923076922,-0.907692307692306,-0.892307692307691,
-0.876923076923076,-0.86153846153846,-0.846153846153845,-0.83076923076923,
-0.815384615384614,-0.799999999999999,-0.784615384615384,-0.769230769230768,
-0.753846153846153,-0.738461538461538,-0.723076923076922,-0.707692307692307,
-0.692307692307692,-0.676923076923076,-0.661538461538461,-0.646153846153846,
-0.63076923076923,-0.615384615384615,-0.6,-0.584615384615384,-0.569230769230769,
-0.553846153846154,-0.538461538461538,-0.523076923076923,-0.507692307692308,
-0.492307692307692,-0.476923076923077,-0.461538461538462,-0.446153846153846,
-0.430769230769231,-0.415384615384615,-0.4,-0.384615384615385,-0.369230769230769,
-0.353846153846154,-0.338461538461538,-0.323076923076923,-0.307692307692308,
-0.292307692307692,-0.276923076923077,-0.261538461538462,-0.246153846153846,
-0.230769230769231,-0.215384615384615,-0.2,-0.184615384615385,-0.169230769230769,
-0.153846153846154,-0.138461538461538,-0.123076923076923,-0.107692307692308,
-0.0923076923076923,-0.0769230769230769,-0.0615384615384615,-0.0461538461538462,
-0.0307692307692308,-0.0153846153846154,-0.0057718433744926),
 .UNSPECIFIED.)
CURVE()
GEOMETRIC_REPRESENTATION_ITEM()
RATIONAL_B_SPLINE_CURVE((1.,1.,1.,1.,1.,1.,1.,1.,1.,1.,1.,1.,1.,1.,1.,1.,
1.,1.,1.,1.,1.,1.,1.,1.,1.,1.,1.,1.,1.,1.,1.,1.,1.,1.,1.,1.,1.,1.,1.,1.,
1.,1.,1.,1.,1.,1.,1.,1.,1.,1.,1.,1.,1.,1.,1.,1.,1.,1.,1.,1.,1.,1.,1.,1.,
1.,1.,1.,1.,1.,1.))
REPRESENTATION_ITEM('')
);
#294=(
BOUNDED_CURVE()
B_SPLINE_CURVE(5,(#40771,#40772,#40773,#40774,#40775,#40776,#40777,#40778,
#40779,#40780,#40781,#40782,#40783,#40784,#40785,#40786,#40787,#40788,#40789,
#40790,#40791,#40792,#40793,#40794,#40795,#40796,#40797,#40798,#40799,#40800,
#40801,#40802,#40803,#40804,#40805,#40806,#40807,#40808,#40809,#40810,#40811,
#40812,#40813,#40814,#40815,#40816,#40817,#40818,#40819,#40820,#40821,#40822,
#40823,#40824,#40825,#40826,#40827,#40828,#40829,#40830,#40831,#40832,#40833,
#40834,#40835,#40836,#40837,#40838,#40839,#40840),.UNSPECIFIED.,.F.,.F.)
B_SPLINE_CURVE_WITH_KNOTS((6,1,1,1,1,1,1,1,1,1,1,1,1,1,1,1,1,1,1,1,1,1,
1,1,1,1,1,1,1,1,1,1,1,1,1,1,1,1,1,1,1,1,1,1,1,1,1,1,1,1,1,1,1,1,1,1,1,1,
1,1,1,1,1,1,1,6),(-0.994228156739718,-0.984615384615383,-0.969230769230768,
-0.953846153846152,-0.938461538461537,-0.923076923076922,-0.907692307692306,
-0.892307692307691,-0.876923076923076,-0.86153846153846,-0.846153846153845,
-0.83076923076923,-0.815384615384614,-0.799999999999999,-0.784615384615384,
-0.769230769230768,-0.753846153846153,-0.738461538461538,-0.723076923076922,
-0.707692307692307,-0.692307692307692,-0.676923076923076,-0.661538461538461,
-0.646153846153846,-0.63076923076923,-0.615384615384615,-0.6,-0.584615384615384,
-0.569230769230769,-0.553846153846154,-0.538461538461538,-0.523076923076923,
-0.507692307692308,-0.492307692307692,-0.476923076923077,-0.461538461538462,
-0.446153846153846,-0.430769230769231,-0.415384615384615,-0.4,-0.384615384615385,
-0.369230769230769,-0.353846153846154,-0.338461538461538,-0.323076923076923,
-0.307692307692308,-0.292307692307692,-0.276923076923077,-0.261538461538462,
-0.246153846153846,-0.230769230769231,-0.215384615384615,-0.2,-0.184615384615385,
-0.169230769230769,-0.153846153846154,-0.138461538461538,-0.123076923076923,
-0.107692307692308,-0.0923076923076923,-0.0769230769230769,-0.0615384615384615,
-0.0461538461538462,-0.0307692307692308,-0.0153846153846154,0.),
 .UNSPECIFIED.)
CURVE()
GEOMETRIC_REPRESENTATION_ITEM()
RATIONAL_B_SPLINE_CURVE((1.,1.,1.,1.,1.,1.,1.,1.,1.,1.,1.,1.,1.,1.,1.,1.,
1.,1.,1.,1.,1.,1.,1.,1.,1.,1.,1.,1.,1.,1.,1.,1.,1.,1.,1.,1.,1.,1.,1.,1.,
1.,1.,1.,1.,1.,1.,1.,1.,1.,1.,1.,1.,1.,1.,1.,1.,1.,1.,1.,1.,1.,1.,1.,1.,
1.,1.,1.,1.,1.,1.))
REPRESENTATION_ITEM('')
);
#295=(
BOUNDED_CURVE()
B_SPLINE_CURVE(5,(#40993,#40994,#40995,#40996,#40997,#40998,#40999,#41000,
#41001,#41002,#41003,#41004,#41005,#41006,#41007,#41008,#41009,#41010,#41011,
#41012,#41013,#41014,#41015,#41016,#41017,#41018,#41019,#41020,#41021,#41022,
#41023,#41024,#41025,#41026,#41027,#41028,#41029,#41030,#41031,#41032,#41033,
#41034,#41035,#41036,#41037,#41038,#41039,#41040,#41041,#41042,#41043,#41044,
#41045,#41046,#41047,#41048,#41049,#41050,#41051,#41052,#41053,#41054,#41055,
#41056,#41057,#41058,#41059,#41060,#41061,#41062),.UNSPECIFIED.,.F.,.F.)
B_SPLINE_CURVE_WITH_KNOTS((6,1,1,1,1,1,1,1,1,1,1,1,1,1,1,1,1,1,1,1,1,1,
1,1,1,1,1,1,1,1,1,1,1,1,1,1,1,1,1,1,1,1,1,1,1,1,1,1,1,1,1,1,1,1,1,1,1,1,
1,1,1,1,1,1,1,6),(-1.,-0.984615384615383,-0.969230769230768,-0.953846153846152,
-0.938461538461537,-0.923076923076922,-0.907692307692306,-0.892307692307691,
-0.876923076923076,-0.86153846153846,-0.846153846153845,-0.83076923076923,
-0.815384615384614,-0.799999999999999,-0.784615384615384,-0.769230769230768,
-0.753846153846153,-0.738461538461538,-0.723076923076922,-0.707692307692307,
-0.692307692307692,-0.676923076923076,-0.661538461538461,-0.646153846153846,
-0.63076923076923,-0.615384615384615,-0.6,-0.584615384615384,-0.569230769230769,
-0.553846153846154,-0.538461538461538,-0.523076923076923,-0.507692307692308,
-0.492307692307692,-0.476923076923077,-0.461538461538462,-0.446153846153846,
-0.430769230769231,-0.415384615384615,-0.4,-0.384615384615385,-0.369230769230769,
-0.353846153846154,-0.338461538461538,-0.323076923076923,-0.307692307692308,
-0.292307692307692,-0.276923076923077,-0.261538461538462,-0.246153846153846,
-0.230769230769231,-0.215384615384615,-0.2,-0.184615384615385,-0.169230769230769,
-0.153846153846154,-0.138461538461538,-0.123076923076923,-0.107692307692308,
-0.0923076923076923,-0.0769230769230769,-0.0615384615384615,-0.0461538461538462,
-0.0307692307692308,-0.0153846153846154,-0.00577184337449396),
 .UNSPECIFIED.)
CURVE()
GEOMETRIC_REPRESENTATION_ITEM()
RATIONAL_B_SPLINE_CURVE((1.,1.,1.,1.,1.,1.,1.,1.,1.,1.,1.,1.,1.,1.,1.,1.,
1.,1.,1.,1.,1.,1.,1.,1.,1.,1.,1.,1.,1.,1.,1.,1.,1.,1.,1.,1.,1.,1.,1.,1.,
1.,1.,1.,1.,1.,1.,1.,1.,1.,1.,1.,1.,1.,1.,1.,1.,1.,1.,1.,1.,1.,1.,1.,1.,
1.,1.,1.,1.,1.,1.))
REPRESENTATION_ITEM('')
);
#296=(
BOUNDED_CURVE()
B_SPLINE_CURVE(5,(#41213,#41214,#41215,#41216,#41217,#41218,#41219,#41220,
#41221,#41222,#41223,#41224,#41225,#41226,#41227,#41228,#41229,#41230,#41231,
#41232,#41233,#41234,#41235,#41236,#41237,#41238,#41239,#41240,#41241,#41242,
#41243,#41244,#41245,#41246,#41247,#41248,#41249,#41250,#41251,#41252,#41253,
#41254,#41255,#41256,#41257,#41258,#41259,#41260,#41261,#41262,#41263,#41264,
#41265,#41266,#41267,#41268,#41269,#41270,#41271,#41272,#41273,#41274,#41275,
#41276,#41277,#41278,#41279,#41280,#41281,#41282),.UNSPECIFIED.,.F.,.F.)
B_SPLINE_CURVE_WITH_KNOTS((6,1,1,1,1,1,1,1,1,1,1,1,1,1,1,1,1,1,1,1,1,1,
1,1,1,1,1,1,1,1,1,1,1,1,1,1,1,1,1,1,1,1,1,1,1,1,1,1,1,1,1,1,1,1,1,1,1,1,
1,1,1,1,1,1,1,6),(-0.994228156739702,-0.984615384615383,-0.969230769230768,
-0.953846153846152,-0.938461538461537,-0.923076923076922,-0.907692307692306,
-0.892307692307691,-0.876923076923076,-0.86153846153846,-0.846153846153845,
-0.83076923076923,-0.815384615384614,-0.799999999999999,-0.784615384615384,
-0.769230769230768,-0.753846153846153,-0.738461538461538,-0.723076923076922,
-0.707692307692307,-0.692307692307692,-0.676923076923076,-0.661538461538461,
-0.646153846153846,-0.63076923076923,-0.615384615384615,-0.6,-0.584615384615384,
-0.569230769230769,-0.553846153846154,-0.538461538461538,-0.523076923076923,
-0.507692307692308,-0.492307692307692,-0.476923076923077,-0.461538461538462,
-0.446153846153846,-0.430769230769231,-0.415384615384615,-0.4,-0.384615384615385,
-0.369230769230769,-0.353846153846154,-0.338461538461538,-0.323076923076923,
-0.307692307692308,-0.292307692307692,-0.276923076923077,-0.261538461538462,
-0.246153846153846,-0.230769230769231,-0.215384615384615,-0.2,-0.184615384615385,
-0.169230769230769,-0.153846153846154,-0.138461538461538,-0.123076923076923,
-0.107692307692308,-0.0923076923076923,-0.0769230769230769,-0.0615384615384615,
-0.0461538461538462,-0.0307692307692308,-0.0153846153846154,0.),
 .UNSPECIFIED.)
CURVE()
GEOMETRIC_REPRESENTATION_ITEM()
RATIONAL_B_SPLINE_CURVE((1.,1.,1.,1.,1.,1.,1.,1.,1.,1.,1.,1.,1.,1.,1.,1.,
1.,1.,1.,1.,1.,1.,1.,1.,1.,1.,1.,1.,1.,1.,1.,1.,1.,1.,1.,1.,1.,1.,1.,1.,
1.,1.,1.,1.,1.,1.,1.,1.,1.,1.,1.,1.,1.,1.,1.,1.,1.,1.,1.,1.,1.,1.,1.,1.,
1.,1.,1.,1.,1.,1.))
REPRESENTATION_ITEM('')
);
#297=(
BOUNDED_CURVE()
B_SPLINE_CURVE(5,(#41435,#41436,#41437,#41438,#41439,#41440,#41441,#41442,
#41443,#41444,#41445,#41446,#41447,#41448,#41449,#41450,#41451,#41452,#41453,
#41454,#41455,#41456,#41457,#41458,#41459,#41460,#41461,#41462,#41463,#41464,
#41465,#41466,#41467,#41468,#41469,#41470,#41471,#41472,#41473,#41474,#41475,
#41476,#41477,#41478,#41479,#41480,#41481,#41482,#41483,#41484,#41485,#41486,
#41487,#41488,#41489,#41490,#41491,#41492,#41493,#41494,#41495,#41496,#41497,
#41498,#41499,#41500,#41501,#41502,#41503,#41504),.UNSPECIFIED.,.F.,.F.)
B_SPLINE_CURVE_WITH_KNOTS((6,1,1,1,1,1,1,1,1,1,1,1,1,1,1,1,1,1,1,1,1,1,
1,1,1,1,1,1,1,1,1,1,1,1,1,1,1,1,1,1,1,1,1,1,1,1,1,1,1,1,1,1,1,1,1,1,1,1,
1,1,1,1,1,1,1,6),(-1.,-0.984615384615383,-0.969230769230768,-0.953846153846152,
-0.938461538461537,-0.923076923076922,-0.907692307692306,-0.892307692307691,
-0.876923076923076,-0.86153846153846,-0.846153846153845,-0.83076923076923,
-0.815384615384614,-0.799999999999999,-0.784615384615384,-0.769230769230768,
-0.753846153846153,-0.738461538461538,-0.723076923076922,-0.707692307692307,
-0.692307692307692,-0.676923076923076,-0.661538461538461,-0.646153846153846,
-0.63076923076923,-0.615384615384615,-0.6,-0.584615384615384,-0.569230769230769,
-0.553846153846154,-0.538461538461538,-0.523076923076923,-0.507692307692308,
-0.492307692307692,-0.476923076923077,-0.461538461538462,-0.446153846153846,
-0.430769230769231,-0.415384615384615,-0.4,-0.384615384615385,-0.369230769230769,
-0.353846153846154,-0.338461538461538,-0.323076923076923,-0.307692307692308,
-0.292307692307692,-0.276923076923077,-0.261538461538462,-0.246153846153846,
-0.230769230769231,-0.215384615384615,-0.2,-0.184615384615385,-0.169230769230769,
-0.153846153846154,-0.138461538461538,-0.123076923076923,-0.107692307692308,
-0.0923076923076923,-0.0769230769230769,-0.0615384615384615,-0.0461538461538462,
-0.0307692307692308,-0.0153846153846154,-0.00577184337450989),
 .UNSPECIFIED.)
CURVE()
GEOMETRIC_REPRESENTATION_ITEM()
RATIONAL_B_SPLINE_CURVE((1.,1.,1.,1.,1.,1.,1.,1.,1.,1.,1.,1.,1.,1.,1.,1.,
1.,1.,1.,1.,1.,1.,1.,1.,1.,1.,1.,1.,1.,1.,1.,1.,1.,1.,1.,1.,1.,1.,1.,1.,
1.,1.,1.,1.,1.,1.,1.,1.,1.,1.,1.,1.,1.,1.,1.,1.,1.,1.,1.,1.,1.,1.,1.,1.,
1.,1.,1.,1.,1.,1.))
REPRESENTATION_ITEM('')
);
#298=(
BOUNDED_CURVE()
B_SPLINE_CURVE(5,(#41655,#41656,#41657,#41658,#41659,#41660,#41661,#41662,
#41663,#41664,#41665,#41666,#41667,#41668,#41669,#41670,#41671,#41672,#41673,
#41674,#41675,#41676,#41677,#41678,#41679,#41680,#41681,#41682,#41683,#41684,
#41685,#41686,#41687,#41688,#41689,#41690,#41691,#41692,#41693,#41694,#41695,
#41696,#41697,#41698,#41699,#41700,#41701,#41702,#41703,#41704,#41705,#41706,
#41707,#41708,#41709,#41710,#41711,#41712,#41713,#41714,#41715,#41716,#41717,
#41718,#41719,#41720,#41721,#41722,#41723,#41724),.UNSPECIFIED.,.F.,.F.)
B_SPLINE_CURVE_WITH_KNOTS((6,1,1,1,1,1,1,1,1,1,1,1,1,1,1,1,1,1,1,1,1,1,
1,1,1,1,1,1,1,1,1,1,1,1,1,1,1,1,1,1,1,1,1,1,1,1,1,1,1,1,1,1,1,1,1,1,1,1,
1,1,1,1,1,1,1,6),(-0.994228156739736,-0.984615384615383,-0.969230769230768,
-0.953846153846152,-0.938461538461537,-0.923076923076922,-0.907692307692306,
-0.892307692307691,-0.876923076923076,-0.86153846153846,-0.846153846153845,
-0.83076923076923,-0.815384615384614,-0.799999999999999,-0.784615384615384,
-0.769230769230768,-0.753846153846153,-0.738461538461538,-0.723076923076922,
-0.707692307692307,-0.692307692307692,-0.676923076923076,-0.661538461538461,
-0.646153846153846,-0.63076923076923,-0.615384615384615,-0.6,-0.584615384615384,
-0.569230769230769,-0.553846153846154,-0.538461538461538,-0.523076923076923,
-0.507692307692308,-0.492307692307692,-0.476923076923077,-0.461538461538462,
-0.446153846153846,-0.430769230769231,-0.415384615384615,-0.4,-0.384615384615385,
-0.369230769230769,-0.353846153846154,-0.338461538461538,-0.323076923076923,
-0.307692307692308,-0.292307692307692,-0.276923076923077,-0.261538461538462,
-0.246153846153846,-0.230769230769231,-0.215384615384615,-0.2,-0.184615384615385,
-0.169230769230769,-0.153846153846154,-0.138461538461538,-0.123076923076923,
-0.107692307692308,-0.0923076923076923,-0.0769230769230769,-0.0615384615384615,
-0.0461538461538462,-0.0307692307692308,-0.0153846153846154,0.),
 .UNSPECIFIED.)
CURVE()
GEOMETRIC_REPRESENTATION_ITEM()
RATIONAL_B_SPLINE_CURVE((1.,1.,1.,1.,1.,1.,1.,1.,1.,1.,1.,1.,1.,1.,1.,1.,
1.,1.,1.,1.,1.,1.,1.,1.,1.,1.,1.,1.,1.,1.,1.,1.,1.,1.,1.,1.,1.,1.,1.,1.,
1.,1.,1.,1.,1.,1.,1.,1.,1.,1.,1.,1.,1.,1.,1.,1.,1.,1.,1.,1.,1.,1.,1.,1.,
1.,1.,1.,1.,1.,1.))
REPRESENTATION_ITEM('')
);
#299=(
BOUNDED_CURVE()
B_SPLINE_CURVE(5,(#41877,#41878,#41879,#41880,#41881,#41882,#41883,#41884,
#41885,#41886,#41887,#41888,#41889,#41890,#41891,#41892,#41893,#41894,#41895,
#41896,#41897,#41898,#41899,#41900,#41901,#41902,#41903,#41904,#41905,#41906,
#41907,#41908,#41909,#41910,#41911,#41912,#41913,#41914,#41915,#41916,#41917,
#41918,#41919,#41920,#41921,#41922,#41923,#41924,#41925,#41926,#41927,#41928,
#41929,#41930,#41931,#41932,#41933,#41934,#41935,#41936,#41937,#41938,#41939,
#41940,#41941,#41942,#41943,#41944,#41945,#41946),.UNSPECIFIED.,.F.,.F.)
B_SPLINE_CURVE_WITH_KNOTS((6,1,1,1,1,1,1,1,1,1,1,1,1,1,1,1,1,1,1,1,1,1,
1,1,1,1,1,1,1,1,1,1,1,1,1,1,1,1,1,1,1,1,1,1,1,1,1,1,1,1,1,1,1,1,1,1,1,1,
1,1,1,1,1,1,1,6),(-1.,-0.984615384615383,-0.969230769230768,-0.953846153846152,
-0.938461538461537,-0.923076923076922,-0.907692307692306,-0.892307692307691,
-0.876923076923076,-0.86153846153846,-0.846153846153845,-0.83076923076923,
-0.815384615384614,-0.799999999999999,-0.784615384615384,-0.769230769230768,
-0.753846153846153,-0.738461538461538,-0.723076923076922,-0.707692307692307,
-0.692307692307692,-0.676923076923076,-0.661538461538461,-0.646153846153846,
-0.63076923076923,-0.615384615384615,-0.6,-0.584615384615384,-0.569230769230769,
-0.553846153846154,-0.538461538461538,-0.523076923076923,-0.507692307692308,
-0.492307692307692,-0.476923076923077,-0.461538461538462,-0.446153846153846,
-0.430769230769231,-0.415384615384615,-0.4,-0.384615384615385,-0.369230769230769,
-0.353846153846154,-0.338461538461538,-0.323076923076923,-0.307692307692308,
-0.292307692307692,-0.276923076923077,-0.261538461538462,-0.246153846153846,
-0.230769230769231,-0.215384615384615,-0.2,-0.184615384615385,-0.169230769230769,
-0.153846153846154,-0.138461538461538,-0.123076923076923,-0.107692307692308,
-0.0923076923076923,-0.0769230769230769,-0.0615384615384615,-0.0461538461538462,
-0.0307692307692308,-0.0153846153846154,-0.00577184337452469),
 .UNSPECIFIED.)
CURVE()
GEOMETRIC_REPRESENTATION_ITEM()
RATIONAL_B_SPLINE_CURVE((1.,1.,1.,1.,1.,1.,1.,1.,1.,1.,1.,1.,1.,1.,1.,1.,
1.,1.,1.,1.,1.,1.,1.,1.,1.,1.,1.,1.,1.,1.,1.,1.,1.,1.,1.,1.,1.,1.,1.,1.,
1.,1.,1.,1.,1.,1.,1.,1.,1.,1.,1.,1.,1.,1.,1.,1.,1.,1.,1.,1.,1.,1.,1.,1.,
1.,1.,1.,1.,1.,1.))
REPRESENTATION_ITEM('')
);
#300=(
BOUNDED_CURVE()
B_SPLINE_CURVE(5,(#42097,#42098,#42099,#42100,#42101,#42102,#42103,#42104,
#42105,#42106,#42107,#42108,#42109,#42110,#42111,#42112,#42113,#42114,#42115,
#42116,#42117,#42118,#42119,#42120,#42121,#42122,#42123,#42124,#42125,#42126,
#42127,#42128,#42129,#42130,#42131,#42132,#42133,#42134,#42135,#42136,#42137,
#42138,#42139,#42140,#42141,#42142,#42143,#42144,#42145,#42146,#42147,#42148,
#42149,#42150,#42151,#42152,#42153,#42154,#42155,#42156,#42157,#42158,#42159,
#42160,#42161,#42162,#42163,#42164,#42165,#42166),.UNSPECIFIED.,.F.,.F.)
B_SPLINE_CURVE_WITH_KNOTS((6,1,1,1,1,1,1,1,1,1,1,1,1,1,1,1,1,1,1,1,1,1,
1,1,1,1,1,1,1,1,1,1,1,1,1,1,1,1,1,1,1,1,1,1,1,1,1,1,1,1,1,1,1,1,1,1,1,1,
1,1,1,1,1,1,1,6),(-0.994228156739717,-0.984615384615383,-0.969230769230768,
-0.953846153846152,-0.938461538461537,-0.923076923076922,-0.907692307692306,
-0.892307692307691,-0.876923076923076,-0.86153846153846,-0.846153846153845,
-0.83076923076923,-0.815384615384614,-0.799999999999999,-0.784615384615384,
-0.769230769230768,-0.753846153846153,-0.738461538461538,-0.723076923076922,
-0.707692307692307,-0.692307692307692,-0.676923076923076,-0.661538461538461,
-0.646153846153846,-0.63076923076923,-0.615384615384615,-0.6,-0.584615384615384,
-0.569230769230769,-0.553846153846154,-0.538461538461538,-0.523076923076923,
-0.507692307692308,-0.492307692307692,-0.476923076923077,-0.461538461538462,
-0.446153846153846,-0.430769230769231,-0.415384615384615,-0.4,-0.384615384615385,
-0.369230769230769,-0.353846153846154,-0.338461538461538,-0.323076923076923,
-0.307692307692308,-0.292307692307692,-0.276923076923077,-0.261538461538462,
-0.246153846153846,-0.230769230769231,-0.215384615384615,-0.2,-0.184615384615385,
-0.169230769230769,-0.153846153846154,-0.138461538461538,-0.123076923076923,
-0.107692307692308,-0.0923076923076923,-0.0769230769230769,-0.0615384615384615,
-0.0461538461538462,-0.0307692307692308,-0.0153846153846154,0.),
 .UNSPECIFIED.)
CURVE()
GEOMETRIC_REPRESENTATION_ITEM()
RATIONAL_B_SPLINE_CURVE((1.,1.,1.,1.,1.,1.,1.,1.,1.,1.,1.,1.,1.,1.,1.,1.,
1.,1.,1.,1.,1.,1.,1.,1.,1.,1.,1.,1.,1.,1.,1.,1.,1.,1.,1.,1.,1.,1.,1.,1.,
1.,1.,1.,1.,1.,1.,1.,1.,1.,1.,1.,1.,1.,1.,1.,1.,1.,1.,1.,1.,1.,1.,1.,1.,
1.,1.,1.,1.,1.,1.))
REPRESENTATION_ITEM('')
);
#301=(
BOUNDED_CURVE()
B_SPLINE_CURVE(5,(#42319,#42320,#42321,#42322,#42323,#42324,#42325,#42326,
#42327,#42328,#42329,#42330,#42331,#42332,#42333,#42334,#42335,#42336,#42337,
#42338,#42339,#42340,#42341,#42342,#42343,#42344,#42345,#42346,#42347,#42348,
#42349,#42350,#42351,#42352,#42353,#42354,#42355,#42356,#42357,#42358,#42359,
#42360,#42361,#42362,#42363,#42364,#42365,#42366,#42367,#42368,#42369,#42370,
#42371,#42372,#42373,#42374,#42375,#42376,#42377,#42378,#42379,#42380,#42381,
#42382,#42383,#42384,#42385,#42386,#42387,#42388),.UNSPECIFIED.,.F.,.F.)
B_SPLINE_CURVE_WITH_KNOTS((6,1,1,1,1,1,1,1,1,1,1,1,1,1,1,1,1,1,1,1,1,1,
1,1,1,1,1,1,1,1,1,1,1,1,1,1,1,1,1,1,1,1,1,1,1,1,1,1,1,1,1,1,1,1,1,1,1,1,
1,1,1,1,1,1,1,6),(-1.,-0.984615384615383,-0.969230769230768,-0.953846153846152,
-0.938461538461537,-0.923076923076922,-0.907692307692306,-0.892307692307691,
-0.876923076923076,-0.86153846153846,-0.846153846153845,-0.83076923076923,
-0.815384615384614,-0.799999999999999,-0.784615384615384,-0.769230769230768,
-0.753846153846153,-0.738461538461538,-0.723076923076922,-0.707692307692307,
-0.692307692307692,-0.676923076923076,-0.661538461538461,-0.646153846153846,
-0.63076923076923,-0.615384615384615,-0.6,-0.584615384615384,-0.569230769230769,
-0.553846153846154,-0.538461538461538,-0.523076923076923,-0.507692307692308,
-0.492307692307692,-0.476923076923077,-0.461538461538462,-0.446153846153846,
-0.430769230769231,-0.415384615384615,-0.4,-0.384615384615385,-0.369230769230769,
-0.353846153846154,-0.338461538461538,-0.323076923076923,-0.307692307692308,
-0.292307692307692,-0.276923076923077,-0.261538461538462,-0.246153846153846,
-0.230769230769231,-0.215384615384615,-0.2,-0.184615384615385,-0.169230769230769,
-0.153846153846154,-0.138461538461538,-0.123076923076923,-0.107692307692308,
-0.0923076923076923,-0.0769230769230769,-0.0615384615384615,-0.0461538461538462,
-0.0307692307692308,-0.0153846153846154,-0.00577184337453472),
 .UNSPECIFIED.)
CURVE()
GEOMETRIC_REPRESENTATION_ITEM()
RATIONAL_B_SPLINE_CURVE((1.,1.,1.,1.,1.,1.,1.,1.,1.,1.,1.,1.,1.,1.,1.,1.,
1.,1.,1.,1.,1.,1.,1.,1.,1.,1.,1.,1.,1.,1.,1.,1.,1.,1.,1.,1.,1.,1.,1.,1.,
1.,1.,1.,1.,1.,1.,1.,1.,1.,1.,1.,1.,1.,1.,1.,1.,1.,1.,1.,1.,1.,1.,1.,1.,
1.,1.,1.,1.,1.,1.))
REPRESENTATION_ITEM('')
);
#302=(
BOUNDED_CURVE()
B_SPLINE_CURVE(5,(#42539,#42540,#42541,#42542,#42543,#42544,#42545,#42546,
#42547,#42548,#42549,#42550,#42551,#42552,#42553,#42554,#42555,#42556,#42557,
#42558,#42559,#42560,#42561,#42562,#42563,#42564,#42565,#42566,#42567,#42568,
#42569,#42570,#42571,#42572,#42573,#42574,#42575,#42576,#42577,#42578,#42579,
#42580,#42581,#42582,#42583,#42584,#42585,#42586,#42587,#42588,#42589,#42590,
#42591,#42592,#42593,#42594,#42595,#42596,#42597,#42598,#42599,#42600,#42601,
#42602,#42603,#42604,#42605,#42606,#42607,#42608),.UNSPECIFIED.,.F.,.F.)
B_SPLINE_CURVE_WITH_KNOTS((6,1,1,1,1,1,1,1,1,1,1,1,1,1,1,1,1,1,1,1,1,1,
1,1,1,1,1,1,1,1,1,1,1,1,1,1,1,1,1,1,1,1,1,1,1,1,1,1,1,1,1,1,1,1,1,1,1,1,
1,1,1,1,1,1,1,6),(-0.994228156739652,-0.984615384615383,-0.969230769230768,
-0.953846153846152,-0.938461538461537,-0.923076923076922,-0.907692307692306,
-0.892307692307691,-0.876923076923076,-0.86153846153846,-0.846153846153845,
-0.83076923076923,-0.815384615384614,-0.799999999999999,-0.784615384615384,
-0.769230769230768,-0.753846153846153,-0.738461538461538,-0.723076923076922,
-0.707692307692307,-0.692307692307692,-0.676923076923076,-0.661538461538461,
-0.646153846153846,-0.63076923076923,-0.615384615384615,-0.6,-0.584615384615384,
-0.569230769230769,-0.553846153846154,-0.538461538461538,-0.523076923076923,
-0.507692307692308,-0.492307692307692,-0.476923076923077,-0.461538461538462,
-0.446153846153846,-0.430769230769231,-0.415384615384615,-0.4,-0.384615384615385,
-0.369230769230769,-0.353846153846154,-0.338461538461538,-0.323076923076923,
-0.307692307692308,-0.292307692307692,-0.276923076923077,-0.261538461538462,
-0.246153846153846,-0.230769230769231,-0.215384615384615,-0.2,-0.184615384615385,
-0.169230769230769,-0.153846153846154,-0.138461538461538,-0.123076923076923,
-0.107692307692308,-0.0923076923076923,-0.0769230769230769,-0.0615384615384615,
-0.0461538461538462,-0.0307692307692308,-0.0153846153846154,0.),
 .UNSPECIFIED.)
CURVE()
GEOMETRIC_REPRESENTATION_ITEM()
RATIONAL_B_SPLINE_CURVE((1.,1.,1.,1.,1.,1.,1.,1.,1.,1.,1.,1.,1.,1.,1.,1.,
1.,1.,1.,1.,1.,1.,1.,1.,1.,1.,1.,1.,1.,1.,1.,1.,1.,1.,1.,1.,1.,1.,1.,1.,
1.,1.,1.,1.,1.,1.,1.,1.,1.,1.,1.,1.,1.,1.,1.,1.,1.,1.,1.,1.,1.,1.,1.,1.,
1.,1.,1.,1.,1.,1.))
REPRESENTATION_ITEM('')
);
#303=(
BOUNDED_CURVE()
B_SPLINE_CURVE(5,(#42761,#42762,#42763,#42764,#42765,#42766,#42767,#42768,
#42769,#42770,#42771,#42772,#42773,#42774,#42775,#42776,#42777,#42778,#42779,
#42780,#42781,#42782,#42783,#42784,#42785,#42786,#42787,#42788,#42789,#42790,
#42791,#42792,#42793,#42794,#42795,#42796,#42797,#42798,#42799,#42800,#42801,
#42802,#42803,#42804,#42805,#42806,#42807,#42808,#42809,#42810,#42811,#42812,
#42813,#42814,#42815,#42816,#42817,#42818,#42819,#42820,#42821,#42822,#42823,
#42824,#42825,#42826,#42827,#42828,#42829,#42830),.UNSPECIFIED.,.F.,.F.)
B_SPLINE_CURVE_WITH_KNOTS((6,1,1,1,1,1,1,1,1,1,1,1,1,1,1,1,1,1,1,1,1,1,
1,1,1,1,1,1,1,1,1,1,1,1,1,1,1,1,1,1,1,1,1,1,1,1,1,1,1,1,1,1,1,1,1,1,1,1,
1,1,1,1,1,1,1,6),(-1.,-0.984615384615383,-0.969230769230768,-0.953846153846152,
-0.938461538461537,-0.923076923076922,-0.907692307692306,-0.892307692307691,
-0.876923076923076,-0.86153846153846,-0.846153846153845,-0.83076923076923,
-0.815384615384614,-0.799999999999999,-0.784615384615384,-0.769230769230768,
-0.753846153846153,-0.738461538461538,-0.723076923076922,-0.707692307692307,
-0.692307692307692,-0.676923076923076,-0.661538461538461,-0.646153846153846,
-0.63076923076923,-0.615384615384615,-0.6,-0.584615384615384,-0.569230769230769,
-0.553846153846154,-0.538461538461538,-0.523076923076923,-0.507692307692308,
-0.492307692307692,-0.476923076923077,-0.461538461538462,-0.446153846153846,
-0.430769230769231,-0.415384615384615,-0.4,-0.384615384615385,-0.369230769230769,
-0.353846153846154,-0.338461538461538,-0.323076923076923,-0.307692307692308,
-0.292307692307692,-0.276923076923077,-0.261538461538462,-0.246153846153846,
-0.230769230769231,-0.215384615384615,-0.2,-0.184615384615385,-0.169230769230769,
-0.153846153846154,-0.138461538461538,-0.123076923076923,-0.107692307692308,
-0.0923076923076923,-0.0769230769230769,-0.0615384615384615,-0.0461538461538462,
-0.0307692307692308,-0.0153846153846154,-0.00577184337450876),
 .UNSPECIFIED.)
CURVE()
GEOMETRIC_REPRESENTATION_ITEM()
RATIONAL_B_SPLINE_CURVE((1.,1.,1.,1.,1.,1.,1.,1.,1.,1.,1.,1.,1.,1.,1.,1.,
1.,1.,1.,1.,1.,1.,1.,1.,1.,1.,1.,1.,1.,1.,1.,1.,1.,1.,1.,1.,1.,1.,1.,1.,
1.,1.,1.,1.,1.,1.,1.,1.,1.,1.,1.,1.,1.,1.,1.,1.,1.,1.,1.,1.,1.,1.,1.,1.,
1.,1.,1.,1.,1.,1.))
REPRESENTATION_ITEM('')
);
#304=(
BOUNDED_CURVE()
B_SPLINE_CURVE(5,(#42981,#42982,#42983,#42984,#42985,#42986,#42987,#42988,
#42989,#42990,#42991,#42992,#42993,#42994,#42995,#42996,#42997,#42998,#42999,
#43000,#43001,#43002,#43003,#43004,#43005,#43006,#43007,#43008,#43009,#43010,
#43011,#43012,#43013,#43014,#43015,#43016,#43017,#43018,#43019,#43020,#43021,
#43022,#43023,#43024,#43025,#43026,#43027,#43028,#43029,#43030,#43031,#43032,
#43033,#43034,#43035,#43036,#43037,#43038,#43039,#43040,#43041,#43042,#43043,
#43044,#43045,#43046,#43047,#43048,#43049,#43050),.UNSPECIFIED.,.F.,.F.)
B_SPLINE_CURVE_WITH_KNOTS((6,1,1,1,1,1,1,1,1,1,1,1,1,1,1,1,1,1,1,1,1,1,
1,1,1,1,1,1,1,1,1,1,1,1,1,1,1,1,1,1,1,1,1,1,1,1,1,1,1,1,1,1,1,1,1,1,1,1,
1,1,1,1,1,1,1,6),(-0.994228156739683,-0.984615384615383,-0.969230769230768,
-0.953846153846152,-0.938461538461537,-0.923076923076922,-0.907692307692306,
-0.892307692307691,-0.876923076923076,-0.86153846153846,-0.846153846153845,
-0.83076923076923,-0.815384615384614,-0.799999999999999,-0.784615384615384,
-0.769230769230768,-0.753846153846153,-0.738461538461538,-0.723076923076922,
-0.707692307692307,-0.692307692307692,-0.676923076923076,-0.661538461538461,
-0.646153846153846,-0.63076923076923,-0.615384615384615,-0.6,-0.584615384615384,
-0.569230769230769,-0.553846153846154,-0.538461538461538,-0.523076923076923,
-0.507692307692308,-0.492307692307692,-0.476923076923077,-0.461538461538462,
-0.446153846153846,-0.430769230769231,-0.415384615384615,-0.4,-0.384615384615385,
-0.369230769230769,-0.353846153846154,-0.338461538461538,-0.323076923076923,
-0.307692307692308,-0.292307692307692,-0.276923076923077,-0.261538461538462,
-0.246153846153846,-0.230769230769231,-0.215384615384615,-0.2,-0.184615384615385,
-0.169230769230769,-0.153846153846154,-0.138461538461538,-0.123076923076923,
-0.107692307692308,-0.0923076923076923,-0.0769230769230769,-0.0615384615384615,
-0.0461538461538462,-0.0307692307692308,-0.0153846153846154,0.),
 .UNSPECIFIED.)
CURVE()
GEOMETRIC_REPRESENTATION_ITEM()
RATIONAL_B_SPLINE_CURVE((1.,1.,1.,1.,1.,1.,1.,1.,1.,1.,1.,1.,1.,1.,1.,1.,
1.,1.,1.,1.,1.,1.,1.,1.,1.,1.,1.,1.,1.,1.,1.,1.,1.,1.,1.,1.,1.,1.,1.,1.,
1.,1.,1.,1.,1.,1.,1.,1.,1.,1.,1.,1.,1.,1.,1.,1.,1.,1.,1.,1.,1.,1.,1.,1.,
1.,1.,1.,1.,1.,1.))
REPRESENTATION_ITEM('')
);
#305=(
BOUNDED_CURVE()
B_SPLINE_CURVE(5,(#43203,#43204,#43205,#43206,#43207,#43208,#43209,#43210,
#43211,#43212,#43213,#43214,#43215,#43216,#43217,#43218,#43219,#43220,#43221,
#43222,#43223,#43224,#43225,#43226,#43227,#43228,#43229,#43230,#43231,#43232,
#43233,#43234,#43235,#43236,#43237,#43238,#43239,#43240,#43241,#43242,#43243,
#43244,#43245,#43246,#43247,#43248,#43249,#43250,#43251,#43252,#43253,#43254,
#43255,#43256,#43257,#43258,#43259,#43260,#43261,#43262,#43263,#43264,#43265,
#43266,#43267,#43268,#43269,#43270,#43271,#43272),.UNSPECIFIED.,.F.,.F.)
B_SPLINE_CURVE_WITH_KNOTS((6,1,1,1,1,1,1,1,1,1,1,1,1,1,1,1,1,1,1,1,1,1,
1,1,1,1,1,1,1,1,1,1,1,1,1,1,1,1,1,1,1,1,1,1,1,1,1,1,1,1,1,1,1,1,1,1,1,1,
1,1,1,1,1,1,1,6),(-1.,-0.984615384615383,-0.969230769230768,-0.953846153846152,
-0.938461538461537,-0.923076923076922,-0.907692307692306,-0.892307692307691,
-0.876923076923076,-0.86153846153846,-0.846153846153845,-0.83076923076923,
-0.815384615384614,-0.799999999999999,-0.784615384615384,-0.769230769230768,
-0.753846153846153,-0.738461538461538,-0.723076923076922,-0.707692307692307,
-0.692307692307692,-0.676923076923076,-0.661538461538461,-0.646153846153846,
-0.63076923076923,-0.615384615384615,-0.6,-0.584615384615384,-0.569230769230769,
-0.553846153846154,-0.538461538461538,-0.523076923076923,-0.507692307692308,
-0.492307692307692,-0.476923076923077,-0.461538461538462,-0.446153846153846,
-0.430769230769231,-0.415384615384615,-0.4,-0.384615384615385,-0.369230769230769,
-0.353846153846154,-0.338461538461538,-0.323076923076923,-0.307692307692308,
-0.292307692307692,-0.276923076923077,-0.261538461538462,-0.246153846153846,
-0.230769230769231,-0.215384615384615,-0.2,-0.184615384615385,-0.169230769230769,
-0.153846153846154,-0.138461538461538,-0.123076923076923,-0.107692307692308,
-0.0923076923076923,-0.0769230769230769,-0.0615384615384615,-0.0461538461538462,
-0.0307692307692308,-0.0153846153846154,-0.00577184337450277),
 .UNSPECIFIED.)
CURVE()
GEOMETRIC_REPRESENTATION_ITEM()
RATIONAL_B_SPLINE_CURVE((1.,1.,1.,1.,1.,1.,1.,1.,1.,1.,1.,1.,1.,1.,1.,1.,
1.,1.,1.,1.,1.,1.,1.,1.,1.,1.,1.,1.,1.,1.,1.,1.,1.,1.,1.,1.,1.,1.,1.,1.,
1.,1.,1.,1.,1.,1.,1.,1.,1.,1.,1.,1.,1.,1.,1.,1.,1.,1.,1.,1.,1.,1.,1.,1.,
1.,1.,1.,1.,1.,1.))
REPRESENTATION_ITEM('')
);
#306=(
BOUNDED_CURVE()
B_SPLINE_CURVE(5,(#43423,#43424,#43425,#43426,#43427,#43428,#43429,#43430,
#43431,#43432,#43433,#43434,#43435,#43436,#43437,#43438,#43439,#43440,#43441,
#43442,#43443,#43444,#43445,#43446,#43447,#43448,#43449,#43450,#43451,#43452,
#43453,#43454,#43455,#43456,#43457,#43458,#43459,#43460,#43461,#43462,#43463,
#43464,#43465,#43466,#43467,#43468,#43469,#43470,#43471,#43472,#43473,#43474,
#43475,#43476,#43477,#43478,#43479,#43480,#43481,#43482,#43483,#43484,#43485,
#43486,#43487,#43488,#43489,#43490,#43491,#43492),.UNSPECIFIED.,.F.,.F.)
B_SPLINE_CURVE_WITH_KNOTS((6,1,1,1,1,1,1,1,1,1,1,1,1,1,1,1,1,1,1,1,1,1,
1,1,1,1,1,1,1,1,1,1,1,1,1,1,1,1,1,1,1,1,1,1,1,1,1,1,1,1,1,1,1,1,1,1,1,1,
1,1,1,1,1,1,1,6),(-0.994228156739689,-0.984615384615383,-0.969230769230768,
-0.953846153846152,-0.938461538461537,-0.923076923076922,-0.907692307692306,
-0.892307692307691,-0.876923076923076,-0.86153846153846,-0.846153846153845,
-0.83076923076923,-0.815384615384614,-0.799999999999999,-0.784615384615384,
-0.769230769230768,-0.753846153846153,-0.738461538461538,-0.723076923076922,
-0.707692307692307,-0.692307692307692,-0.676923076923076,-0.661538461538461,
-0.646153846153846,-0.63076923076923,-0.615384615384615,-0.6,-0.584615384615384,
-0.569230769230769,-0.553846153846154,-0.538461538461538,-0.523076923076923,
-0.507692307692308,-0.492307692307692,-0.476923076923077,-0.461538461538462,
-0.446153846153846,-0.430769230769231,-0.415384615384615,-0.4,-0.384615384615385,
-0.369230769230769,-0.353846153846154,-0.338461538461538,-0.323076923076923,
-0.307692307692308,-0.292307692307692,-0.276923076923077,-0.261538461538462,
-0.246153846153846,-0.230769230769231,-0.215384615384615,-0.2,-0.184615384615385,
-0.169230769230769,-0.153846153846154,-0.138461538461538,-0.123076923076923,
-0.107692307692308,-0.0923076923076923,-0.0769230769230769,-0.0615384615384615,
-0.0461538461538462,-0.0307692307692308,-0.0153846153846154,0.),
 .UNSPECIFIED.)
CURVE()
GEOMETRIC_REPRESENTATION_ITEM()
RATIONAL_B_SPLINE_CURVE((1.,1.,1.,1.,1.,1.,1.,1.,1.,1.,1.,1.,1.,1.,1.,1.,
1.,1.,1.,1.,1.,1.,1.,1.,1.,1.,1.,1.,1.,1.,1.,1.,1.,1.,1.,1.,1.,1.,1.,1.,
1.,1.,1.,1.,1.,1.,1.,1.,1.,1.,1.,1.,1.,1.,1.,1.,1.,1.,1.,1.,1.,1.,1.,1.,
1.,1.,1.,1.,1.,1.))
REPRESENTATION_ITEM('')
);
#307=(
BOUNDED_CURVE()
B_SPLINE_CURVE(5,(#43645,#43646,#43647,#43648,#43649,#43650,#43651,#43652,
#43653,#43654,#43655,#43656,#43657,#43658,#43659,#43660,#43661,#43662,#43663,
#43664,#43665,#43666,#43667,#43668,#43669,#43670,#43671,#43672,#43673,#43674,
#43675,#43676,#43677,#43678,#43679,#43680,#43681,#43682,#43683,#43684,#43685,
#43686,#43687,#43688,#43689,#43690,#43691,#43692,#43693,#43694,#43695,#43696,
#43697,#43698,#43699,#43700,#43701,#43702,#43703,#43704,#43705,#43706,#43707,
#43708,#43709,#43710,#43711,#43712,#43713,#43714),.UNSPECIFIED.,.F.,.F.)
B_SPLINE_CURVE_WITH_KNOTS((6,1,1,1,1,1,1,1,1,1,1,1,1,1,1,1,1,1,1,1,1,1,
1,1,1,1,1,1,1,1,1,1,1,1,1,1,1,1,1,1,1,1,1,1,1,1,1,1,1,1,1,1,1,1,1,1,1,1,
1,1,1,1,1,1,1,6),(-1.,-0.984615384615383,-0.969230769230768,-0.953846153846152,
-0.938461538461537,-0.923076923076922,-0.907692307692306,-0.892307692307691,
-0.876923076923076,-0.86153846153846,-0.846153846153845,-0.83076923076923,
-0.815384615384614,-0.799999999999999,-0.784615384615384,-0.769230769230768,
-0.753846153846153,-0.738461538461538,-0.723076923076922,-0.707692307692307,
-0.692307692307692,-0.676923076923076,-0.661538461538461,-0.646153846153846,
-0.63076923076923,-0.615384615384615,-0.6,-0.584615384615384,-0.569230769230769,
-0.553846153846154,-0.538461538461538,-0.523076923076923,-0.507692307692308,
-0.492307692307692,-0.476923076923077,-0.461538461538462,-0.446153846153846,
-0.430769230769231,-0.415384615384615,-0.4,-0.384615384615385,-0.369230769230769,
-0.353846153846154,-0.338461538461538,-0.323076923076923,-0.307692307692308,
-0.292307692307692,-0.276923076923077,-0.261538461538462,-0.246153846153846,
-0.230769230769231,-0.215384615384615,-0.2,-0.184615384615385,-0.169230769230769,
-0.153846153846154,-0.138461538461538,-0.123076923076923,-0.107692307692308,
-0.0923076923076923,-0.0769230769230769,-0.0615384615384615,-0.0461538461538462,
-0.0307692307692308,-0.0153846153846154,-0.00577184337451766),
 .UNSPECIFIED.)
CURVE()
GEOMETRIC_REPRESENTATION_ITEM()
RATIONAL_B_SPLINE_CURVE((1.,1.,1.,1.,1.,1.,1.,1.,1.,1.,1.,1.,1.,1.,1.,1.,
1.,1.,1.,1.,1.,1.,1.,1.,1.,1.,1.,1.,1.,1.,1.,1.,1.,1.,1.,1.,1.,1.,1.,1.,
1.,1.,1.,1.,1.,1.,1.,1.,1.,1.,1.,1.,1.,1.,1.,1.,1.,1.,1.,1.,1.,1.,1.,1.,
1.,1.,1.,1.,1.,1.))
REPRESENTATION_ITEM('')
);
#308=(
BOUNDED_CURVE()
B_SPLINE_CURVE(5,(#43865,#43866,#43867,#43868,#43869,#43870,#43871,#43872,
#43873,#43874,#43875,#43876,#43877,#43878,#43879,#43880,#43881,#43882,#43883,
#43884,#43885,#43886,#43887,#43888,#43889,#43890,#43891,#43892,#43893,#43894,
#43895,#43896,#43897,#43898,#43899,#43900,#43901,#43902,#43903,#43904,#43905,
#43906,#43907,#43908,#43909,#43910,#43911,#43912,#43913,#43914,#43915,#43916,
#43917,#43918,#43919,#43920,#43921,#43922,#43923,#43924,#43925,#43926,#43927,
#43928,#43929,#43930,#43931,#43932,#43933,#43934),.UNSPECIFIED.,.F.,.F.)
B_SPLINE_CURVE_WITH_KNOTS((6,1,1,1,1,1,1,1,1,1,1,1,1,1,1,1,1,1,1,1,1,1,
1,1,1,1,1,1,1,1,1,1,1,1,1,1,1,1,1,1,1,1,1,1,1,1,1,1,1,1,1,1,1,1,1,1,1,1,
1,1,1,1,1,1,1,6),(-0.994228156739687,-0.984615384615383,-0.969230769230768,
-0.953846153846152,-0.938461538461537,-0.923076923076922,-0.907692307692306,
-0.892307692307691,-0.876923076923076,-0.86153846153846,-0.846153846153845,
-0.83076923076923,-0.815384615384614,-0.799999999999999,-0.784615384615384,
-0.769230769230768,-0.753846153846153,-0.738461538461538,-0.723076923076922,
-0.707692307692307,-0.692307692307692,-0.676923076923076,-0.661538461538461,
-0.646153846153846,-0.63076923076923,-0.615384615384615,-0.6,-0.584615384615384,
-0.569230769230769,-0.553846153846154,-0.538461538461538,-0.523076923076923,
-0.507692307692308,-0.492307692307692,-0.476923076923077,-0.461538461538462,
-0.446153846153846,-0.430769230769231,-0.415384615384615,-0.4,-0.384615384615385,
-0.369230769230769,-0.353846153846154,-0.338461538461538,-0.323076923076923,
-0.307692307692308,-0.292307692307692,-0.276923076923077,-0.261538461538462,
-0.246153846153846,-0.230769230769231,-0.215384615384615,-0.2,-0.184615384615385,
-0.169230769230769,-0.153846153846154,-0.138461538461538,-0.123076923076923,
-0.107692307692308,-0.0923076923076923,-0.0769230769230769,-0.0615384615384615,
-0.0461538461538462,-0.0307692307692308,-0.0153846153846154,0.),
 .UNSPECIFIED.)
CURVE()
GEOMETRIC_REPRESENTATION_ITEM()
RATIONAL_B_SPLINE_CURVE((1.,1.,1.,1.,1.,1.,1.,1.,1.,1.,1.,1.,1.,1.,1.,1.,
1.,1.,1.,1.,1.,1.,1.,1.,1.,1.,1.,1.,1.,1.,1.,1.,1.,1.,1.,1.,1.,1.,1.,1.,
1.,1.,1.,1.,1.,1.,1.,1.,1.,1.,1.,1.,1.,1.,1.,1.,1.,1.,1.,1.,1.,1.,1.,1.,
1.,1.,1.,1.,1.,1.))
REPRESENTATION_ITEM('')
);
#309=(
BOUNDED_CURVE()
B_SPLINE_CURVE(5,(#44087,#44088,#44089,#44090,#44091,#44092,#44093,#44094,
#44095,#44096,#44097,#44098,#44099,#44100,#44101,#44102,#44103,#44104,#44105,
#44106,#44107,#44108,#44109,#44110,#44111,#44112,#44113,#44114,#44115,#44116,
#44117,#44118,#44119,#44120,#44121,#44122,#44123,#44124,#44125,#44126,#44127,
#44128,#44129,#44130,#44131,#44132,#44133,#44134,#44135,#44136,#44137,#44138,
#44139,#44140,#44141,#44142,#44143,#44144,#44145,#44146,#44147,#44148,#44149,
#44150,#44151,#44152,#44153,#44154,#44155,#44156),.UNSPECIFIED.,.F.,.F.)
B_SPLINE_CURVE_WITH_KNOTS((6,1,1,1,1,1,1,1,1,1,1,1,1,1,1,1,1,1,1,1,1,1,
1,1,1,1,1,1,1,1,1,1,1,1,1,1,1,1,1,1,1,1,1,1,1,1,1,1,1,1,1,1,1,1,1,1,1,1,
1,1,1,1,1,1,1,6),(-1.,-0.984615384615383,-0.969230769230768,-0.953846153846152,
-0.938461538461537,-0.923076923076922,-0.907692307692306,-0.892307692307691,
-0.876923076923076,-0.86153846153846,-0.846153846153845,-0.83076923076923,
-0.815384615384614,-0.799999999999999,-0.784615384615384,-0.769230769230768,
-0.753846153846153,-0.738461538461538,-0.723076923076922,-0.707692307692307,
-0.692307692307692,-0.676923076923076,-0.661538461538461,-0.646153846153846,
-0.63076923076923,-0.615384615384615,-0.6,-0.584615384615384,-0.569230769230769,
-0.553846153846154,-0.538461538461538,-0.523076923076923,-0.507692307692308,
-0.492307692307692,-0.476923076923077,-0.461538461538462,-0.446153846153846,
-0.430769230769231,-0.415384615384615,-0.4,-0.384615384615385,-0.369230769230769,
-0.353846153846154,-0.338461538461538,-0.323076923076923,-0.307692307692308,
-0.292307692307692,-0.276923076923077,-0.261538461538462,-0.246153846153846,
-0.230769230769231,-0.215384615384615,-0.2,-0.184615384615385,-0.169230769230769,
-0.153846153846154,-0.138461538461538,-0.123076923076923,-0.107692307692308,
-0.0923076923076923,-0.0769230769230769,-0.0615384615384615,-0.0461538461538462,
-0.0307692307692308,-0.0153846153846154,-0.00577184337452512),
 .UNSPECIFIED.)
CURVE()
GEOMETRIC_REPRESENTATION_ITEM()
RATIONAL_B_SPLINE_CURVE((1.,1.,1.,1.,1.,1.,1.,1.,1.,1.,1.,1.,1.,1.,1.,1.,
1.,1.,1.,1.,1.,1.,1.,1.,1.,1.,1.,1.,1.,1.,1.,1.,1.,1.,1.,1.,1.,1.,1.,1.,
1.,1.,1.,1.,1.,1.,1.,1.,1.,1.,1.,1.,1.,1.,1.,1.,1.,1.,1.,1.,1.,1.,1.,1.,
1.,1.,1.,1.,1.,1.))
REPRESENTATION_ITEM('')
);
#310=(
BOUNDED_CURVE()
B_SPLINE_CURVE(5,(#44307,#44308,#44309,#44310,#44311,#44312,#44313,#44314,
#44315,#44316,#44317,#44318,#44319,#44320,#44321,#44322,#44323,#44324,#44325,
#44326,#44327,#44328,#44329,#44330,#44331,#44332,#44333,#44334,#44335,#44336,
#44337,#44338,#44339,#44340,#44341,#44342,#44343,#44344,#44345,#44346,#44347,
#44348,#44349,#44350,#44351,#44352,#44353,#44354,#44355,#44356,#44357,#44358,
#44359,#44360,#44361,#44362,#44363,#44364,#44365,#44366,#44367,#44368,#44369,
#44370,#44371,#44372,#44373,#44374,#44375,#44376),.UNSPECIFIED.,.F.,.F.)
B_SPLINE_CURVE_WITH_KNOTS((6,1,1,1,1,1,1,1,1,1,1,1,1,1,1,1,1,1,1,1,1,1,
1,1,1,1,1,1,1,1,1,1,1,1,1,1,1,1,1,1,1,1,1,1,1,1,1,1,1,1,1,1,1,1,1,1,1,1,
1,1,1,1,1,1,1,6),(-0.994228156739691,-0.984615384615383,-0.969230769230768,
-0.953846153846152,-0.938461538461537,-0.923076923076922,-0.907692307692306,
-0.892307692307691,-0.876923076923076,-0.86153846153846,-0.846153846153845,
-0.83076923076923,-0.815384615384614,-0.799999999999999,-0.784615384615384,
-0.769230769230768,-0.753846153846153,-0.738461538461538,-0.723076923076922,
-0.707692307692307,-0.692307692307692,-0.676923076923076,-0.661538461538461,
-0.646153846153846,-0.63076923076923,-0.615384615384615,-0.6,-0.584615384615384,
-0.569230769230769,-0.553846153846154,-0.538461538461538,-0.523076923076923,
-0.507692307692308,-0.492307692307692,-0.476923076923077,-0.461538461538462,
-0.446153846153846,-0.430769230769231,-0.415384615384615,-0.4,-0.384615384615385,
-0.369230769230769,-0.353846153846154,-0.338461538461538,-0.323076923076923,
-0.307692307692308,-0.292307692307692,-0.276923076923077,-0.261538461538462,
-0.246153846153846,-0.230769230769231,-0.215384615384615,-0.2,-0.184615384615385,
-0.169230769230769,-0.153846153846154,-0.138461538461538,-0.123076923076923,
-0.107692307692308,-0.0923076923076923,-0.0769230769230769,-0.0615384615384615,
-0.0461538461538462,-0.0307692307692308,-0.0153846153846154,0.),
 .UNSPECIFIED.)
CURVE()
GEOMETRIC_REPRESENTATION_ITEM()
RATIONAL_B_SPLINE_CURVE((1.,1.,1.,1.,1.,1.,1.,1.,1.,1.,1.,1.,1.,1.,1.,1.,
1.,1.,1.,1.,1.,1.,1.,1.,1.,1.,1.,1.,1.,1.,1.,1.,1.,1.,1.,1.,1.,1.,1.,1.,
1.,1.,1.,1.,1.,1.,1.,1.,1.,1.,1.,1.,1.,1.,1.,1.,1.,1.,1.,1.,1.,1.,1.,1.,
1.,1.,1.,1.,1.,1.))
REPRESENTATION_ITEM('')
);
#311=(
BOUNDED_CURVE()
B_SPLINE_CURVE(5,(#44529,#44530,#44531,#44532,#44533,#44534,#44535,#44536,
#44537,#44538,#44539,#44540,#44541,#44542,#44543,#44544,#44545,#44546,#44547,
#44548,#44549,#44550,#44551,#44552,#44553,#44554,#44555,#44556,#44557,#44558,
#44559,#44560,#44561,#44562,#44563,#44564,#44565,#44566,#44567,#44568,#44569,
#44570,#44571,#44572,#44573,#44574,#44575,#44576,#44577,#44578,#44579,#44580,
#44581,#44582,#44583,#44584,#44585,#44586,#44587,#44588,#44589,#44590,#44591,
#44592,#44593,#44594,#44595,#44596,#44597,#44598),.UNSPECIFIED.,.F.,.F.)
B_SPLINE_CURVE_WITH_KNOTS((6,1,1,1,1,1,1,1,1,1,1,1,1,1,1,1,1,1,1,1,1,1,
1,1,1,1,1,1,1,1,1,1,1,1,1,1,1,1,1,1,1,1,1,1,1,1,1,1,1,1,1,1,1,1,1,1,1,1,
1,1,1,1,1,1,1,6),(-1.,-0.984615384615383,-0.969230769230768,-0.953846153846152,
-0.938461538461537,-0.923076923076922,-0.907692307692306,-0.892307692307691,
-0.876923076923076,-0.86153846153846,-0.846153846153845,-0.83076923076923,
-0.815384615384614,-0.799999999999999,-0.784615384615384,-0.769230769230768,
-0.753846153846153,-0.738461538461538,-0.723076923076922,-0.707692307692307,
-0.692307692307692,-0.676923076923076,-0.661538461538461,-0.646153846153846,
-0.63076923076923,-0.615384615384615,-0.6,-0.584615384615384,-0.569230769230769,
-0.553846153846154,-0.538461538461538,-0.523076923076923,-0.507692307692308,
-0.492307692307692,-0.476923076923077,-0.461538461538462,-0.446153846153846,
-0.430769230769231,-0.415384615384615,-0.4,-0.384615384615385,-0.369230769230769,
-0.353846153846154,-0.338461538461538,-0.323076923076923,-0.307692307692308,
-0.292307692307692,-0.276923076923077,-0.261538461538462,-0.246153846153846,
-0.230769230769231,-0.215384615384615,-0.2,-0.184615384615385,-0.169230769230769,
-0.153846153846154,-0.138461538461538,-0.123076923076923,-0.107692307692308,
-0.0923076923076923,-0.0769230769230769,-0.0615384615384615,-0.0461538461538462,
-0.0307692307692308,-0.0153846153846154,-0.00577184337448448),
 .UNSPECIFIED.)
CURVE()
GEOMETRIC_REPRESENTATION_ITEM()
RATIONAL_B_SPLINE_CURVE((1.,1.,1.,1.,1.,1.,1.,1.,1.,1.,1.,1.,1.,1.,1.,1.,
1.,1.,1.,1.,1.,1.,1.,1.,1.,1.,1.,1.,1.,1.,1.,1.,1.,1.,1.,1.,1.,1.,1.,1.,
1.,1.,1.,1.,1.,1.,1.,1.,1.,1.,1.,1.,1.,1.,1.,1.,1.,1.,1.,1.,1.,1.,1.,1.,
1.,1.,1.,1.,1.,1.))
REPRESENTATION_ITEM('')
);
#312=(
BOUNDED_CURVE()
B_SPLINE_CURVE(5,(#44749,#44750,#44751,#44752,#44753,#44754,#44755,#44756,
#44757,#44758,#44759,#44760,#44761,#44762,#44763,#44764,#44765,#44766,#44767,
#44768,#44769,#44770,#44771,#44772,#44773,#44774,#44775,#44776,#44777,#44778,
#44779,#44780,#44781,#44782,#44783,#44784,#44785,#44786,#44787,#44788,#44789,
#44790,#44791,#44792,#44793,#44794,#44795,#44796,#44797,#44798,#44799,#44800,
#44801,#44802,#44803,#44804,#44805,#44806,#44807,#44808,#44809,#44810,#44811,
#44812,#44813,#44814,#44815,#44816,#44817,#44818),.UNSPECIFIED.,.F.,.F.)
B_SPLINE_CURVE_WITH_KNOTS((6,1,1,1,1,1,1,1,1,1,1,1,1,1,1,1,1,1,1,1,1,1,
1,1,1,1,1,1,1,1,1,1,1,1,1,1,1,1,1,1,1,1,1,1,1,1,1,1,1,1,1,1,1,1,1,1,1,1,
1,1,1,1,1,1,1,6),(-0.99422815673972,-0.984615384615383,-0.969230769230768,
-0.953846153846152,-0.938461538461537,-0.923076923076922,-0.907692307692306,
-0.892307692307691,-0.876923076923076,-0.86153846153846,-0.846153846153845,
-0.83076923076923,-0.815384615384614,-0.799999999999999,-0.784615384615384,
-0.769230769230768,-0.753846153846153,-0.738461538461538,-0.723076923076922,
-0.707692307692307,-0.692307692307692,-0.676923076923076,-0.661538461538461,
-0.646153846153846,-0.63076923076923,-0.615384615384615,-0.6,-0.584615384615384,
-0.569230769230769,-0.553846153846154,-0.538461538461538,-0.523076923076923,
-0.507692307692308,-0.492307692307692,-0.476923076923077,-0.461538461538462,
-0.446153846153846,-0.430769230769231,-0.415384615384615,-0.4,-0.384615384615385,
-0.369230769230769,-0.353846153846154,-0.338461538461538,-0.323076923076923,
-0.307692307692308,-0.292307692307692,-0.276923076923077,-0.261538461538462,
-0.246153846153846,-0.230769230769231,-0.215384615384615,-0.2,-0.184615384615385,
-0.169230769230769,-0.153846153846154,-0.138461538461538,-0.123076923076923,
-0.107692307692308,-0.0923076923076923,-0.0769230769230769,-0.0615384615384615,
-0.0461538461538462,-0.0307692307692308,-0.0153846153846154,0.),
 .UNSPECIFIED.)
CURVE()
GEOMETRIC_REPRESENTATION_ITEM()
RATIONAL_B_SPLINE_CURVE((1.,1.,1.,1.,1.,1.,1.,1.,1.,1.,1.,1.,1.,1.,1.,1.,
1.,1.,1.,1.,1.,1.,1.,1.,1.,1.,1.,1.,1.,1.,1.,1.,1.,1.,1.,1.,1.,1.,1.,1.,
1.,1.,1.,1.,1.,1.,1.,1.,1.,1.,1.,1.,1.,1.,1.,1.,1.,1.,1.,1.,1.,1.,1.,1.,
1.,1.,1.,1.,1.,1.))
REPRESENTATION_ITEM('')
);
#313=(
BOUNDED_CURVE()
B_SPLINE_CURVE(5,(#44971,#44972,#44973,#44974,#44975,#44976,#44977,#44978,
#44979,#44980,#44981,#44982,#44983,#44984,#44985,#44986,#44987,#44988,#44989,
#44990,#44991,#44992,#44993,#44994,#44995,#44996,#44997,#44998,#44999,#45000,
#45001,#45002,#45003,#45004,#45005,#45006,#45007,#45008,#45009,#45010,#45011,
#45012,#45013,#45014,#45015,#45016,#45017,#45018,#45019,#45020,#45021,#45022,
#45023,#45024,#45025,#45026,#45027,#45028,#45029,#45030,#45031,#45032,#45033,
#45034,#45035,#45036,#45037,#45038,#45039,#45040),.UNSPECIFIED.,.F.,.F.)
B_SPLINE_CURVE_WITH_KNOTS((6,1,1,1,1,1,1,1,1,1,1,1,1,1,1,1,1,1,1,1,1,1,
1,1,1,1,1,1,1,1,1,1,1,1,1,1,1,1,1,1,1,1,1,1,1,1,1,1,1,1,1,1,1,1,1,1,1,1,
1,1,1,1,1,1,1,6),(-1.,-0.984615384615383,-0.969230769230768,-0.953846153846152,
-0.938461538461537,-0.923076923076922,-0.907692307692306,-0.892307692307691,
-0.876923076923076,-0.86153846153846,-0.846153846153845,-0.83076923076923,
-0.815384615384614,-0.799999999999999,-0.784615384615384,-0.769230769230768,
-0.753846153846153,-0.738461538461538,-0.723076923076922,-0.707692307692307,
-0.692307692307692,-0.676923076923076,-0.661538461538461,-0.646153846153846,
-0.63076923076923,-0.615384615384615,-0.6,-0.584615384615384,-0.569230769230769,
-0.553846153846154,-0.538461538461538,-0.523076923076923,-0.507692307692308,
-0.492307692307692,-0.476923076923077,-0.461538461538462,-0.446153846153846,
-0.430769230769231,-0.415384615384615,-0.4,-0.384615384615385,-0.369230769230769,
-0.353846153846154,-0.338461538461538,-0.323076923076923,-0.307692307692308,
-0.292307692307692,-0.276923076923077,-0.261538461538462,-0.246153846153846,
-0.230769230769231,-0.215384615384615,-0.2,-0.184615384615385,-0.169230769230769,
-0.153846153846154,-0.138461538461538,-0.123076923076923,-0.107692307692308,
-0.0923076923076923,-0.0769230769230769,-0.0615384615384615,-0.0461538461538462,
-0.0307692307692308,-0.0153846153846154,-0.00577184337448251),
 .UNSPECIFIED.)
CURVE()
GEOMETRIC_REPRESENTATION_ITEM()
RATIONAL_B_SPLINE_CURVE((1.,1.,1.,1.,1.,1.,1.,1.,1.,1.,1.,1.,1.,1.,1.,1.,
1.,1.,1.,1.,1.,1.,1.,1.,1.,1.,1.,1.,1.,1.,1.,1.,1.,1.,1.,1.,1.,1.,1.,1.,
1.,1.,1.,1.,1.,1.,1.,1.,1.,1.,1.,1.,1.,1.,1.,1.,1.,1.,1.,1.,1.,1.,1.,1.,
1.,1.,1.,1.,1.,1.))
REPRESENTATION_ITEM('')
);
#314=(
BOUNDED_CURVE()
B_SPLINE_CURVE(5,(#45191,#45192,#45193,#45194,#45195,#45196,#45197,#45198,
#45199,#45200,#45201,#45202,#45203,#45204,#45205,#45206,#45207,#45208,#45209,
#45210,#45211,#45212,#45213,#45214,#45215,#45216,#45217,#45218,#45219,#45220,
#45221,#45222,#45223,#45224,#45225,#45226,#45227,#45228,#45229,#45230,#45231,
#45232,#45233,#45234,#45235,#45236,#45237,#45238,#45239,#45240,#45241,#45242,
#45243,#45244,#45245,#45246,#45247,#45248,#45249,#45250,#45251,#45252,#45253,
#45254,#45255,#45256,#45257,#45258,#45259,#45260),.UNSPECIFIED.,.F.,.F.)
B_SPLINE_CURVE_WITH_KNOTS((6,1,1,1,1,1,1,1,1,1,1,1,1,1,1,1,1,1,1,1,1,1,
1,1,1,1,1,1,1,1,1,1,1,1,1,1,1,1,1,1,1,1,1,1,1,1,1,1,1,1,1,1,1,1,1,1,1,1,
1,1,1,1,1,1,1,6),(-0.994228156739703,-0.984615384615383,-0.969230769230768,
-0.953846153846152,-0.938461538461537,-0.923076923076922,-0.907692307692306,
-0.892307692307691,-0.876923076923076,-0.86153846153846,-0.846153846153845,
-0.83076923076923,-0.815384615384614,-0.799999999999999,-0.784615384615384,
-0.769230769230768,-0.753846153846153,-0.738461538461538,-0.723076923076922,
-0.707692307692307,-0.692307692307692,-0.676923076923076,-0.661538461538461,
-0.646153846153846,-0.63076923076923,-0.615384615384615,-0.6,-0.584615384615384,
-0.569230769230769,-0.553846153846154,-0.538461538461538,-0.523076923076923,
-0.507692307692308,-0.492307692307692,-0.476923076923077,-0.461538461538462,
-0.446153846153846,-0.430769230769231,-0.415384615384615,-0.4,-0.384615384615385,
-0.369230769230769,-0.353846153846154,-0.338461538461538,-0.323076923076923,
-0.307692307692308,-0.292307692307692,-0.276923076923077,-0.261538461538462,
-0.246153846153846,-0.230769230769231,-0.215384615384615,-0.2,-0.184615384615385,
-0.169230769230769,-0.153846153846154,-0.138461538461538,-0.123076923076923,
-0.107692307692308,-0.0923076923076923,-0.0769230769230769,-0.0615384615384615,
-0.0461538461538462,-0.0307692307692308,-0.0153846153846154,0.),
 .UNSPECIFIED.)
CURVE()
GEOMETRIC_REPRESENTATION_ITEM()
RATIONAL_B_SPLINE_CURVE((1.,1.,1.,1.,1.,1.,1.,1.,1.,1.,1.,1.,1.,1.,1.,1.,
1.,1.,1.,1.,1.,1.,1.,1.,1.,1.,1.,1.,1.,1.,1.,1.,1.,1.,1.,1.,1.,1.,1.,1.,
1.,1.,1.,1.,1.,1.,1.,1.,1.,1.,1.,1.,1.,1.,1.,1.,1.,1.,1.,1.,1.,1.,1.,1.,
1.,1.,1.,1.,1.,1.))
REPRESENTATION_ITEM('')
);
#315=(
BOUNDED_CURVE()
B_SPLINE_CURVE(5,(#45413,#45414,#45415,#45416,#45417,#45418,#45419,#45420,
#45421,#45422,#45423,#45424,#45425,#45426,#45427,#45428,#45429,#45430,#45431,
#45432,#45433,#45434,#45435,#45436,#45437,#45438,#45439,#45440,#45441,#45442,
#45443,#45444,#45445,#45446,#45447,#45448,#45449,#45450,#45451,#45452,#45453,
#45454,#45455,#45456,#45457,#45458,#45459,#45460,#45461,#45462,#45463,#45464,
#45465,#45466,#45467,#45468,#45469,#45470,#45471,#45472,#45473,#45474,#45475,
#45476,#45477,#45478,#45479,#45480,#45481,#45482),.UNSPECIFIED.,.F.,.F.)
B_SPLINE_CURVE_WITH_KNOTS((6,1,1,1,1,1,1,1,1,1,1,1,1,1,1,1,1,1,1,1,1,1,
1,1,1,1,1,1,1,1,1,1,1,1,1,1,1,1,1,1,1,1,1,1,1,1,1,1,1,1,1,1,1,1,1,1,1,1,
1,1,1,1,1,1,1,6),(-1.,-0.984615384615383,-0.969230769230768,-0.953846153846152,
-0.938461538461537,-0.923076923076922,-0.907692307692306,-0.892307692307691,
-0.876923076923076,-0.86153846153846,-0.846153846153845,-0.83076923076923,
-0.815384615384614,-0.799999999999999,-0.784615384615384,-0.769230769230768,
-0.753846153846153,-0.738461538461538,-0.723076923076922,-0.707692307692307,
-0.692307692307692,-0.676923076923076,-0.661538461538461,-0.646153846153846,
-0.63076923076923,-0.615384615384615,-0.6,-0.584615384615384,-0.569230769230769,
-0.553846153846154,-0.538461538461538,-0.523076923076923,-0.507692307692308,
-0.492307692307692,-0.476923076923077,-0.461538461538462,-0.446153846153846,
-0.430769230769231,-0.415384615384615,-0.4,-0.384615384615385,-0.369230769230769,
-0.353846153846154,-0.338461538461538,-0.323076923076923,-0.307692307692308,
-0.292307692307692,-0.276923076923077,-0.261538461538462,-0.246153846153846,
-0.230769230769231,-0.215384615384615,-0.2,-0.184615384615385,-0.169230769230769,
-0.153846153846154,-0.138461538461538,-0.123076923076923,-0.107692307692308,
-0.0923076923076923,-0.0769230769230769,-0.0615384615384615,-0.0461538461538462,
-0.0307692307692308,-0.0153846153846154,-0.00577184337449602),
 .UNSPECIFIED.)
CURVE()
GEOMETRIC_REPRESENTATION_ITEM()
RATIONAL_B_SPLINE_CURVE((1.,1.,1.,1.,1.,1.,1.,1.,1.,1.,1.,1.,1.,1.,1.,1.,
1.,1.,1.,1.,1.,1.,1.,1.,1.,1.,1.,1.,1.,1.,1.,1.,1.,1.,1.,1.,1.,1.,1.,1.,
1.,1.,1.,1.,1.,1.,1.,1.,1.,1.,1.,1.,1.,1.,1.,1.,1.,1.,1.,1.,1.,1.,1.,1.,
1.,1.,1.,1.,1.,1.))
REPRESENTATION_ITEM('')
);
#316=(
BOUNDED_CURVE()
B_SPLINE_CURVE(5,(#45633,#45634,#45635,#45636,#45637,#45638,#45639,#45640,
#45641,#45642,#45643,#45644,#45645,#45646,#45647,#45648,#45649,#45650,#45651,
#45652,#45653,#45654,#45655,#45656,#45657,#45658,#45659,#45660,#45661,#45662,
#45663,#45664,#45665,#45666,#45667,#45668,#45669,#45670,#45671,#45672,#45673,
#45674,#45675,#45676,#45677,#45678,#45679,#45680,#45681,#45682,#45683,#45684,
#45685,#45686,#45687,#45688,#45689,#45690,#45691,#45692,#45693,#45694,#45695,
#45696,#45697,#45698,#45699,#45700,#45701,#45702),.UNSPECIFIED.,.F.,.F.)
B_SPLINE_CURVE_WITH_KNOTS((6,1,1,1,1,1,1,1,1,1,1,1,1,1,1,1,1,1,1,1,1,1,
1,1,1,1,1,1,1,1,1,1,1,1,1,1,1,1,1,1,1,1,1,1,1,1,1,1,1,1,1,1,1,1,1,1,1,1,
1,1,1,1,1,1,1,6),(-0.994228156739695,-0.984615384615383,-0.969230769230768,
-0.953846153846152,-0.938461538461537,-0.923076923076922,-0.907692307692306,
-0.892307692307691,-0.876923076923076,-0.86153846153846,-0.846153846153845,
-0.83076923076923,-0.815384615384614,-0.799999999999999,-0.784615384615384,
-0.769230769230768,-0.753846153846153,-0.738461538461538,-0.723076923076922,
-0.707692307692307,-0.692307692307692,-0.676923076923076,-0.661538461538461,
-0.646153846153846,-0.63076923076923,-0.615384615384615,-0.6,-0.584615384615384,
-0.569230769230769,-0.553846153846154,-0.538461538461538,-0.523076923076923,
-0.507692307692308,-0.492307692307692,-0.476923076923077,-0.461538461538462,
-0.446153846153846,-0.430769230769231,-0.415384615384615,-0.4,-0.384615384615385,
-0.369230769230769,-0.353846153846154,-0.338461538461538,-0.323076923076923,
-0.307692307692308,-0.292307692307692,-0.276923076923077,-0.261538461538462,
-0.246153846153846,-0.230769230769231,-0.215384615384615,-0.2,-0.184615384615385,
-0.169230769230769,-0.153846153846154,-0.138461538461538,-0.123076923076923,
-0.107692307692308,-0.0923076923076923,-0.0769230769230769,-0.0615384615384615,
-0.0461538461538462,-0.0307692307692308,-0.0153846153846154,0.),
 .UNSPECIFIED.)
CURVE()
GEOMETRIC_REPRESENTATION_ITEM()
RATIONAL_B_SPLINE_CURVE((1.,1.,1.,1.,1.,1.,1.,1.,1.,1.,1.,1.,1.,1.,1.,1.,
1.,1.,1.,1.,1.,1.,1.,1.,1.,1.,1.,1.,1.,1.,1.,1.,1.,1.,1.,1.,1.,1.,1.,1.,
1.,1.,1.,1.,1.,1.,1.,1.,1.,1.,1.,1.,1.,1.,1.,1.,1.,1.,1.,1.,1.,1.,1.,1.,
1.,1.,1.,1.,1.,1.))
REPRESENTATION_ITEM('')
);
#317=(
BOUNDED_CURVE()
B_SPLINE_CURVE(5,(#45855,#45856,#45857,#45858,#45859,#45860,#45861,#45862,
#45863,#45864,#45865,#45866,#45867,#45868,#45869,#45870,#45871,#45872,#45873,
#45874,#45875,#45876,#45877,#45878,#45879,#45880,#45881,#45882,#45883,#45884,
#45885,#45886,#45887,#45888,#45889,#45890,#45891,#45892,#45893,#45894,#45895,
#45896,#45897,#45898,#45899,#45900,#45901,#45902,#45903,#45904,#45905,#45906,
#45907,#45908,#45909,#45910,#45911,#45912,#45913,#45914,#45915,#45916,#45917,
#45918,#45919,#45920,#45921,#45922,#45923,#45924),.UNSPECIFIED.,.F.,.F.)
B_SPLINE_CURVE_WITH_KNOTS((6,1,1,1,1,1,1,1,1,1,1,1,1,1,1,1,1,1,1,1,1,1,
1,1,1,1,1,1,1,1,1,1,1,1,1,1,1,1,1,1,1,1,1,1,1,1,1,1,1,1,1,1,1,1,1,1,1,1,
1,1,1,1,1,1,1,6),(-1.,-0.984615384615383,-0.969230769230768,-0.953846153846152,
-0.938461538461537,-0.923076923076922,-0.907692307692306,-0.892307692307691,
-0.876923076923076,-0.86153846153846,-0.846153846153845,-0.83076923076923,
-0.815384615384614,-0.799999999999999,-0.784615384615384,-0.769230769230768,
-0.753846153846153,-0.738461538461538,-0.723076923076922,-0.707692307692307,
-0.692307692307692,-0.676923076923076,-0.661538461538461,-0.646153846153846,
-0.63076923076923,-0.615384615384615,-0.6,-0.584615384615384,-0.569230769230769,
-0.553846153846154,-0.538461538461538,-0.523076923076923,-0.507692307692308,
-0.492307692307692,-0.476923076923077,-0.461538461538462,-0.446153846153846,
-0.430769230769231,-0.415384615384615,-0.4,-0.384615384615385,-0.369230769230769,
-0.353846153846154,-0.338461538461538,-0.323076923076923,-0.307692307692308,
-0.292307692307692,-0.276923076923077,-0.261538461538462,-0.246153846153846,
-0.230769230769231,-0.215384615384615,-0.2,-0.184615384615385,-0.169230769230769,
-0.153846153846154,-0.138461538461538,-0.123076923076923,-0.107692307692308,
-0.0923076923076923,-0.0769230769230769,-0.0615384615384615,-0.0461538461538462,
-0.0307692307692308,-0.0153846153846154,-0.00577184337450911),
 .UNSPECIFIED.)
CURVE()
GEOMETRIC_REPRESENTATION_ITEM()
RATIONAL_B_SPLINE_CURVE((1.,1.,1.,1.,1.,1.,1.,1.,1.,1.,1.,1.,1.,1.,1.,1.,
1.,1.,1.,1.,1.,1.,1.,1.,1.,1.,1.,1.,1.,1.,1.,1.,1.,1.,1.,1.,1.,1.,1.,1.,
1.,1.,1.,1.,1.,1.,1.,1.,1.,1.,1.,1.,1.,1.,1.,1.,1.,1.,1.,1.,1.,1.,1.,1.,
1.,1.,1.,1.,1.,1.))
REPRESENTATION_ITEM('')
);
#318=(
BOUNDED_CURVE()
B_SPLINE_CURVE(5,(#46075,#46076,#46077,#46078,#46079,#46080,#46081,#46082,
#46083,#46084,#46085,#46086,#46087,#46088,#46089,#46090,#46091,#46092,#46093,
#46094,#46095,#46096,#46097,#46098,#46099,#46100,#46101,#46102,#46103,#46104,
#46105,#46106,#46107,#46108,#46109,#46110,#46111,#46112,#46113,#46114,#46115,
#46116,#46117,#46118,#46119,#46120,#46121,#46122,#46123,#46124,#46125,#46126,
#46127,#46128,#46129,#46130,#46131,#46132,#46133,#46134,#46135,#46136,#46137,
#46138,#46139,#46140,#46141,#46142,#46143,#46144),.UNSPECIFIED.,.F.,.F.)
B_SPLINE_CURVE_WITH_KNOTS((6,1,1,1,1,1,1,1,1,1,1,1,1,1,1,1,1,1,1,1,1,1,
1,1,1,1,1,1,1,1,1,1,1,1,1,1,1,1,1,1,1,1,1,1,1,1,1,1,1,1,1,1,1,1,1,1,1,1,
1,1,1,1,1,1,1,6),(-0.994228156739712,-0.984615384615383,-0.969230769230768,
-0.953846153846152,-0.938461538461537,-0.923076923076922,-0.907692307692306,
-0.892307692307691,-0.876923076923076,-0.86153846153846,-0.846153846153845,
-0.83076923076923,-0.815384615384614,-0.799999999999999,-0.784615384615384,
-0.769230769230768,-0.753846153846153,-0.738461538461538,-0.723076923076922,
-0.707692307692307,-0.692307692307692,-0.676923076923076,-0.661538461538461,
-0.646153846153846,-0.63076923076923,-0.615384615384615,-0.6,-0.584615384615384,
-0.569230769230769,-0.553846153846154,-0.538461538461538,-0.523076923076923,
-0.507692307692308,-0.492307692307692,-0.476923076923077,-0.461538461538462,
-0.446153846153846,-0.430769230769231,-0.415384615384615,-0.4,-0.384615384615385,
-0.369230769230769,-0.353846153846154,-0.338461538461538,-0.323076923076923,
-0.307692307692308,-0.292307692307692,-0.276923076923077,-0.261538461538462,
-0.246153846153846,-0.230769230769231,-0.215384615384615,-0.2,-0.184615384615385,
-0.169230769230769,-0.153846153846154,-0.138461538461538,-0.123076923076923,
-0.107692307692308,-0.0923076923076923,-0.0769230769230769,-0.0615384615384615,
-0.0461538461538462,-0.0307692307692308,-0.0153846153846154,0.),
 .UNSPECIFIED.)
CURVE()
GEOMETRIC_REPRESENTATION_ITEM()
RATIONAL_B_SPLINE_CURVE((1.,1.,1.,1.,1.,1.,1.,1.,1.,1.,1.,1.,1.,1.,1.,1.,
1.,1.,1.,1.,1.,1.,1.,1.,1.,1.,1.,1.,1.,1.,1.,1.,1.,1.,1.,1.,1.,1.,1.,1.,
1.,1.,1.,1.,1.,1.,1.,1.,1.,1.,1.,1.,1.,1.,1.,1.,1.,1.,1.,1.,1.,1.,1.,1.,
1.,1.,1.,1.,1.,1.))
REPRESENTATION_ITEM('')
);
#319=(
BOUNDED_CURVE()
B_SPLINE_CURVE(5,(#46297,#46298,#46299,#46300,#46301,#46302,#46303,#46304,
#46305,#46306,#46307,#46308,#46309,#46310,#46311,#46312,#46313,#46314,#46315,
#46316,#46317,#46318,#46319,#46320,#46321,#46322,#46323,#46324,#46325,#46326,
#46327,#46328,#46329,#46330,#46331,#46332,#46333,#46334,#46335,#46336,#46337,
#46338,#46339,#46340,#46341,#46342,#46343,#46344,#46345,#46346,#46347,#46348,
#46349,#46350,#46351,#46352,#46353,#46354,#46355,#46356,#46357,#46358,#46359,
#46360,#46361,#46362,#46363,#46364,#46365,#46366),.UNSPECIFIED.,.F.,.F.)
B_SPLINE_CURVE_WITH_KNOTS((6,1,1,1,1,1,1,1,1,1,1,1,1,1,1,1,1,1,1,1,1,1,
1,1,1,1,1,1,1,1,1,1,1,1,1,1,1,1,1,1,1,1,1,1,1,1,1,1,1,1,1,1,1,1,1,1,1,1,
1,1,1,1,1,1,1,6),(-1.,-0.984615384615383,-0.969230769230768,-0.953846153846152,
-0.938461538461537,-0.923076923076922,-0.907692307692306,-0.892307692307691,
-0.876923076923076,-0.86153846153846,-0.846153846153845,-0.83076923076923,
-0.815384615384614,-0.799999999999999,-0.784615384615384,-0.769230769230768,
-0.753846153846153,-0.738461538461538,-0.723076923076922,-0.707692307692307,
-0.692307692307692,-0.676923076923076,-0.661538461538461,-0.646153846153846,
-0.63076923076923,-0.615384615384615,-0.6,-0.584615384615384,-0.569230769230769,
-0.553846153846154,-0.538461538461538,-0.523076923076923,-0.507692307692308,
-0.492307692307692,-0.476923076923077,-0.461538461538462,-0.446153846153846,
-0.430769230769231,-0.415384615384615,-0.4,-0.384615384615385,-0.369230769230769,
-0.353846153846154,-0.338461538461538,-0.323076923076923,-0.307692307692308,
-0.292307692307692,-0.276923076923077,-0.261538461538462,-0.246153846153846,
-0.230769230769231,-0.215384615384615,-0.2,-0.184615384615385,-0.169230769230769,
-0.153846153846154,-0.138461538461538,-0.123076923076923,-0.107692307692308,
-0.0923076923076923,-0.0769230769230769,-0.0615384615384615,-0.0461538461538462,
-0.0307692307692308,-0.0153846153846154,-0.00577184337451206),
 .UNSPECIFIED.)
CURVE()
GEOMETRIC_REPRESENTATION_ITEM()
RATIONAL_B_SPLINE_CURVE((1.,1.,1.,1.,1.,1.,1.,1.,1.,1.,1.,1.,1.,1.,1.,1.,
1.,1.,1.,1.,1.,1.,1.,1.,1.,1.,1.,1.,1.,1.,1.,1.,1.,1.,1.,1.,1.,1.,1.,1.,
1.,1.,1.,1.,1.,1.,1.,1.,1.,1.,1.,1.,1.,1.,1.,1.,1.,1.,1.,1.,1.,1.,1.,1.,
1.,1.,1.,1.,1.,1.))
REPRESENTATION_ITEM('')
);
#320=(
BOUNDED_CURVE()
B_SPLINE_CURVE(5,(#46517,#46518,#46519,#46520,#46521,#46522,#46523,#46524,
#46525,#46526,#46527,#46528,#46529,#46530,#46531,#46532,#46533,#46534,#46535,
#46536,#46537,#46538,#46539,#46540,#46541,#46542,#46543,#46544,#46545,#46546,
#46547,#46548,#46549,#46550,#46551,#46552,#46553,#46554,#46555,#46556,#46557,
#46558,#46559,#46560,#46561,#46562,#46563,#46564,#46565,#46566,#46567,#46568,
#46569,#46570,#46571,#46572,#46573,#46574,#46575,#46576,#46577,#46578,#46579,
#46580,#46581,#46582,#46583,#46584,#46585,#46586),.UNSPECIFIED.,.F.,.F.)
B_SPLINE_CURVE_WITH_KNOTS((6,1,1,1,1,1,1,1,1,1,1,1,1,1,1,1,1,1,1,1,1,1,
1,1,1,1,1,1,1,1,1,1,1,1,1,1,1,1,1,1,1,1,1,1,1,1,1,1,1,1,1,1,1,1,1,1,1,1,
1,1,1,1,1,1,1,6),(-0.994228156739717,-0.984615384615383,-0.969230769230768,
-0.953846153846152,-0.938461538461537,-0.923076923076922,-0.907692307692306,
-0.892307692307691,-0.876923076923076,-0.86153846153846,-0.846153846153845,
-0.83076923076923,-0.815384615384614,-0.799999999999999,-0.784615384615384,
-0.769230769230768,-0.753846153846153,-0.738461538461538,-0.723076923076922,
-0.707692307692307,-0.692307692307692,-0.676923076923076,-0.661538461538461,
-0.646153846153846,-0.63076923076923,-0.615384615384615,-0.6,-0.584615384615384,
-0.569230769230769,-0.553846153846154,-0.538461538461538,-0.523076923076923,
-0.507692307692308,-0.492307692307692,-0.476923076923077,-0.461538461538462,
-0.446153846153846,-0.430769230769231,-0.415384615384615,-0.4,-0.384615384615385,
-0.369230769230769,-0.353846153846154,-0.338461538461538,-0.323076923076923,
-0.307692307692308,-0.292307692307692,-0.276923076923077,-0.261538461538462,
-0.246153846153846,-0.230769230769231,-0.215384615384615,-0.2,-0.184615384615385,
-0.169230769230769,-0.153846153846154,-0.138461538461538,-0.123076923076923,
-0.107692307692308,-0.0923076923076923,-0.0769230769230769,-0.0615384615384615,
-0.0461538461538462,-0.0307692307692308,-0.0153846153846154,0.),
 .UNSPECIFIED.)
CURVE()
GEOMETRIC_REPRESENTATION_ITEM()
RATIONAL_B_SPLINE_CURVE((1.,1.,1.,1.,1.,1.,1.,1.,1.,1.,1.,1.,1.,1.,1.,1.,
1.,1.,1.,1.,1.,1.,1.,1.,1.,1.,1.,1.,1.,1.,1.,1.,1.,1.,1.,1.,1.,1.,1.,1.,
1.,1.,1.,1.,1.,1.,1.,1.,1.,1.,1.,1.,1.,1.,1.,1.,1.,1.,1.,1.,1.,1.,1.,1.,
1.,1.,1.,1.,1.,1.))
REPRESENTATION_ITEM('')
);
#321=(
BOUNDED_CURVE()
B_SPLINE_CURVE(5,(#46739,#46740,#46741,#46742,#46743,#46744,#46745,#46746,
#46747,#46748,#46749,#46750,#46751,#46752,#46753,#46754,#46755,#46756,#46757,
#46758,#46759,#46760,#46761,#46762,#46763,#46764,#46765,#46766,#46767,#46768,
#46769,#46770,#46771,#46772,#46773,#46774,#46775,#46776,#46777,#46778,#46779,
#46780,#46781,#46782,#46783,#46784,#46785,#46786,#46787,#46788,#46789,#46790,
#46791,#46792,#46793,#46794,#46795,#46796,#46797,#46798,#46799,#46800,#46801,
#46802,#46803,#46804,#46805,#46806,#46807,#46808),.UNSPECIFIED.,.F.,.F.)
B_SPLINE_CURVE_WITH_KNOTS((6,1,1,1,1,1,1,1,1,1,1,1,1,1,1,1,1,1,1,1,1,1,
1,1,1,1,1,1,1,1,1,1,1,1,1,1,1,1,1,1,1,1,1,1,1,1,1,1,1,1,1,1,1,1,1,1,1,1,
1,1,1,1,1,1,1,6),(-1.,-0.984615384615383,-0.969230769230768,-0.953846153846152,
-0.938461538461537,-0.923076923076922,-0.907692307692306,-0.892307692307691,
-0.876923076923076,-0.86153846153846,-0.846153846153845,-0.83076923076923,
-0.815384615384614,-0.799999999999999,-0.784615384615384,-0.769230769230768,
-0.753846153846153,-0.738461538461538,-0.723076923076922,-0.707692307692307,
-0.692307692307692,-0.676923076923076,-0.661538461538461,-0.646153846153846,
-0.63076923076923,-0.615384615384615,-0.6,-0.584615384615384,-0.569230769230769,
-0.553846153846154,-0.538461538461538,-0.523076923076923,-0.507692307692308,
-0.492307692307692,-0.476923076923077,-0.461538461538462,-0.446153846153846,
-0.430769230769231,-0.415384615384615,-0.4,-0.384615384615385,-0.369230769230769,
-0.353846153846154,-0.338461538461538,-0.323076923076923,-0.307692307692308,
-0.292307692307692,-0.276923076923077,-0.261538461538462,-0.246153846153846,
-0.230769230769231,-0.215384615384615,-0.2,-0.184615384615385,-0.169230769230769,
-0.153846153846154,-0.138461538461538,-0.123076923076923,-0.107692307692308,
-0.0923076923076923,-0.0769230769230769,-0.0615384615384615,-0.0461538461538462,
-0.0307692307692308,-0.0153846153846154,-0.00577184337448646),
 .UNSPECIFIED.)
CURVE()
GEOMETRIC_REPRESENTATION_ITEM()
RATIONAL_B_SPLINE_CURVE((1.,1.,1.,1.,1.,1.,1.,1.,1.,1.,1.,1.,1.,1.,1.,1.,
1.,1.,1.,1.,1.,1.,1.,1.,1.,1.,1.,1.,1.,1.,1.,1.,1.,1.,1.,1.,1.,1.,1.,1.,
1.,1.,1.,1.,1.,1.,1.,1.,1.,1.,1.,1.,1.,1.,1.,1.,1.,1.,1.,1.,1.,1.,1.,1.,
1.,1.,1.,1.,1.,1.))
REPRESENTATION_ITEM('')
);
#322=(
BOUNDED_CURVE()
B_SPLINE_CURVE(5,(#46959,#46960,#46961,#46962,#46963,#46964,#46965,#46966,
#46967,#46968,#46969,#46970,#46971,#46972,#46973,#46974,#46975,#46976,#46977,
#46978,#46979,#46980,#46981,#46982,#46983,#46984,#46985,#46986,#46987,#46988,
#46989,#46990,#46991,#46992,#46993,#46994,#46995,#46996,#46997,#46998,#46999,
#47000,#47001,#47002,#47003,#47004,#47005,#47006,#47007,#47008,#47009,#47010,
#47011,#47012,#47013,#47014,#47015,#47016,#47017,#47018,#47019,#47020,#47021,
#47022,#47023,#47024,#47025,#47026,#47027,#47028),.UNSPECIFIED.,.F.,.F.)
B_SPLINE_CURVE_WITH_KNOTS((6,1,1,1,1,1,1,1,1,1,1,1,1,1,1,1,1,1,1,1,1,1,
1,1,1,1,1,1,1,1,1,1,1,1,1,1,1,1,1,1,1,1,1,1,1,1,1,1,1,1,1,1,1,1,1,1,1,1,
1,1,1,1,1,1,1,6),(-0.994228156739708,-0.984615384615383,-0.969230769230768,
-0.953846153846152,-0.938461538461537,-0.923076923076922,-0.907692307692306,
-0.892307692307691,-0.876923076923076,-0.86153846153846,-0.846153846153845,
-0.83076923076923,-0.815384615384614,-0.799999999999999,-0.784615384615384,
-0.769230769230768,-0.753846153846153,-0.738461538461538,-0.723076923076922,
-0.707692307692307,-0.692307692307692,-0.676923076923076,-0.661538461538461,
-0.646153846153846,-0.63076923076923,-0.615384615384615,-0.6,-0.584615384615384,
-0.569230769230769,-0.553846153846154,-0.538461538461538,-0.523076923076923,
-0.507692307692308,-0.492307692307692,-0.476923076923077,-0.461538461538462,
-0.446153846153846,-0.430769230769231,-0.415384615384615,-0.4,-0.384615384615385,
-0.369230769230769,-0.353846153846154,-0.338461538461538,-0.323076923076923,
-0.307692307692308,-0.292307692307692,-0.276923076923077,-0.261538461538462,
-0.246153846153846,-0.230769230769231,-0.215384615384615,-0.2,-0.184615384615385,
-0.169230769230769,-0.153846153846154,-0.138461538461538,-0.123076923076923,
-0.107692307692308,-0.0923076923076923,-0.0769230769230769,-0.0615384615384615,
-0.0461538461538462,-0.0307692307692308,-0.0153846153846154,0.),
 .UNSPECIFIED.)
CURVE()
GEOMETRIC_REPRESENTATION_ITEM()
RATIONAL_B_SPLINE_CURVE((1.,1.,1.,1.,1.,1.,1.,1.,1.,1.,1.,1.,1.,1.,1.,1.,
1.,1.,1.,1.,1.,1.,1.,1.,1.,1.,1.,1.,1.,1.,1.,1.,1.,1.,1.,1.,1.,1.,1.,1.,
1.,1.,1.,1.,1.,1.,1.,1.,1.,1.,1.,1.,1.,1.,1.,1.,1.,1.,1.,1.,1.,1.,1.,1.,
1.,1.,1.,1.,1.,1.))
REPRESENTATION_ITEM('')
);
#323=(
BOUNDED_CURVE()
B_SPLINE_CURVE(5,(#47181,#47182,#47183,#47184,#47185,#47186,#47187,#47188,
#47189,#47190,#47191,#47192,#47193,#47194,#47195,#47196,#47197,#47198,#47199,
#47200,#47201,#47202,#47203,#47204,#47205,#47206,#47207,#47208,#47209,#47210,
#47211,#47212,#47213,#47214,#47215,#47216,#47217,#47218,#47219,#47220,#47221,
#47222,#47223,#47224,#47225,#47226,#47227,#47228,#47229,#47230,#47231,#47232,
#47233,#47234,#47235,#47236,#47237,#47238,#47239,#47240,#47241,#47242,#47243,
#47244,#47245,#47246,#47247,#47248,#47249,#47250),.UNSPECIFIED.,.F.,.F.)
B_SPLINE_CURVE_WITH_KNOTS((6,1,1,1,1,1,1,1,1,1,1,1,1,1,1,1,1,1,1,1,1,1,
1,1,1,1,1,1,1,1,1,1,1,1,1,1,1,1,1,1,1,1,1,1,1,1,1,1,1,1,1,1,1,1,1,1,1,1,
1,1,1,1,1,1,1,6),(-1.,-0.984615384615383,-0.969230769230768,-0.953846153846152,
-0.938461538461537,-0.923076923076922,-0.907692307692306,-0.892307692307691,
-0.876923076923076,-0.86153846153846,-0.846153846153845,-0.83076923076923,
-0.815384615384614,-0.799999999999999,-0.784615384615384,-0.769230769230768,
-0.753846153846153,-0.738461538461538,-0.723076923076922,-0.707692307692307,
-0.692307692307692,-0.676923076923076,-0.661538461538461,-0.646153846153846,
-0.63076923076923,-0.615384615384615,-0.6,-0.584615384615384,-0.569230769230769,
-0.553846153846154,-0.538461538461538,-0.523076923076923,-0.507692307692308,
-0.492307692307692,-0.476923076923077,-0.461538461538462,-0.446153846153846,
-0.430769230769231,-0.415384615384615,-0.4,-0.384615384615385,-0.369230769230769,
-0.353846153846154,-0.338461538461538,-0.323076923076923,-0.307692307692308,
-0.292307692307692,-0.276923076923077,-0.261538461538462,-0.246153846153846,
-0.230769230769231,-0.215384615384615,-0.2,-0.184615384615385,-0.169230769230769,
-0.153846153846154,-0.138461538461538,-0.123076923076923,-0.107692307692308,
-0.0923076923076923,-0.0769230769230769,-0.0615384615384615,-0.0461538461538462,
-0.0307692307692308,-0.0153846153846154,-0.00577184337451626),
 .UNSPECIFIED.)
CURVE()
GEOMETRIC_REPRESENTATION_ITEM()
RATIONAL_B_SPLINE_CURVE((1.,1.,1.,1.,1.,1.,1.,1.,1.,1.,1.,1.,1.,1.,1.,1.,
1.,1.,1.,1.,1.,1.,1.,1.,1.,1.,1.,1.,1.,1.,1.,1.,1.,1.,1.,1.,1.,1.,1.,1.,
1.,1.,1.,1.,1.,1.,1.,1.,1.,1.,1.,1.,1.,1.,1.,1.,1.,1.,1.,1.,1.,1.,1.,1.,
1.,1.,1.,1.,1.,1.))
REPRESENTATION_ITEM('')
);
#324=(
BOUNDED_CURVE()
B_SPLINE_CURVE(5,(#47401,#47402,#47403,#47404,#47405,#47406,#47407,#47408,
#47409,#47410,#47411,#47412,#47413,#47414,#47415,#47416,#47417,#47418,#47419,
#47420,#47421,#47422,#47423,#47424,#47425,#47426,#47427,#47428,#47429,#47430,
#47431,#47432,#47433,#47434,#47435,#47436,#47437,#47438,#47439,#47440,#47441,
#47442,#47443,#47444,#47445,#47446,#47447,#47448,#47449,#47450,#47451,#47452,
#47453,#47454,#47455,#47456,#47457,#47458,#47459,#47460,#47461,#47462,#47463,
#47464,#47465,#47466,#47467,#47468,#47469,#47470),.UNSPECIFIED.,.F.,.F.)
B_SPLINE_CURVE_WITH_KNOTS((6,1,1,1,1,1,1,1,1,1,1,1,1,1,1,1,1,1,1,1,1,1,
1,1,1,1,1,1,1,1,1,1,1,1,1,1,1,1,1,1,1,1,1,1,1,1,1,1,1,1,1,1,1,1,1,1,1,1,
1,1,1,1,1,1,1,6),(-0.994228156739708,-0.984615384615383,-0.969230769230768,
-0.953846153846152,-0.938461538461537,-0.923076923076922,-0.907692307692306,
-0.892307692307691,-0.876923076923076,-0.86153846153846,-0.846153846153845,
-0.83076923076923,-0.815384615384614,-0.799999999999999,-0.784615384615384,
-0.769230769230768,-0.753846153846153,-0.738461538461538,-0.723076923076922,
-0.707692307692307,-0.692307692307692,-0.676923076923076,-0.661538461538461,
-0.646153846153846,-0.63076923076923,-0.615384615384615,-0.6,-0.584615384615384,
-0.569230769230769,-0.553846153846154,-0.538461538461538,-0.523076923076923,
-0.507692307692308,-0.492307692307692,-0.476923076923077,-0.461538461538462,
-0.446153846153846,-0.430769230769231,-0.415384615384615,-0.4,-0.384615384615385,
-0.369230769230769,-0.353846153846154,-0.338461538461538,-0.323076923076923,
-0.307692307692308,-0.292307692307692,-0.276923076923077,-0.261538461538462,
-0.246153846153846,-0.230769230769231,-0.215384615384615,-0.2,-0.184615384615385,
-0.169230769230769,-0.153846153846154,-0.138461538461538,-0.123076923076923,
-0.107692307692308,-0.0923076923076923,-0.0769230769230769,-0.0615384615384615,
-0.0461538461538462,-0.0307692307692308,-0.0153846153846154,0.),
 .UNSPECIFIED.)
CURVE()
GEOMETRIC_REPRESENTATION_ITEM()
RATIONAL_B_SPLINE_CURVE((1.,1.,1.,1.,1.,1.,1.,1.,1.,1.,1.,1.,1.,1.,1.,1.,
1.,1.,1.,1.,1.,1.,1.,1.,1.,1.,1.,1.,1.,1.,1.,1.,1.,1.,1.,1.,1.,1.,1.,1.,
1.,1.,1.,1.,1.,1.,1.,1.,1.,1.,1.,1.,1.,1.,1.,1.,1.,1.,1.,1.,1.,1.,1.,1.,
1.,1.,1.,1.,1.,1.))
REPRESENTATION_ITEM('')
);
#325=(
BOUNDED_CURVE()
B_SPLINE_CURVE(5,(#47623,#47624,#47625,#47626,#47627,#47628,#47629,#47630,
#47631,#47632,#47633,#47634,#47635,#47636,#47637,#47638,#47639,#47640,#47641,
#47642,#47643,#47644,#47645,#47646,#47647,#47648,#47649,#47650,#47651,#47652,
#47653,#47654,#47655,#47656,#47657,#47658,#47659,#47660,#47661,#47662,#47663,
#47664,#47665,#47666,#47667,#47668,#47669,#47670,#47671,#47672,#47673,#47674,
#47675,#47676,#47677,#47678,#47679,#47680,#47681,#47682,#47683,#47684,#47685,
#47686,#47687,#47688,#47689,#47690,#47691,#47692),.UNSPECIFIED.,.F.,.F.)
B_SPLINE_CURVE_WITH_KNOTS((6,1,1,1,1,1,1,1,1,1,1,1,1,1,1,1,1,1,1,1,1,1,
1,1,1,1,1,1,1,1,1,1,1,1,1,1,1,1,1,1,1,1,1,1,1,1,1,1,1,1,1,1,1,1,1,1,1,1,
1,1,1,1,1,1,1,6),(-1.,-0.984615384615383,-0.969230769230768,-0.953846153846152,
-0.938461538461537,-0.923076923076922,-0.907692307692306,-0.892307692307691,
-0.876923076923076,-0.86153846153846,-0.846153846153845,-0.83076923076923,
-0.815384615384614,-0.799999999999999,-0.784615384615384,-0.769230769230768,
-0.753846153846153,-0.738461538461538,-0.723076923076922,-0.707692307692307,
-0.692307692307692,-0.676923076923076,-0.661538461538461,-0.646153846153846,
-0.63076923076923,-0.615384615384615,-0.6,-0.584615384615384,-0.569230769230769,
-0.553846153846154,-0.538461538461538,-0.523076923076923,-0.507692307692308,
-0.492307692307692,-0.476923076923077,-0.461538461538462,-0.446153846153846,
-0.430769230769231,-0.415384615384615,-0.4,-0.384615384615385,-0.369230769230769,
-0.353846153846154,-0.338461538461538,-0.323076923076923,-0.307692307692308,
-0.292307692307692,-0.276923076923077,-0.261538461538462,-0.246153846153846,
-0.230769230769231,-0.215384615384615,-0.2,-0.184615384615385,-0.169230769230769,
-0.153846153846154,-0.138461538461538,-0.123076923076923,-0.107692307692308,
-0.0923076923076923,-0.0769230769230769,-0.0615384615384615,-0.0461538461538462,
-0.0307692307692308,-0.0153846153846154,-0.00577184337451372),
 .UNSPECIFIED.)
CURVE()
GEOMETRIC_REPRESENTATION_ITEM()
RATIONAL_B_SPLINE_CURVE((1.,1.,1.,1.,1.,1.,1.,1.,1.,1.,1.,1.,1.,1.,1.,1.,
1.,1.,1.,1.,1.,1.,1.,1.,1.,1.,1.,1.,1.,1.,1.,1.,1.,1.,1.,1.,1.,1.,1.,1.,
1.,1.,1.,1.,1.,1.,1.,1.,1.,1.,1.,1.,1.,1.,1.,1.,1.,1.,1.,1.,1.,1.,1.,1.,
1.,1.,1.,1.,1.,1.))
REPRESENTATION_ITEM('')
);
#326=(
BOUNDED_CURVE()
B_SPLINE_CURVE(5,(#47843,#47844,#47845,#47846,#47847,#47848,#47849,#47850,
#47851,#47852,#47853,#47854,#47855,#47856,#47857,#47858,#47859,#47860,#47861,
#47862,#47863,#47864,#47865,#47866,#47867,#47868,#47869,#47870,#47871,#47872,
#47873,#47874,#47875,#47876,#47877,#47878,#47879,#47880,#47881,#47882,#47883,
#47884,#47885,#47886,#47887,#47888,#47889,#47890,#47891,#47892,#47893,#47894,
#47895,#47896,#47897,#47898,#47899,#47900,#47901,#47902,#47903,#47904,#47905,
#47906,#47907,#47908,#47909,#47910,#47911,#47912),.UNSPECIFIED.,.F.,.F.)
B_SPLINE_CURVE_WITH_KNOTS((6,1,1,1,1,1,1,1,1,1,1,1,1,1,1,1,1,1,1,1,1,1,
1,1,1,1,1,1,1,1,1,1,1,1,1,1,1,1,1,1,1,1,1,1,1,1,1,1,1,1,1,1,1,1,1,1,1,1,
1,1,1,1,1,1,1,6),(-0.994228156739703,-0.984615384615383,-0.969230769230768,
-0.953846153846152,-0.938461538461537,-0.923076923076922,-0.907692307692306,
-0.892307692307691,-0.876923076923076,-0.86153846153846,-0.846153846153845,
-0.83076923076923,-0.815384615384614,-0.799999999999999,-0.784615384615384,
-0.769230769230768,-0.753846153846153,-0.738461538461538,-0.723076923076922,
-0.707692307692307,-0.692307692307692,-0.676923076923076,-0.661538461538461,
-0.646153846153846,-0.63076923076923,-0.615384615384615,-0.6,-0.584615384615384,
-0.569230769230769,-0.553846153846154,-0.538461538461538,-0.523076923076923,
-0.507692307692308,-0.492307692307692,-0.476923076923077,-0.461538461538462,
-0.446153846153846,-0.430769230769231,-0.415384615384615,-0.4,-0.384615384615385,
-0.369230769230769,-0.353846153846154,-0.338461538461538,-0.323076923076923,
-0.307692307692308,-0.292307692307692,-0.276923076923077,-0.261538461538462,
-0.246153846153846,-0.230769230769231,-0.215384615384615,-0.2,-0.184615384615385,
-0.169230769230769,-0.153846153846154,-0.138461538461538,-0.123076923076923,
-0.107692307692308,-0.0923076923076923,-0.0769230769230769,-0.0615384615384615,
-0.0461538461538462,-0.0307692307692308,-0.0153846153846154,0.),
 .UNSPECIFIED.)
CURVE()
GEOMETRIC_REPRESENTATION_ITEM()
RATIONAL_B_SPLINE_CURVE((1.,1.,1.,1.,1.,1.,1.,1.,1.,1.,1.,1.,1.,1.,1.,1.,
1.,1.,1.,1.,1.,1.,1.,1.,1.,1.,1.,1.,1.,1.,1.,1.,1.,1.,1.,1.,1.,1.,1.,1.,
1.,1.,1.,1.,1.,1.,1.,1.,1.,1.,1.,1.,1.,1.,1.,1.,1.,1.,1.,1.,1.,1.,1.,1.,
1.,1.,1.,1.,1.,1.))
REPRESENTATION_ITEM('')
);
#327=(
BOUNDED_CURVE()
B_SPLINE_CURVE(5,(#48065,#48066,#48067,#48068,#48069,#48070,#48071,#48072,
#48073,#48074,#48075,#48076,#48077,#48078,#48079,#48080,#48081,#48082,#48083,
#48084,#48085,#48086,#48087,#48088,#48089,#48090,#48091,#48092,#48093,#48094,
#48095,#48096,#48097,#48098,#48099,#48100,#48101,#48102,#48103,#48104,#48105,
#48106,#48107,#48108,#48109,#48110,#48111,#48112,#48113,#48114,#48115,#48116,
#48117,#48118,#48119,#48120,#48121,#48122,#48123,#48124,#48125,#48126,#48127,
#48128,#48129,#48130,#48131,#48132,#48133,#48134),.UNSPECIFIED.,.F.,.F.)
B_SPLINE_CURVE_WITH_KNOTS((6,1,1,1,1,1,1,1,1,1,1,1,1,1,1,1,1,1,1,1,1,1,
1,1,1,1,1,1,1,1,1,1,1,1,1,1,1,1,1,1,1,1,1,1,1,1,1,1,1,1,1,1,1,1,1,1,1,1,
1,1,1,1,1,1,1,6),(-1.,-0.984615384615383,-0.969230769230768,-0.953846153846152,
-0.938461538461537,-0.923076923076922,-0.907692307692306,-0.892307692307691,
-0.876923076923076,-0.86153846153846,-0.846153846153845,-0.83076923076923,
-0.815384615384614,-0.799999999999999,-0.784615384615384,-0.769230769230768,
-0.753846153846153,-0.738461538461538,-0.723076923076922,-0.707692307692307,
-0.692307692307692,-0.676923076923076,-0.661538461538461,-0.646153846153846,
-0.63076923076923,-0.615384615384615,-0.6,-0.584615384615384,-0.569230769230769,
-0.553846153846154,-0.538461538461538,-0.523076923076923,-0.507692307692308,
-0.492307692307692,-0.476923076923077,-0.461538461538462,-0.446153846153846,
-0.430769230769231,-0.415384615384615,-0.4,-0.384615384615385,-0.369230769230769,
-0.353846153846154,-0.338461538461538,-0.323076923076923,-0.307692307692308,
-0.292307692307692,-0.276923076923077,-0.261538461538462,-0.246153846153846,
-0.230769230769231,-0.215384615384615,-0.2,-0.184615384615385,-0.169230769230769,
-0.153846153846154,-0.138461538461538,-0.123076923076923,-0.107692307692308,
-0.0923076923076923,-0.0769230769230769,-0.0615384615384615,-0.0461538461538462,
-0.0307692307692308,-0.0153846153846154,-0.00577184337451698),
 .UNSPECIFIED.)
CURVE()
GEOMETRIC_REPRESENTATION_ITEM()
RATIONAL_B_SPLINE_CURVE((1.,1.,1.,1.,1.,1.,1.,1.,1.,1.,1.,1.,1.,1.,1.,1.,
1.,1.,1.,1.,1.,1.,1.,1.,1.,1.,1.,1.,1.,1.,1.,1.,1.,1.,1.,1.,1.,1.,1.,1.,
1.,1.,1.,1.,1.,1.,1.,1.,1.,1.,1.,1.,1.,1.,1.,1.,1.,1.,1.,1.,1.,1.,1.,1.,
1.,1.,1.,1.,1.,1.))
REPRESENTATION_ITEM('')
);
#328=(
BOUNDED_CURVE()
B_SPLINE_CURVE(5,(#48285,#48286,#48287,#48288,#48289,#48290,#48291,#48292,
#48293,#48294,#48295,#48296,#48297,#48298,#48299,#48300,#48301,#48302,#48303,
#48304,#48305,#48306,#48307,#48308,#48309,#48310,#48311,#48312,#48313,#48314,
#48315,#48316,#48317,#48318,#48319,#48320,#48321,#48322,#48323,#48324,#48325,
#48326,#48327,#48328,#48329,#48330,#48331,#48332,#48333,#48334,#48335,#48336,
#48337,#48338,#48339,#48340,#48341,#48342,#48343,#48344,#48345,#48346,#48347,
#48348,#48349,#48350,#48351,#48352,#48353,#48354),.UNSPECIFIED.,.F.,.F.)
B_SPLINE_CURVE_WITH_KNOTS((6,1,1,1,1,1,1,1,1,1,1,1,1,1,1,1,1,1,1,1,1,1,
1,1,1,1,1,1,1,1,1,1,1,1,1,1,1,1,1,1,1,1,1,1,1,1,1,1,1,1,1,1,1,1,1,1,1,1,
1,1,1,1,1,1,1,6),(-0.994228156739706,-0.984615384615383,-0.969230769230768,
-0.953846153846152,-0.938461538461537,-0.923076923076922,-0.907692307692306,
-0.892307692307691,-0.876923076923076,-0.86153846153846,-0.846153846153845,
-0.83076923076923,-0.815384615384614,-0.799999999999999,-0.784615384615384,
-0.769230769230768,-0.753846153846153,-0.738461538461538,-0.723076923076922,
-0.707692307692307,-0.692307692307692,-0.676923076923076,-0.661538461538461,
-0.646153846153846,-0.63076923076923,-0.615384615384615,-0.6,-0.584615384615384,
-0.569230769230769,-0.553846153846154,-0.538461538461538,-0.523076923076923,
-0.507692307692308,-0.492307692307692,-0.476923076923077,-0.461538461538462,
-0.446153846153846,-0.430769230769231,-0.415384615384615,-0.4,-0.384615384615385,
-0.369230769230769,-0.353846153846154,-0.338461538461538,-0.323076923076923,
-0.307692307692308,-0.292307692307692,-0.276923076923077,-0.261538461538462,
-0.246153846153846,-0.230769230769231,-0.215384615384615,-0.2,-0.184615384615385,
-0.169230769230769,-0.153846153846154,-0.138461538461538,-0.123076923076923,
-0.107692307692308,-0.0923076923076923,-0.0769230769230769,-0.0615384615384615,
-0.0461538461538462,-0.0307692307692308,-0.0153846153846154,0.),
 .UNSPECIFIED.)
CURVE()
GEOMETRIC_REPRESENTATION_ITEM()
RATIONAL_B_SPLINE_CURVE((1.,1.,1.,1.,1.,1.,1.,1.,1.,1.,1.,1.,1.,1.,1.,1.,
1.,1.,1.,1.,1.,1.,1.,1.,1.,1.,1.,1.,1.,1.,1.,1.,1.,1.,1.,1.,1.,1.,1.,1.,
1.,1.,1.,1.,1.,1.,1.,1.,1.,1.,1.,1.,1.,1.,1.,1.,1.,1.,1.,1.,1.,1.,1.,1.,
1.,1.,1.,1.,1.,1.))
REPRESENTATION_ITEM('')
);
#329=(
BOUNDED_CURVE()
B_SPLINE_CURVE(5,(#48507,#48508,#48509,#48510,#48511,#48512,#48513,#48514,
#48515,#48516,#48517,#48518,#48519,#48520,#48521,#48522,#48523,#48524,#48525,
#48526,#48527,#48528,#48529,#48530,#48531,#48532,#48533,#48534,#48535,#48536,
#48537,#48538,#48539,#48540,#48541,#48542,#48543,#48544,#48545,#48546,#48547,
#48548,#48549,#48550,#48551,#48552,#48553,#48554,#48555,#48556,#48557,#48558,
#48559,#48560,#48561,#48562,#48563,#48564,#48565,#48566,#48567,#48568,#48569,
#48570,#48571,#48572,#48573,#48574,#48575,#48576),.UNSPECIFIED.,.F.,.F.)
B_SPLINE_CURVE_WITH_KNOTS((6,1,1,1,1,1,1,1,1,1,1,1,1,1,1,1,1,1,1,1,1,1,
1,1,1,1,1,1,1,1,1,1,1,1,1,1,1,1,1,1,1,1,1,1,1,1,1,1,1,1,1,1,1,1,1,1,1,1,
1,1,1,1,1,1,1,6),(-1.,-0.984615384615383,-0.969230769230768,-0.953846153846152,
-0.938461538461537,-0.923076923076922,-0.907692307692306,-0.892307692307691,
-0.876923076923076,-0.86153846153846,-0.846153846153845,-0.83076923076923,
-0.815384615384614,-0.799999999999999,-0.784615384615384,-0.769230769230768,
-0.753846153846153,-0.738461538461538,-0.723076923076922,-0.707692307692307,
-0.692307692307692,-0.676923076923076,-0.661538461538461,-0.646153846153846,
-0.63076923076923,-0.615384615384615,-0.6,-0.584615384615384,-0.569230769230769,
-0.553846153846154,-0.538461538461538,-0.523076923076923,-0.507692307692308,
-0.492307692307692,-0.476923076923077,-0.461538461538462,-0.446153846153846,
-0.430769230769231,-0.415384615384615,-0.4,-0.384615384615385,-0.369230769230769,
-0.353846153846154,-0.338461538461538,-0.323076923076923,-0.307692307692308,
-0.292307692307692,-0.276923076923077,-0.261538461538462,-0.246153846153846,
-0.230769230769231,-0.215384615384615,-0.2,-0.184615384615385,-0.169230769230769,
-0.153846153846154,-0.138461538461538,-0.123076923076923,-0.107692307692308,
-0.0923076923076923,-0.0769230769230769,-0.0615384615384615,-0.0461538461538462,
-0.0307692307692308,-0.0153846153846154,-0.00577184337452512),
 .UNSPECIFIED.)
CURVE()
GEOMETRIC_REPRESENTATION_ITEM()
RATIONAL_B_SPLINE_CURVE((1.,1.,1.,1.,1.,1.,1.,1.,1.,1.,1.,1.,1.,1.,1.,1.,
1.,1.,1.,1.,1.,1.,1.,1.,1.,1.,1.,1.,1.,1.,1.,1.,1.,1.,1.,1.,1.,1.,1.,1.,
1.,1.,1.,1.,1.,1.,1.,1.,1.,1.,1.,1.,1.,1.,1.,1.,1.,1.,1.,1.,1.,1.,1.,1.,
1.,1.,1.,1.,1.,1.))
REPRESENTATION_ITEM('')
);
#330=(
BOUNDED_CURVE()
B_SPLINE_CURVE(5,(#48727,#48728,#48729,#48730,#48731,#48732,#48733,#48734,
#48735,#48736,#48737,#48738,#48739,#48740,#48741,#48742,#48743,#48744,#48745,
#48746,#48747,#48748,#48749,#48750,#48751,#48752,#48753,#48754,#48755,#48756,
#48757,#48758,#48759,#48760,#48761,#48762,#48763,#48764,#48765,#48766,#48767,
#48768,#48769,#48770,#48771,#48772,#48773,#48774,#48775,#48776,#48777,#48778,
#48779,#48780,#48781,#48782,#48783,#48784,#48785,#48786,#48787,#48788,#48789,
#48790,#48791,#48792,#48793,#48794,#48795,#48796),.UNSPECIFIED.,.F.,.F.)
B_SPLINE_CURVE_WITH_KNOTS((6,1,1,1,1,1,1,1,1,1,1,1,1,1,1,1,1,1,1,1,1,1,
1,1,1,1,1,1,1,1,1,1,1,1,1,1,1,1,1,1,1,1,1,1,1,1,1,1,1,1,1,1,1,1,1,1,1,1,
1,1,1,1,1,1,1,6),(-0.994228156739713,-0.984615384615383,-0.969230769230768,
-0.953846153846152,-0.938461538461537,-0.923076923076922,-0.907692307692306,
-0.892307692307691,-0.876923076923076,-0.86153846153846,-0.846153846153845,
-0.83076923076923,-0.815384615384614,-0.799999999999999,-0.784615384615384,
-0.769230769230768,-0.753846153846153,-0.738461538461538,-0.723076923076922,
-0.707692307692307,-0.692307692307692,-0.676923076923076,-0.661538461538461,
-0.646153846153846,-0.63076923076923,-0.615384615384615,-0.6,-0.584615384615384,
-0.569230769230769,-0.553846153846154,-0.538461538461538,-0.523076923076923,
-0.507692307692308,-0.492307692307692,-0.476923076923077,-0.461538461538462,
-0.446153846153846,-0.430769230769231,-0.415384615384615,-0.4,-0.384615384615385,
-0.369230769230769,-0.353846153846154,-0.338461538461538,-0.323076923076923,
-0.307692307692308,-0.292307692307692,-0.276923076923077,-0.261538461538462,
-0.246153846153846,-0.230769230769231,-0.215384615384615,-0.2,-0.184615384615385,
-0.169230769230769,-0.153846153846154,-0.138461538461538,-0.123076923076923,
-0.107692307692308,-0.0923076923076923,-0.0769230769230769,-0.0615384615384615,
-0.0461538461538462,-0.0307692307692308,-0.0153846153846154,0.),
 .UNSPECIFIED.)
CURVE()
GEOMETRIC_REPRESENTATION_ITEM()
RATIONAL_B_SPLINE_CURVE((1.,1.,1.,1.,1.,1.,1.,1.,1.,1.,1.,1.,1.,1.,1.,1.,
1.,1.,1.,1.,1.,1.,1.,1.,1.,1.,1.,1.,1.,1.,1.,1.,1.,1.,1.,1.,1.,1.,1.,1.,
1.,1.,1.,1.,1.,1.,1.,1.,1.,1.,1.,1.,1.,1.,1.,1.,1.,1.,1.,1.,1.,1.,1.,1.,
1.,1.,1.,1.,1.,1.))
REPRESENTATION_ITEM('')
);
#331=(
BOUNDED_CURVE()
B_SPLINE_CURVE(5,(#48949,#48950,#48951,#48952,#48953,#48954,#48955,#48956,
#48957,#48958,#48959,#48960,#48961,#48962,#48963,#48964,#48965,#48966,#48967,
#48968,#48969,#48970,#48971,#48972,#48973,#48974,#48975,#48976,#48977,#48978,
#48979,#48980,#48981,#48982,#48983,#48984,#48985,#48986,#48987,#48988,#48989,
#48990,#48991,#48992,#48993,#48994,#48995,#48996,#48997,#48998,#48999,#49000,
#49001,#49002,#49003,#49004,#49005,#49006,#49007,#49008,#49009,#49010,#49011,
#49012,#49013,#49014,#49015,#49016,#49017,#49018),.UNSPECIFIED.,.F.,.F.)
B_SPLINE_CURVE_WITH_KNOTS((6,1,1,1,1,1,1,1,1,1,1,1,1,1,1,1,1,1,1,1,1,1,
1,1,1,1,1,1,1,1,1,1,1,1,1,1,1,1,1,1,1,1,1,1,1,1,1,1,1,1,1,1,1,1,1,1,1,1,
1,1,1,1,1,1,1,6),(-1.,-0.984615384615383,-0.969230769230768,-0.953846153846152,
-0.938461538461537,-0.923076923076922,-0.907692307692306,-0.892307692307691,
-0.876923076923076,-0.86153846153846,-0.846153846153845,-0.83076923076923,
-0.815384615384614,-0.799999999999999,-0.784615384615384,-0.769230769230768,
-0.753846153846153,-0.738461538461538,-0.723076923076922,-0.707692307692307,
-0.692307692307692,-0.676923076923076,-0.661538461538461,-0.646153846153846,
-0.63076923076923,-0.615384615384615,-0.6,-0.584615384615384,-0.569230769230769,
-0.553846153846154,-0.538461538461538,-0.523076923076923,-0.507692307692308,
-0.492307692307692,-0.476923076923077,-0.461538461538462,-0.446153846153846,
-0.430769230769231,-0.415384615384615,-0.4,-0.384615384615385,-0.369230769230769,
-0.353846153846154,-0.338461538461538,-0.323076923076923,-0.307692307692308,
-0.292307692307692,-0.276923076923077,-0.261538461538462,-0.246153846153846,
-0.230769230769231,-0.215384615384615,-0.2,-0.184615384615385,-0.169230769230769,
-0.153846153846154,-0.138461538461538,-0.123076923076923,-0.107692307692308,
-0.0923076923076923,-0.0769230769230769,-0.0615384615384615,-0.0461538461538462,
-0.0307692307692308,-0.0153846153846154,-0.00577184337450204),
 .UNSPECIFIED.)
CURVE()
GEOMETRIC_REPRESENTATION_ITEM()
RATIONAL_B_SPLINE_CURVE((1.,1.,1.,1.,1.,1.,1.,1.,1.,1.,1.,1.,1.,1.,1.,1.,
1.,1.,1.,1.,1.,1.,1.,1.,1.,1.,1.,1.,1.,1.,1.,1.,1.,1.,1.,1.,1.,1.,1.,1.,
1.,1.,1.,1.,1.,1.,1.,1.,1.,1.,1.,1.,1.,1.,1.,1.,1.,1.,1.,1.,1.,1.,1.,1.,
1.,1.,1.,1.,1.,1.))
REPRESENTATION_ITEM('')
);
#332=(
BOUNDED_CURVE()
B_SPLINE_CURVE(5,(#49169,#49170,#49171,#49172,#49173,#49174,#49175,#49176,
#49177,#49178,#49179,#49180,#49181,#49182,#49183,#49184,#49185,#49186,#49187,
#49188,#49189,#49190,#49191,#49192,#49193,#49194,#49195,#49196,#49197,#49198,
#49199,#49200,#49201,#49202,#49203,#49204,#49205,#49206,#49207,#49208,#49209,
#49210,#49211,#49212,#49213,#49214,#49215,#49216,#49217,#49218,#49219,#49220,
#49221,#49222,#49223,#49224,#49225,#49226,#49227,#49228,#49229,#49230,#49231,
#49232,#49233,#49234,#49235,#49236,#49237,#49238),.UNSPECIFIED.,.F.,.F.)
B_SPLINE_CURVE_WITH_KNOTS((6,1,1,1,1,1,1,1,1,1,1,1,1,1,1,1,1,1,1,1,1,1,
1,1,1,1,1,1,1,1,1,1,1,1,1,1,1,1,1,1,1,1,1,1,1,1,1,1,1,1,1,1,1,1,1,1,1,1,
1,1,1,1,1,1,1,6),(-0.99422815673972,-0.984615384615383,-0.969230769230768,
-0.953846153846152,-0.938461538461537,-0.923076923076922,-0.907692307692306,
-0.892307692307691,-0.876923076923076,-0.86153846153846,-0.846153846153845,
-0.83076923076923,-0.815384615384614,-0.799999999999999,-0.784615384615384,
-0.769230769230768,-0.753846153846153,-0.738461538461538,-0.723076923076922,
-0.707692307692307,-0.692307692307692,-0.676923076923076,-0.661538461538461,
-0.646153846153846,-0.63076923076923,-0.615384615384615,-0.6,-0.584615384615384,
-0.569230769230769,-0.553846153846154,-0.538461538461538,-0.523076923076923,
-0.507692307692308,-0.492307692307692,-0.476923076923077,-0.461538461538462,
-0.446153846153846,-0.430769230769231,-0.415384615384615,-0.4,-0.384615384615385,
-0.369230769230769,-0.353846153846154,-0.338461538461538,-0.323076923076923,
-0.307692307692308,-0.292307692307692,-0.276923076923077,-0.261538461538462,
-0.246153846153846,-0.230769230769231,-0.215384615384615,-0.2,-0.184615384615385,
-0.169230769230769,-0.153846153846154,-0.138461538461538,-0.123076923076923,
-0.107692307692308,-0.0923076923076923,-0.0769230769230769,-0.0615384615384615,
-0.0461538461538462,-0.0307692307692308,-0.0153846153846154,0.),
 .UNSPECIFIED.)
CURVE()
GEOMETRIC_REPRESENTATION_ITEM()
RATIONAL_B_SPLINE_CURVE((1.,1.,1.,1.,1.,1.,1.,1.,1.,1.,1.,1.,1.,1.,1.,1.,
1.,1.,1.,1.,1.,1.,1.,1.,1.,1.,1.,1.,1.,1.,1.,1.,1.,1.,1.,1.,1.,1.,1.,1.,
1.,1.,1.,1.,1.,1.,1.,1.,1.,1.,1.,1.,1.,1.,1.,1.,1.,1.,1.,1.,1.,1.,1.,1.,
1.,1.,1.,1.,1.,1.))
REPRESENTATION_ITEM('')
);
#333=(
BOUNDED_CURVE()
B_SPLINE_CURVE(5,(#49391,#49392,#49393,#49394,#49395,#49396,#49397,#49398,
#49399,#49400,#49401,#49402,#49403,#49404,#49405,#49406,#49407,#49408,#49409,
#49410,#49411,#49412,#49413,#49414,#49415,#49416,#49417,#49418,#49419,#49420,
#49421,#49422,#49423,#49424,#49425,#49426,#49427,#49428,#49429,#49430,#49431,
#49432,#49433,#49434,#49435,#49436,#49437,#49438,#49439,#49440,#49441,#49442,
#49443,#49444,#49445,#49446,#49447,#49448,#49449,#49450,#49451,#49452,#49453,
#49454,#49455,#49456,#49457,#49458,#49459,#49460),.UNSPECIFIED.,.F.,.F.)
B_SPLINE_CURVE_WITH_KNOTS((6,1,1,1,1,1,1,1,1,1,1,1,1,1,1,1,1,1,1,1,1,1,
1,1,1,1,1,1,1,1,1,1,1,1,1,1,1,1,1,1,1,1,1,1,1,1,1,1,1,1,1,1,1,1,1,1,1,1,
1,1,1,1,1,1,1,6),(-1.,-0.984615384615383,-0.969230769230768,-0.953846153846152,
-0.938461538461537,-0.923076923076922,-0.907692307692306,-0.892307692307691,
-0.876923076923076,-0.86153846153846,-0.846153846153845,-0.83076923076923,
-0.815384615384614,-0.799999999999999,-0.784615384615384,-0.769230769230768,
-0.753846153846153,-0.738461538461538,-0.723076923076922,-0.707692307692307,
-0.692307692307692,-0.676923076923076,-0.661538461538461,-0.646153846153846,
-0.63076923076923,-0.615384615384615,-0.6,-0.584615384615384,-0.569230769230769,
-0.553846153846154,-0.538461538461538,-0.523076923076923,-0.507692307692308,
-0.492307692307692,-0.476923076923077,-0.461538461538462,-0.446153846153846,
-0.430769230769231,-0.415384615384615,-0.4,-0.384615384615385,-0.369230769230769,
-0.353846153846154,-0.338461538461538,-0.323076923076923,-0.307692307692308,
-0.292307692307692,-0.276923076923077,-0.261538461538462,-0.246153846153846,
-0.230769230769231,-0.215384615384615,-0.2,-0.184615384615385,-0.169230769230769,
-0.153846153846154,-0.138461538461538,-0.123076923076923,-0.107692307692308,
-0.0923076923076923,-0.0769230769230769,-0.0615384615384615,-0.0461538461538462,
-0.0307692307692308,-0.0153846153846154,-0.0057718433745107),
 .UNSPECIFIED.)
CURVE()
GEOMETRIC_REPRESENTATION_ITEM()
RATIONAL_B_SPLINE_CURVE((1.,1.,1.,1.,1.,1.,1.,1.,1.,1.,1.,1.,1.,1.,1.,1.,
1.,1.,1.,1.,1.,1.,1.,1.,1.,1.,1.,1.,1.,1.,1.,1.,1.,1.,1.,1.,1.,1.,1.,1.,
1.,1.,1.,1.,1.,1.,1.,1.,1.,1.,1.,1.,1.,1.,1.,1.,1.,1.,1.,1.,1.,1.,1.,1.,
1.,1.,1.,1.,1.,1.))
REPRESENTATION_ITEM('')
);
#334=(
BOUNDED_CURVE()
B_SPLINE_CURVE(5,(#49611,#49612,#49613,#49614,#49615,#49616,#49617,#49618,
#49619,#49620,#49621,#49622,#49623,#49624,#49625,#49626,#49627,#49628,#49629,
#49630,#49631,#49632,#49633,#49634,#49635,#49636,#49637,#49638,#49639,#49640,
#49641,#49642,#49643,#49644,#49645,#49646,#49647,#49648,#49649,#49650,#49651,
#49652,#49653,#49654,#49655,#49656,#49657,#49658,#49659,#49660,#49661,#49662,
#49663,#49664,#49665,#49666,#49667,#49668,#49669,#49670,#49671,#49672,#49673,
#49674,#49675,#49676,#49677,#49678,#49679,#49680),.UNSPECIFIED.,.F.,.F.)
B_SPLINE_CURVE_WITH_KNOTS((6,1,1,1,1,1,1,1,1,1,1,1,1,1,1,1,1,1,1,1,1,1,
1,1,1,1,1,1,1,1,1,1,1,1,1,1,1,1,1,1,1,1,1,1,1,1,1,1,1,1,1,1,1,1,1,1,1,1,
1,1,1,1,1,1,1,6),(-0.994228156739708,-0.984615384615383,-0.969230769230768,
-0.953846153846152,-0.938461538461537,-0.923076923076922,-0.907692307692306,
-0.892307692307691,-0.876923076923076,-0.86153846153846,-0.846153846153845,
-0.83076923076923,-0.815384615384614,-0.799999999999999,-0.784615384615384,
-0.769230769230768,-0.753846153846153,-0.738461538461538,-0.723076923076922,
-0.707692307692307,-0.692307692307692,-0.676923076923076,-0.661538461538461,
-0.646153846153846,-0.63076923076923,-0.615384615384615,-0.6,-0.584615384615384,
-0.569230769230769,-0.553846153846154,-0.538461538461538,-0.523076923076923,
-0.507692307692308,-0.492307692307692,-0.476923076923077,-0.461538461538462,
-0.446153846153846,-0.430769230769231,-0.415384615384615,-0.4,-0.384615384615385,
-0.369230769230769,-0.353846153846154,-0.338461538461538,-0.323076923076923,
-0.307692307692308,-0.292307692307692,-0.276923076923077,-0.261538461538462,
-0.246153846153846,-0.230769230769231,-0.215384615384615,-0.2,-0.184615384615385,
-0.169230769230769,-0.153846153846154,-0.138461538461538,-0.123076923076923,
-0.107692307692308,-0.0923076923076923,-0.0769230769230769,-0.0615384615384615,
-0.0461538461538462,-0.0307692307692308,-0.0153846153846154,0.),
 .UNSPECIFIED.)
CURVE()
GEOMETRIC_REPRESENTATION_ITEM()
RATIONAL_B_SPLINE_CURVE((1.,1.,1.,1.,1.,1.,1.,1.,1.,1.,1.,1.,1.,1.,1.,1.,
1.,1.,1.,1.,1.,1.,1.,1.,1.,1.,1.,1.,1.,1.,1.,1.,1.,1.,1.,1.,1.,1.,1.,1.,
1.,1.,1.,1.,1.,1.,1.,1.,1.,1.,1.,1.,1.,1.,1.,1.,1.,1.,1.,1.,1.,1.,1.,1.,
1.,1.,1.,1.,1.,1.))
REPRESENTATION_ITEM('')
);
#335=(
BOUNDED_CURVE()
B_SPLINE_CURVE(5,(#49833,#49834,#49835,#49836,#49837,#49838,#49839,#49840,
#49841,#49842,#49843,#49844,#49845,#49846,#49847,#49848,#49849,#49850,#49851,
#49852,#49853,#49854,#49855,#49856,#49857,#49858,#49859,#49860,#49861,#49862,
#49863,#49864,#49865,#49866,#49867,#49868,#49869,#49870,#49871,#49872,#49873,
#49874,#49875,#49876,#49877,#49878,#49879,#49880,#49881,#49882,#49883,#49884,
#49885,#49886,#49887,#49888,#49889,#49890,#49891,#49892,#49893,#49894,#49895,
#49896,#49897,#49898,#49899,#49900,#49901,#49902),.UNSPECIFIED.,.F.,.F.)
B_SPLINE_CURVE_WITH_KNOTS((6,1,1,1,1,1,1,1,1,1,1,1,1,1,1,1,1,1,1,1,1,1,
1,1,1,1,1,1,1,1,1,1,1,1,1,1,1,1,1,1,1,1,1,1,1,1,1,1,1,1,1,1,1,1,1,1,1,1,
1,1,1,1,1,1,1,6),(-1.,-0.984615384615383,-0.969230769230768,-0.953846153846152,
-0.938461538461537,-0.923076923076922,-0.907692307692306,-0.892307692307691,
-0.876923076923076,-0.86153846153846,-0.846153846153845,-0.83076923076923,
-0.815384615384614,-0.799999999999999,-0.784615384615384,-0.769230769230768,
-0.753846153846153,-0.738461538461538,-0.723076923076922,-0.707692307692307,
-0.692307692307692,-0.676923076923076,-0.661538461538461,-0.646153846153846,
-0.63076923076923,-0.615384615384615,-0.6,-0.584615384615384,-0.569230769230769,
-0.553846153846154,-0.538461538461538,-0.523076923076923,-0.507692307692308,
-0.492307692307692,-0.476923076923077,-0.461538461538462,-0.446153846153846,
-0.430769230769231,-0.415384615384615,-0.4,-0.384615384615385,-0.369230769230769,
-0.353846153846154,-0.338461538461538,-0.323076923076923,-0.307692307692308,
-0.292307692307692,-0.276923076923077,-0.261538461538462,-0.246153846153846,
-0.230769230769231,-0.215384615384615,-0.2,-0.184615384615385,-0.169230769230769,
-0.153846153846154,-0.138461538461538,-0.123076923076923,-0.107692307692308,
-0.0923076923076923,-0.0769230769230769,-0.0615384615384615,-0.0461538461538462,
-0.0307692307692308,-0.0153846153846154,-0.00577184337451708),
 .UNSPECIFIED.)
CURVE()
GEOMETRIC_REPRESENTATION_ITEM()
RATIONAL_B_SPLINE_CURVE((1.,1.,1.,1.,1.,1.,1.,1.,1.,1.,1.,1.,1.,1.,1.,1.,
1.,1.,1.,1.,1.,1.,1.,1.,1.,1.,1.,1.,1.,1.,1.,1.,1.,1.,1.,1.,1.,1.,1.,1.,
1.,1.,1.,1.,1.,1.,1.,1.,1.,1.,1.,1.,1.,1.,1.,1.,1.,1.,1.,1.,1.,1.,1.,1.,
1.,1.,1.,1.,1.,1.))
REPRESENTATION_ITEM('')
);
#336=(
BOUNDED_CURVE()
B_SPLINE_CURVE(5,(#50053,#50054,#50055,#50056,#50057,#50058,#50059,#50060,
#50061,#50062,#50063,#50064,#50065,#50066,#50067,#50068,#50069,#50070,#50071,
#50072,#50073,#50074,#50075,#50076,#50077,#50078,#50079,#50080,#50081,#50082,
#50083,#50084,#50085,#50086,#50087,#50088,#50089,#50090,#50091,#50092,#50093,
#50094,#50095,#50096,#50097,#50098,#50099,#50100,#50101,#50102,#50103,#50104,
#50105,#50106,#50107,#50108,#50109,#50110,#50111,#50112,#50113,#50114,#50115,
#50116,#50117,#50118,#50119,#50120,#50121,#50122),.UNSPECIFIED.,.F.,.F.)
B_SPLINE_CURVE_WITH_KNOTS((6,1,1,1,1,1,1,1,1,1,1,1,1,1,1,1,1,1,1,1,1,1,
1,1,1,1,1,1,1,1,1,1,1,1,1,1,1,1,1,1,1,1,1,1,1,1,1,1,1,1,1,1,1,1,1,1,1,1,
1,1,1,1,1,1,1,6),(-0.994228156739669,-0.984615384615383,-0.969230769230768,
-0.953846153846152,-0.938461538461537,-0.923076923076922,-0.907692307692306,
-0.892307692307691,-0.876923076923076,-0.86153846153846,-0.846153846153845,
-0.83076923076923,-0.815384615384614,-0.799999999999999,-0.784615384615384,
-0.769230769230768,-0.753846153846153,-0.738461538461538,-0.723076923076922,
-0.707692307692307,-0.692307692307692,-0.676923076923076,-0.661538461538461,
-0.646153846153846,-0.63076923076923,-0.615384615384615,-0.6,-0.584615384615384,
-0.569230769230769,-0.553846153846154,-0.538461538461538,-0.523076923076923,
-0.507692307692308,-0.492307692307692,-0.476923076923077,-0.461538461538462,
-0.446153846153846,-0.430769230769231,-0.415384615384615,-0.4,-0.384615384615385,
-0.369230769230769,-0.353846153846154,-0.338461538461538,-0.323076923076923,
-0.307692307692308,-0.292307692307692,-0.276923076923077,-0.261538461538462,
-0.246153846153846,-0.230769230769231,-0.215384615384615,-0.2,-0.184615384615385,
-0.169230769230769,-0.153846153846154,-0.138461538461538,-0.123076923076923,
-0.107692307692308,-0.0923076923076923,-0.0769230769230769,-0.0615384615384615,
-0.0461538461538462,-0.0307692307692308,-0.0153846153846154,0.),
 .UNSPECIFIED.)
CURVE()
GEOMETRIC_REPRESENTATION_ITEM()
RATIONAL_B_SPLINE_CURVE((1.,1.,1.,1.,1.,1.,1.,1.,1.,1.,1.,1.,1.,1.,1.,1.,
1.,1.,1.,1.,1.,1.,1.,1.,1.,1.,1.,1.,1.,1.,1.,1.,1.,1.,1.,1.,1.,1.,1.,1.,
1.,1.,1.,1.,1.,1.,1.,1.,1.,1.,1.,1.,1.,1.,1.,1.,1.,1.,1.,1.,1.,1.,1.,1.,
1.,1.,1.,1.,1.,1.))
REPRESENTATION_ITEM('')
);
#337=(
BOUNDED_CURVE()
B_SPLINE_CURVE(5,(#50275,#50276,#50277,#50278,#50279,#50280,#50281,#50282,
#50283,#50284,#50285,#50286,#50287,#50288,#50289,#50290,#50291,#50292,#50293,
#50294,#50295,#50296,#50297,#50298,#50299,#50300,#50301,#50302,#50303,#50304,
#50305,#50306,#50307,#50308,#50309,#50310,#50311,#50312,#50313,#50314,#50315,
#50316,#50317,#50318,#50319,#50320,#50321,#50322,#50323,#50324,#50325,#50326,
#50327,#50328,#50329,#50330,#50331,#50332,#50333,#50334,#50335,#50336,#50337,
#50338,#50339,#50340,#50341,#50342,#50343,#50344),.UNSPECIFIED.,.F.,.F.)
B_SPLINE_CURVE_WITH_KNOTS((6,1,1,1,1,1,1,1,1,1,1,1,1,1,1,1,1,1,1,1,1,1,
1,1,1,1,1,1,1,1,1,1,1,1,1,1,1,1,1,1,1,1,1,1,1,1,1,1,1,1,1,1,1,1,1,1,1,1,
1,1,1,1,1,1,1,6),(-1.,-0.984615384615383,-0.969230769230768,-0.953846153846152,
-0.938461538461537,-0.923076923076922,-0.907692307692306,-0.892307692307691,
-0.876923076923076,-0.86153846153846,-0.846153846153845,-0.83076923076923,
-0.815384615384614,-0.799999999999999,-0.784615384615384,-0.769230769230768,
-0.753846153846153,-0.738461538461538,-0.723076923076922,-0.707692307692307,
-0.692307692307692,-0.676923076923076,-0.661538461538461,-0.646153846153846,
-0.63076923076923,-0.615384615384615,-0.6,-0.584615384615384,-0.569230769230769,
-0.553846153846154,-0.538461538461538,-0.523076923076923,-0.507692307692308,
-0.492307692307692,-0.476923076923077,-0.461538461538462,-0.446153846153846,
-0.430769230769231,-0.415384615384615,-0.4,-0.384615384615385,-0.369230769230769,
-0.353846153846154,-0.338461538461538,-0.323076923076923,-0.307692307692308,
-0.292307692307692,-0.276923076923077,-0.261538461538462,-0.246153846153846,
-0.230769230769231,-0.215384615384615,-0.2,-0.184615384615385,-0.169230769230769,
-0.153846153846154,-0.138461538461538,-0.123076923076923,-0.107692307692308,
-0.0923076923076923,-0.0769230769230769,-0.0615384615384615,-0.0461538461538462,
-0.0307692307692308,-0.0153846153846154,-0.0057718433744903),
 .UNSPECIFIED.)
CURVE()
GEOMETRIC_REPRESENTATION_ITEM()
RATIONAL_B_SPLINE_CURVE((1.,1.,1.,1.,1.,1.,1.,1.,1.,1.,1.,1.,1.,1.,1.,1.,
1.,1.,1.,1.,1.,1.,1.,1.,1.,1.,1.,1.,1.,1.,1.,1.,1.,1.,1.,1.,1.,1.,1.,1.,
1.,1.,1.,1.,1.,1.,1.,1.,1.,1.,1.,1.,1.,1.,1.,1.,1.,1.,1.,1.,1.,1.,1.,1.,
1.,1.,1.,1.,1.,1.))
REPRESENTATION_ITEM('')
);
#338=(
BOUNDED_CURVE()
B_SPLINE_CURVE(5,(#50495,#50496,#50497,#50498,#50499,#50500,#50501,#50502,
#50503,#50504,#50505,#50506,#50507,#50508,#50509,#50510,#50511,#50512,#50513,
#50514,#50515,#50516,#50517,#50518,#50519,#50520,#50521,#50522,#50523,#50524,
#50525,#50526,#50527,#50528,#50529,#50530,#50531,#50532,#50533,#50534,#50535,
#50536,#50537,#50538,#50539,#50540,#50541,#50542,#50543,#50544,#50545,#50546,
#50547,#50548,#50549,#50550,#50551,#50552,#50553,#50554,#50555,#50556,#50557,
#50558,#50559,#50560,#50561,#50562,#50563,#50564),.UNSPECIFIED.,.F.,.F.)
B_SPLINE_CURVE_WITH_KNOTS((6,1,1,1,1,1,1,1,1,1,1,1,1,1,1,1,1,1,1,1,1,1,
1,1,1,1,1,1,1,1,1,1,1,1,1,1,1,1,1,1,1,1,1,1,1,1,1,1,1,1,1,1,1,1,1,1,1,1,
1,1,1,1,1,1,1,6),(-0.994228156739712,-0.984615384615383,-0.969230769230768,
-0.953846153846152,-0.938461538461537,-0.923076923076922,-0.907692307692306,
-0.892307692307691,-0.876923076923076,-0.86153846153846,-0.846153846153845,
-0.83076923076923,-0.815384615384614,-0.799999999999999,-0.784615384615384,
-0.769230769230768,-0.753846153846153,-0.738461538461538,-0.723076923076922,
-0.707692307692307,-0.692307692307692,-0.676923076923076,-0.661538461538461,
-0.646153846153846,-0.63076923076923,-0.615384615384615,-0.6,-0.584615384615384,
-0.569230769230769,-0.553846153846154,-0.538461538461538,-0.523076923076923,
-0.507692307692308,-0.492307692307692,-0.476923076923077,-0.461538461538462,
-0.446153846153846,-0.430769230769231,-0.415384615384615,-0.4,-0.384615384615385,
-0.369230769230769,-0.353846153846154,-0.338461538461538,-0.323076923076923,
-0.307692307692308,-0.292307692307692,-0.276923076923077,-0.261538461538462,
-0.246153846153846,-0.230769230769231,-0.215384615384615,-0.2,-0.184615384615385,
-0.169230769230769,-0.153846153846154,-0.138461538461538,-0.123076923076923,
-0.107692307692308,-0.0923076923076923,-0.0769230769230769,-0.0615384615384615,
-0.0461538461538462,-0.0307692307692308,-0.0153846153846154,0.),
 .UNSPECIFIED.)
CURVE()
GEOMETRIC_REPRESENTATION_ITEM()
RATIONAL_B_SPLINE_CURVE((1.,1.,1.,1.,1.,1.,1.,1.,1.,1.,1.,1.,1.,1.,1.,1.,
1.,1.,1.,1.,1.,1.,1.,1.,1.,1.,1.,1.,1.,1.,1.,1.,1.,1.,1.,1.,1.,1.,1.,1.,
1.,1.,1.,1.,1.,1.,1.,1.,1.,1.,1.,1.,1.,1.,1.,1.,1.,1.,1.,1.,1.,1.,1.,1.,
1.,1.,1.,1.,1.,1.))
REPRESENTATION_ITEM('')
);
#339=(
BOUNDED_CURVE()
B_SPLINE_CURVE(5,(#50717,#50718,#50719,#50720,#50721,#50722,#50723,#50724,
#50725,#50726,#50727,#50728,#50729,#50730,#50731,#50732,#50733,#50734,#50735,
#50736,#50737,#50738,#50739,#50740,#50741,#50742,#50743,#50744,#50745,#50746,
#50747,#50748,#50749,#50750,#50751,#50752,#50753,#50754,#50755,#50756,#50757,
#50758,#50759,#50760,#50761,#50762,#50763,#50764,#50765,#50766,#50767,#50768,
#50769,#50770,#50771,#50772,#50773,#50774,#50775,#50776,#50777,#50778,#50779,
#50780,#50781,#50782,#50783,#50784,#50785,#50786),.UNSPECIFIED.,.F.,.F.)
B_SPLINE_CURVE_WITH_KNOTS((6,1,1,1,1,1,1,1,1,1,1,1,1,1,1,1,1,1,1,1,1,1,
1,1,1,1,1,1,1,1,1,1,1,1,1,1,1,1,1,1,1,1,1,1,1,1,1,1,1,1,1,1,1,1,1,1,1,1,
1,1,1,1,1,1,1,6),(-1.,-0.984615384615383,-0.969230769230768,-0.953846153846152,
-0.938461538461537,-0.923076923076922,-0.907692307692306,-0.892307692307691,
-0.876923076923076,-0.86153846153846,-0.846153846153845,-0.83076923076923,
-0.815384615384614,-0.799999999999999,-0.784615384615384,-0.769230769230768,
-0.753846153846153,-0.738461538461538,-0.723076923076922,-0.707692307692307,
-0.692307692307692,-0.676923076923076,-0.661538461538461,-0.646153846153846,
-0.63076923076923,-0.615384615384615,-0.6,-0.584615384615384,-0.569230769230769,
-0.553846153846154,-0.538461538461538,-0.523076923076923,-0.507692307692308,
-0.492307692307692,-0.476923076923077,-0.461538461538462,-0.446153846153846,
-0.430769230769231,-0.415384615384615,-0.4,-0.384615384615385,-0.369230769230769,
-0.353846153846154,-0.338461538461538,-0.323076923076923,-0.307692307692308,
-0.292307692307692,-0.276923076923077,-0.261538461538462,-0.246153846153846,
-0.230769230769231,-0.215384615384615,-0.2,-0.184615384615385,-0.169230769230769,
-0.153846153846154,-0.138461538461538,-0.123076923076923,-0.107692307692308,
-0.0923076923076923,-0.0769230769230769,-0.0615384615384615,-0.0461538461538462,
-0.0307692307692308,-0.0153846153846154,-0.0057718433745291),
 .UNSPECIFIED.)
CURVE()
GEOMETRIC_REPRESENTATION_ITEM()
RATIONAL_B_SPLINE_CURVE((1.,1.,1.,1.,1.,1.,1.,1.,1.,1.,1.,1.,1.,1.,1.,1.,
1.,1.,1.,1.,1.,1.,1.,1.,1.,1.,1.,1.,1.,1.,1.,1.,1.,1.,1.,1.,1.,1.,1.,1.,
1.,1.,1.,1.,1.,1.,1.,1.,1.,1.,1.,1.,1.,1.,1.,1.,1.,1.,1.,1.,1.,1.,1.,1.,
1.,1.,1.,1.,1.,1.))
REPRESENTATION_ITEM('')
);
#340=(
BOUNDED_CURVE()
B_SPLINE_CURVE(5,(#50937,#50938,#50939,#50940,#50941,#50942,#50943,#50944,
#50945,#50946,#50947,#50948,#50949,#50950,#50951,#50952,#50953,#50954,#50955,
#50956,#50957,#50958,#50959,#50960,#50961,#50962,#50963,#50964,#50965,#50966,
#50967,#50968,#50969,#50970,#50971,#50972,#50973,#50974,#50975,#50976,#50977,
#50978,#50979,#50980,#50981,#50982,#50983,#50984,#50985,#50986,#50987,#50988,
#50989,#50990,#50991,#50992,#50993,#50994,#50995,#50996,#50997,#50998,#50999,
#51000,#51001,#51002,#51003,#51004,#51005,#51006),.UNSPECIFIED.,.F.,.F.)
B_SPLINE_CURVE_WITH_KNOTS((6,1,1,1,1,1,1,1,1,1,1,1,1,1,1,1,1,1,1,1,1,1,
1,1,1,1,1,1,1,1,1,1,1,1,1,1,1,1,1,1,1,1,1,1,1,1,1,1,1,1,1,1,1,1,1,1,1,1,
1,1,1,1,1,1,1,6),(-0.994228156739695,-0.984615384615383,-0.969230769230768,
-0.953846153846152,-0.938461538461537,-0.923076923076922,-0.907692307692306,
-0.892307692307691,-0.876923076923076,-0.86153846153846,-0.846153846153845,
-0.83076923076923,-0.815384615384614,-0.799999999999999,-0.784615384615384,
-0.769230769230768,-0.753846153846153,-0.738461538461538,-0.723076923076922,
-0.707692307692307,-0.692307692307692,-0.676923076923076,-0.661538461538461,
-0.646153846153846,-0.63076923076923,-0.615384615384615,-0.6,-0.584615384615384,
-0.569230769230769,-0.553846153846154,-0.538461538461538,-0.523076923076923,
-0.507692307692308,-0.492307692307692,-0.476923076923077,-0.461538461538462,
-0.446153846153846,-0.430769230769231,-0.415384615384615,-0.4,-0.384615384615385,
-0.369230769230769,-0.353846153846154,-0.338461538461538,-0.323076923076923,
-0.307692307692308,-0.292307692307692,-0.276923076923077,-0.261538461538462,
-0.246153846153846,-0.230769230769231,-0.215384615384615,-0.2,-0.184615384615385,
-0.169230769230769,-0.153846153846154,-0.138461538461538,-0.123076923076923,
-0.107692307692308,-0.0923076923076923,-0.0769230769230769,-0.0615384615384615,
-0.0461538461538462,-0.0307692307692308,-0.0153846153846154,0.),
 .UNSPECIFIED.)
CURVE()
GEOMETRIC_REPRESENTATION_ITEM()
RATIONAL_B_SPLINE_CURVE((1.,1.,1.,1.,1.,1.,1.,1.,1.,1.,1.,1.,1.,1.,1.,1.,
1.,1.,1.,1.,1.,1.,1.,1.,1.,1.,1.,1.,1.,1.,1.,1.,1.,1.,1.,1.,1.,1.,1.,1.,
1.,1.,1.,1.,1.,1.,1.,1.,1.,1.,1.,1.,1.,1.,1.,1.,1.,1.,1.,1.,1.,1.,1.,1.,
1.,1.,1.,1.,1.,1.))
REPRESENTATION_ITEM('')
);
#341=(
BOUNDED_CURVE()
B_SPLINE_CURVE(5,(#51159,#51160,#51161,#51162,#51163,#51164,#51165,#51166,
#51167,#51168,#51169,#51170,#51171,#51172,#51173,#51174,#51175,#51176,#51177,
#51178,#51179,#51180,#51181,#51182,#51183,#51184,#51185,#51186,#51187,#51188,
#51189,#51190,#51191,#51192,#51193,#51194,#51195,#51196,#51197,#51198,#51199,
#51200,#51201,#51202,#51203,#51204,#51205,#51206,#51207,#51208,#51209,#51210,
#51211,#51212,#51213,#51214,#51215,#51216,#51217,#51218,#51219,#51220,#51221,
#51222,#51223,#51224,#51225,#51226,#51227,#51228),.UNSPECIFIED.,.F.,.F.)
B_SPLINE_CURVE_WITH_KNOTS((6,1,1,1,1,1,1,1,1,1,1,1,1,1,1,1,1,1,1,1,1,1,
1,1,1,1,1,1,1,1,1,1,1,1,1,1,1,1,1,1,1,1,1,1,1,1,1,1,1,1,1,1,1,1,1,1,1,1,
1,1,1,1,1,1,1,6),(-1.,-0.984615384615383,-0.969230769230768,-0.953846153846152,
-0.938461538461537,-0.923076923076922,-0.907692307692306,-0.892307692307691,
-0.876923076923076,-0.86153846153846,-0.846153846153845,-0.83076923076923,
-0.815384615384614,-0.799999999999999,-0.784615384615384,-0.769230769230768,
-0.753846153846153,-0.738461538461538,-0.723076923076922,-0.707692307692307,
-0.692307692307692,-0.676923076923076,-0.661538461538461,-0.646153846153846,
-0.63076923076923,-0.615384615384615,-0.6,-0.584615384615384,-0.569230769230769,
-0.553846153846154,-0.538461538461538,-0.523076923076923,-0.507692307692308,
-0.492307692307692,-0.476923076923077,-0.461538461538462,-0.446153846153846,
-0.430769230769231,-0.415384615384615,-0.4,-0.384615384615385,-0.369230769230769,
-0.353846153846154,-0.338461538461538,-0.323076923076923,-0.307692307692308,
-0.292307692307692,-0.276923076923077,-0.261538461538462,-0.246153846153846,
-0.230769230769231,-0.215384615384615,-0.2,-0.184615384615385,-0.169230769230769,
-0.153846153846154,-0.138461538461538,-0.123076923076923,-0.107692307692308,
-0.0923076923076923,-0.0769230769230769,-0.0615384615384615,-0.0461538461538462,
-0.0307692307692308,-0.0153846153846154,-0.00577184337450344),
 .UNSPECIFIED.)
CURVE()
GEOMETRIC_REPRESENTATION_ITEM()
RATIONAL_B_SPLINE_CURVE((1.,1.,1.,1.,1.,1.,1.,1.,1.,1.,1.,1.,1.,1.,1.,1.,
1.,1.,1.,1.,1.,1.,1.,1.,1.,1.,1.,1.,1.,1.,1.,1.,1.,1.,1.,1.,1.,1.,1.,1.,
1.,1.,1.,1.,1.,1.,1.,1.,1.,1.,1.,1.,1.,1.,1.,1.,1.,1.,1.,1.,1.,1.,1.,1.,
1.,1.,1.,1.,1.,1.))
REPRESENTATION_ITEM('')
);
#342=(
BOUNDED_CURVE()
B_SPLINE_CURVE(5,(#51379,#51380,#51381,#51382,#51383,#51384,#51385,#51386,
#51387,#51388,#51389,#51390,#51391,#51392,#51393,#51394,#51395,#51396,#51397,
#51398,#51399,#51400,#51401,#51402,#51403,#51404,#51405,#51406,#51407,#51408,
#51409,#51410,#51411,#51412,#51413,#51414,#51415,#51416,#51417,#51418,#51419,
#51420,#51421,#51422,#51423,#51424,#51425,#51426,#51427,#51428,#51429,#51430,
#51431,#51432,#51433,#51434,#51435,#51436,#51437,#51438,#51439,#51440,#51441,
#51442,#51443,#51444,#51445,#51446,#51447,#51448),.UNSPECIFIED.,.F.,.F.)
B_SPLINE_CURVE_WITH_KNOTS((6,1,1,1,1,1,1,1,1,1,1,1,1,1,1,1,1,1,1,1,1,1,
1,1,1,1,1,1,1,1,1,1,1,1,1,1,1,1,1,1,1,1,1,1,1,1,1,1,1,1,1,1,1,1,1,1,1,1,
1,1,1,1,1,1,1,6),(-0.994228156739669,-0.984615384615383,-0.969230769230768,
-0.953846153846152,-0.938461538461537,-0.923076923076922,-0.907692307692306,
-0.892307692307691,-0.876923076923076,-0.86153846153846,-0.846153846153845,
-0.83076923076923,-0.815384615384614,-0.799999999999999,-0.784615384615384,
-0.769230769230768,-0.753846153846153,-0.738461538461538,-0.723076923076922,
-0.707692307692307,-0.692307692307692,-0.676923076923076,-0.661538461538461,
-0.646153846153846,-0.63076923076923,-0.615384615384615,-0.6,-0.584615384615384,
-0.569230769230769,-0.553846153846154,-0.538461538461538,-0.523076923076923,
-0.507692307692308,-0.492307692307692,-0.476923076923077,-0.461538461538462,
-0.446153846153846,-0.430769230769231,-0.415384615384615,-0.4,-0.384615384615385,
-0.369230769230769,-0.353846153846154,-0.338461538461538,-0.323076923076923,
-0.307692307692308,-0.292307692307692,-0.276923076923077,-0.261538461538462,
-0.246153846153846,-0.230769230769231,-0.215384615384615,-0.2,-0.184615384615385,
-0.169230769230769,-0.153846153846154,-0.138461538461538,-0.123076923076923,
-0.107692307692308,-0.0923076923076923,-0.0769230769230769,-0.0615384615384615,
-0.0461538461538462,-0.0307692307692308,-0.0153846153846154,0.),
 .UNSPECIFIED.)
CURVE()
GEOMETRIC_REPRESENTATION_ITEM()
RATIONAL_B_SPLINE_CURVE((1.,1.,1.,1.,1.,1.,1.,1.,1.,1.,1.,1.,1.,1.,1.,1.,
1.,1.,1.,1.,1.,1.,1.,1.,1.,1.,1.,1.,1.,1.,1.,1.,1.,1.,1.,1.,1.,1.,1.,1.,
1.,1.,1.,1.,1.,1.,1.,1.,1.,1.,1.,1.,1.,1.,1.,1.,1.,1.,1.,1.,1.,1.,1.,1.,
1.,1.,1.,1.,1.,1.))
REPRESENTATION_ITEM('')
);
#343=(
BOUNDED_CURVE()
B_SPLINE_CURVE(5,(#51601,#51602,#51603,#51604,#51605,#51606,#51607,#51608,
#51609,#51610,#51611,#51612,#51613,#51614,#51615,#51616,#51617,#51618,#51619,
#51620,#51621,#51622,#51623,#51624,#51625,#51626,#51627,#51628,#51629,#51630,
#51631,#51632,#51633,#51634,#51635,#51636,#51637,#51638,#51639,#51640,#51641,
#51642,#51643,#51644,#51645,#51646,#51647,#51648,#51649,#51650,#51651,#51652,
#51653,#51654,#51655,#51656,#51657,#51658,#51659,#51660,#51661,#51662,#51663,
#51664,#51665,#51666,#51667,#51668,#51669,#51670),.UNSPECIFIED.,.F.,.F.)
B_SPLINE_CURVE_WITH_KNOTS((6,1,1,1,1,1,1,1,1,1,1,1,1,1,1,1,1,1,1,1,1,1,
1,1,1,1,1,1,1,1,1,1,1,1,1,1,1,1,1,1,1,1,1,1,1,1,1,1,1,1,1,1,1,1,1,1,1,1,
1,1,1,1,1,1,1,6),(-1.,-0.984615384615383,-0.969230769230768,-0.953846153846152,
-0.938461538461537,-0.923076923076922,-0.907692307692306,-0.892307692307691,
-0.876923076923076,-0.86153846153846,-0.846153846153845,-0.83076923076923,
-0.815384615384614,-0.799999999999999,-0.784615384615384,-0.769230769230768,
-0.753846153846153,-0.738461538461538,-0.723076923076922,-0.707692307692307,
-0.692307692307692,-0.676923076923076,-0.661538461538461,-0.646153846153846,
-0.63076923076923,-0.615384615384615,-0.6,-0.584615384615384,-0.569230769230769,
-0.553846153846154,-0.538461538461538,-0.523076923076923,-0.507692307692308,
-0.492307692307692,-0.476923076923077,-0.461538461538462,-0.446153846153846,
-0.430769230769231,-0.415384615384615,-0.4,-0.384615384615385,-0.369230769230769,
-0.353846153846154,-0.338461538461538,-0.323076923076923,-0.307692307692308,
-0.292307692307692,-0.276923076923077,-0.261538461538462,-0.246153846153846,
-0.230769230769231,-0.215384615384615,-0.2,-0.184615384615385,-0.169230769230769,
-0.153846153846154,-0.138461538461538,-0.123076923076923,-0.107692307692308,
-0.0923076923076923,-0.0769230769230769,-0.0615384615384615,-0.0461538461538462,
-0.0307692307692308,-0.0153846153846154,-0.00577184337450876),
 .UNSPECIFIED.)
CURVE()
GEOMETRIC_REPRESENTATION_ITEM()
RATIONAL_B_SPLINE_CURVE((1.,1.,1.,1.,1.,1.,1.,1.,1.,1.,1.,1.,1.,1.,1.,1.,
1.,1.,1.,1.,1.,1.,1.,1.,1.,1.,1.,1.,1.,1.,1.,1.,1.,1.,1.,1.,1.,1.,1.,1.,
1.,1.,1.,1.,1.,1.,1.,1.,1.,1.,1.,1.,1.,1.,1.,1.,1.,1.,1.,1.,1.,1.,1.,1.,
1.,1.,1.,1.,1.,1.))
REPRESENTATION_ITEM('')
);
#344=(
BOUNDED_CURVE()
B_SPLINE_CURVE(5,(#51821,#51822,#51823,#51824,#51825,#51826,#51827,#51828,
#51829,#51830,#51831,#51832,#51833,#51834,#51835,#51836,#51837,#51838,#51839,
#51840,#51841,#51842,#51843,#51844,#51845,#51846,#51847,#51848,#51849,#51850,
#51851,#51852,#51853,#51854,#51855,#51856,#51857,#51858,#51859,#51860,#51861,
#51862,#51863,#51864,#51865,#51866,#51867,#51868,#51869,#51870,#51871,#51872,
#51873,#51874,#51875,#51876,#51877,#51878,#51879,#51880,#51881,#51882,#51883,
#51884,#51885,#51886,#51887,#51888,#51889,#51890),.UNSPECIFIED.,.F.,.F.)
B_SPLINE_CURVE_WITH_KNOTS((6,1,1,1,1,1,1,1,1,1,1,1,1,1,1,1,1,1,1,1,1,1,
1,1,1,1,1,1,1,1,1,1,1,1,1,1,1,1,1,1,1,1,1,1,1,1,1,1,1,1,1,1,1,1,1,1,1,1,
1,1,1,1,1,1,1,6),(-0.99422815673966,-0.984615384615383,-0.969230769230768,
-0.953846153846152,-0.938461538461537,-0.923076923076922,-0.907692307692306,
-0.892307692307691,-0.876923076923076,-0.86153846153846,-0.846153846153845,
-0.83076923076923,-0.815384615384614,-0.799999999999999,-0.784615384615384,
-0.769230769230768,-0.753846153846153,-0.738461538461538,-0.723076923076922,
-0.707692307692307,-0.692307692307692,-0.676923076923076,-0.661538461538461,
-0.646153846153846,-0.63076923076923,-0.615384615384615,-0.6,-0.584615384615384,
-0.569230769230769,-0.553846153846154,-0.538461538461538,-0.523076923076923,
-0.507692307692308,-0.492307692307692,-0.476923076923077,-0.461538461538462,
-0.446153846153846,-0.430769230769231,-0.415384615384615,-0.4,-0.384615384615385,
-0.369230769230769,-0.353846153846154,-0.338461538461538,-0.323076923076923,
-0.307692307692308,-0.292307692307692,-0.276923076923077,-0.261538461538462,
-0.246153846153846,-0.230769230769231,-0.215384615384615,-0.2,-0.184615384615385,
-0.169230769230769,-0.153846153846154,-0.138461538461538,-0.123076923076923,
-0.107692307692308,-0.0923076923076923,-0.0769230769230769,-0.0615384615384615,
-0.0461538461538462,-0.0307692307692308,-0.0153846153846154,0.),
 .UNSPECIFIED.)
CURVE()
GEOMETRIC_REPRESENTATION_ITEM()
RATIONAL_B_SPLINE_CURVE((1.,1.,1.,1.,1.,1.,1.,1.,1.,1.,1.,1.,1.,1.,1.,1.,
1.,1.,1.,1.,1.,1.,1.,1.,1.,1.,1.,1.,1.,1.,1.,1.,1.,1.,1.,1.,1.,1.,1.,1.,
1.,1.,1.,1.,1.,1.,1.,1.,1.,1.,1.,1.,1.,1.,1.,1.,1.,1.,1.,1.,1.,1.,1.,1.,
1.,1.,1.,1.,1.,1.))
REPRESENTATION_ITEM('')
);
#345=(
BOUNDED_CURVE()
B_SPLINE_CURVE(5,(#52043,#52044,#52045,#52046,#52047,#52048,#52049,#52050,
#52051,#52052,#52053,#52054,#52055,#52056,#52057,#52058,#52059,#52060,#52061,
#52062,#52063,#52064,#52065,#52066,#52067,#52068,#52069,#52070,#52071,#52072,
#52073,#52074,#52075,#52076,#52077,#52078,#52079,#52080,#52081,#52082,#52083,
#52084,#52085,#52086,#52087,#52088,#52089,#52090,#52091,#52092,#52093,#52094,
#52095,#52096,#52097,#52098,#52099,#52100,#52101,#52102,#52103,#52104,#52105,
#52106,#52107,#52108,#52109,#52110,#52111,#52112),.UNSPECIFIED.,.F.,.F.)
B_SPLINE_CURVE_WITH_KNOTS((6,1,1,1,1,1,1,1,1,1,1,1,1,1,1,1,1,1,1,1,1,1,
1,1,1,1,1,1,1,1,1,1,1,1,1,1,1,1,1,1,1,1,1,1,1,1,1,1,1,1,1,1,1,1,1,1,1,1,
1,1,1,1,1,1,1,6),(-1.,-0.984615384615383,-0.969230769230768,-0.953846153846152,
-0.938461538461537,-0.923076923076922,-0.907692307692306,-0.892307692307691,
-0.876923076923076,-0.86153846153846,-0.846153846153845,-0.83076923076923,
-0.815384615384614,-0.799999999999999,-0.784615384615384,-0.769230769230768,
-0.753846153846153,-0.738461538461538,-0.723076923076922,-0.707692307692307,
-0.692307692307692,-0.676923076923076,-0.661538461538461,-0.646153846153846,
-0.63076923076923,-0.615384615384615,-0.6,-0.584615384615384,-0.569230769230769,
-0.553846153846154,-0.538461538461538,-0.523076923076923,-0.507692307692308,
-0.492307692307692,-0.476923076923077,-0.461538461538462,-0.446153846153846,
-0.430769230769231,-0.415384615384615,-0.4,-0.384615384615385,-0.369230769230769,
-0.353846153846154,-0.338461538461538,-0.323076923076923,-0.307692307692308,
-0.292307692307692,-0.276923076923077,-0.261538461538462,-0.246153846153846,
-0.230769230769231,-0.215384615384615,-0.2,-0.184615384615385,-0.169230769230769,
-0.153846153846154,-0.138461538461538,-0.123076923076923,-0.107692307692308,
-0.0923076923076923,-0.0769230769230769,-0.0615384615384615,-0.0461538461538462,
-0.0307692307692308,-0.0153846153846154,-0.00577184337451051),
 .UNSPECIFIED.)
CURVE()
GEOMETRIC_REPRESENTATION_ITEM()
RATIONAL_B_SPLINE_CURVE((1.,1.,1.,1.,1.,1.,1.,1.,1.,1.,1.,1.,1.,1.,1.,1.,
1.,1.,1.,1.,1.,1.,1.,1.,1.,1.,1.,1.,1.,1.,1.,1.,1.,1.,1.,1.,1.,1.,1.,1.,
1.,1.,1.,1.,1.,1.,1.,1.,1.,1.,1.,1.,1.,1.,1.,1.,1.,1.,1.,1.,1.,1.,1.,1.,
1.,1.,1.,1.,1.,1.))
REPRESENTATION_ITEM('')
);
#346=(
BOUNDED_CURVE()
B_SPLINE_CURVE(5,(#52263,#52264,#52265,#52266,#52267,#52268,#52269,#52270,
#52271,#52272,#52273,#52274,#52275,#52276,#52277,#52278,#52279,#52280,#52281,
#52282,#52283,#52284,#52285,#52286,#52287,#52288,#52289,#52290,#52291,#52292,
#52293,#52294,#52295,#52296,#52297,#52298,#52299,#52300,#52301,#52302,#52303,
#52304,#52305,#52306,#52307,#52308,#52309,#52310,#52311,#52312,#52313,#52314,
#52315,#52316,#52317,#52318,#52319,#52320,#52321,#52322,#52323,#52324,#52325,
#52326,#52327,#52328,#52329,#52330,#52331,#52332),.UNSPECIFIED.,.F.,.F.)
B_SPLINE_CURVE_WITH_KNOTS((6,1,1,1,1,1,1,1,1,1,1,1,1,1,1,1,1,1,1,1,1,1,
1,1,1,1,1,1,1,1,1,1,1,1,1,1,1,1,1,1,1,1,1,1,1,1,1,1,1,1,1,1,1,1,1,1,1,1,
1,1,1,1,1,1,1,6),(-0.994228156739678,-0.984615384615383,-0.969230769230768,
-0.953846153846152,-0.938461538461537,-0.923076923076922,-0.907692307692306,
-0.892307692307691,-0.876923076923076,-0.86153846153846,-0.846153846153845,
-0.83076923076923,-0.815384615384614,-0.799999999999999,-0.784615384615384,
-0.769230769230768,-0.753846153846153,-0.738461538461538,-0.723076923076922,
-0.707692307692307,-0.692307692307692,-0.676923076923076,-0.661538461538461,
-0.646153846153846,-0.63076923076923,-0.615384615384615,-0.6,-0.584615384615384,
-0.569230769230769,-0.553846153846154,-0.538461538461538,-0.523076923076923,
-0.507692307692308,-0.492307692307692,-0.476923076923077,-0.461538461538462,
-0.446153846153846,-0.430769230769231,-0.415384615384615,-0.4,-0.384615384615385,
-0.369230769230769,-0.353846153846154,-0.338461538461538,-0.323076923076923,
-0.307692307692308,-0.292307692307692,-0.276923076923077,-0.261538461538462,
-0.246153846153846,-0.230769230769231,-0.215384615384615,-0.2,-0.184615384615385,
-0.169230769230769,-0.153846153846154,-0.138461538461538,-0.123076923076923,
-0.107692307692308,-0.0923076923076923,-0.0769230769230769,-0.0615384615384615,
-0.0461538461538462,-0.0307692307692308,-0.0153846153846154,0.),
 .UNSPECIFIED.)
CURVE()
GEOMETRIC_REPRESENTATION_ITEM()
RATIONAL_B_SPLINE_CURVE((1.,1.,1.,1.,1.,1.,1.,1.,1.,1.,1.,1.,1.,1.,1.,1.,
1.,1.,1.,1.,1.,1.,1.,1.,1.,1.,1.,1.,1.,1.,1.,1.,1.,1.,1.,1.,1.,1.,1.,1.,
1.,1.,1.,1.,1.,1.,1.,1.,1.,1.,1.,1.,1.,1.,1.,1.,1.,1.,1.,1.,1.,1.,1.,1.,
1.,1.,1.,1.,1.,1.))
REPRESENTATION_ITEM('')
);
#347=(
BOUNDED_CURVE()
B_SPLINE_CURVE(5,(#52485,#52486,#52487,#52488,#52489,#52490,#52491,#52492,
#52493,#52494,#52495,#52496,#52497,#52498,#52499,#52500,#52501,#52502,#52503,
#52504,#52505,#52506,#52507,#52508,#52509,#52510,#52511,#52512,#52513,#52514,
#52515,#52516,#52517,#52518,#52519,#52520,#52521,#52522,#52523,#52524,#52525,
#52526,#52527,#52528,#52529,#52530,#52531,#52532,#52533,#52534,#52535,#52536,
#52537,#52538,#52539,#52540,#52541,#52542,#52543,#52544,#52545,#52546,#52547,
#52548,#52549,#52550,#52551,#52552,#52553,#52554),.UNSPECIFIED.,.F.,.F.)
B_SPLINE_CURVE_WITH_KNOTS((6,1,1,1,1,1,1,1,1,1,1,1,1,1,1,1,1,1,1,1,1,1,
1,1,1,1,1,1,1,1,1,1,1,1,1,1,1,1,1,1,1,1,1,1,1,1,1,1,1,1,1,1,1,1,1,1,1,1,
1,1,1,1,1,1,1,6),(-1.,-0.984615384615383,-0.969230769230768,-0.953846153846152,
-0.938461538461537,-0.923076923076922,-0.907692307692306,-0.892307692307691,
-0.876923076923076,-0.86153846153846,-0.846153846153845,-0.83076923076923,
-0.815384615384614,-0.799999999999999,-0.784615384615384,-0.769230769230768,
-0.753846153846153,-0.738461538461538,-0.723076923076922,-0.707692307692307,
-0.692307692307692,-0.676923076923076,-0.661538461538461,-0.646153846153846,
-0.63076923076923,-0.615384615384615,-0.6,-0.584615384615384,-0.569230769230769,
-0.553846153846154,-0.538461538461538,-0.523076923076923,-0.507692307692308,
-0.492307692307692,-0.476923076923077,-0.461538461538462,-0.446153846153846,
-0.430769230769231,-0.415384615384615,-0.4,-0.384615384615385,-0.369230769230769,
-0.353846153846154,-0.338461538461538,-0.323076923076923,-0.307692307692308,
-0.292307692307692,-0.276923076923077,-0.261538461538462,-0.246153846153846,
-0.230769230769231,-0.215384615384615,-0.2,-0.184615384615385,-0.169230769230769,
-0.153846153846154,-0.138461538461538,-0.123076923076923,-0.107692307692308,
-0.0923076923076923,-0.0769230769230769,-0.0615384615384615,-0.0461538461538462,
-0.0307692307692308,-0.0153846153846154,-0.0057718433745179),
 .UNSPECIFIED.)
CURVE()
GEOMETRIC_REPRESENTATION_ITEM()
RATIONAL_B_SPLINE_CURVE((1.,1.,1.,1.,1.,1.,1.,1.,1.,1.,1.,1.,1.,1.,1.,1.,
1.,1.,1.,1.,1.,1.,1.,1.,1.,1.,1.,1.,1.,1.,1.,1.,1.,1.,1.,1.,1.,1.,1.,1.,
1.,1.,1.,1.,1.,1.,1.,1.,1.,1.,1.,1.,1.,1.,1.,1.,1.,1.,1.,1.,1.,1.,1.,1.,
1.,1.,1.,1.,1.,1.))
REPRESENTATION_ITEM('')
);
#348=(
BOUNDED_CURVE()
B_SPLINE_CURVE(5,(#52705,#52706,#52707,#52708,#52709,#52710,#52711,#52712,
#52713,#52714,#52715,#52716,#52717,#52718,#52719,#52720,#52721,#52722,#52723,
#52724,#52725,#52726,#52727,#52728,#52729,#52730,#52731,#52732,#52733,#52734,
#52735,#52736,#52737,#52738,#52739,#52740,#52741,#52742,#52743,#52744,#52745,
#52746,#52747,#52748,#52749,#52750,#52751,#52752,#52753,#52754,#52755,#52756,
#52757,#52758,#52759,#52760,#52761,#52762,#52763,#52764,#52765,#52766,#52767,
#52768,#52769,#52770,#52771,#52772,#52773,#52774),.UNSPECIFIED.,.F.,.F.)
B_SPLINE_CURVE_WITH_KNOTS((6,1,1,1,1,1,1,1,1,1,1,1,1,1,1,1,1,1,1,1,1,1,
1,1,1,1,1,1,1,1,1,1,1,1,1,1,1,1,1,1,1,1,1,1,1,1,1,1,1,1,1,1,1,1,1,1,1,1,
1,1,1,1,1,1,1,6),(-0.99422815673967,-0.984615384615383,-0.969230769230768,
-0.953846153846152,-0.938461538461537,-0.923076923076922,-0.907692307692306,
-0.892307692307691,-0.876923076923076,-0.86153846153846,-0.846153846153845,
-0.83076923076923,-0.815384615384614,-0.799999999999999,-0.784615384615384,
-0.769230769230768,-0.753846153846153,-0.738461538461538,-0.723076923076922,
-0.707692307692307,-0.692307692307692,-0.676923076923076,-0.661538461538461,
-0.646153846153846,-0.63076923076923,-0.615384615384615,-0.6,-0.584615384615384,
-0.569230769230769,-0.553846153846154,-0.538461538461538,-0.523076923076923,
-0.507692307692308,-0.492307692307692,-0.476923076923077,-0.461538461538462,
-0.446153846153846,-0.430769230769231,-0.415384615384615,-0.4,-0.384615384615385,
-0.369230769230769,-0.353846153846154,-0.338461538461538,-0.323076923076923,
-0.307692307692308,-0.292307692307692,-0.276923076923077,-0.261538461538462,
-0.246153846153846,-0.230769230769231,-0.215384615384615,-0.2,-0.184615384615385,
-0.169230769230769,-0.153846153846154,-0.138461538461538,-0.123076923076923,
-0.107692307692308,-0.0923076923076923,-0.0769230769230769,-0.0615384615384615,
-0.0461538461538462,-0.0307692307692308,-0.0153846153846154,0.),
 .UNSPECIFIED.)
CURVE()
GEOMETRIC_REPRESENTATION_ITEM()
RATIONAL_B_SPLINE_CURVE((1.,1.,1.,1.,1.,1.,1.,1.,1.,1.,1.,1.,1.,1.,1.,1.,
1.,1.,1.,1.,1.,1.,1.,1.,1.,1.,1.,1.,1.,1.,1.,1.,1.,1.,1.,1.,1.,1.,1.,1.,
1.,1.,1.,1.,1.,1.,1.,1.,1.,1.,1.,1.,1.,1.,1.,1.,1.,1.,1.,1.,1.,1.,1.,1.,
1.,1.,1.,1.,1.,1.))
REPRESENTATION_ITEM('')
);
#349=(
BOUNDED_CURVE()
B_SPLINE_CURVE(5,(#52927,#52928,#52929,#52930,#52931,#52932,#52933,#52934,
#52935,#52936,#52937,#52938,#52939,#52940,#52941,#52942,#52943,#52944,#52945,
#52946,#52947,#52948,#52949,#52950,#52951,#52952,#52953,#52954,#52955,#52956,
#52957,#52958,#52959,#52960,#52961,#52962,#52963,#52964,#52965,#52966,#52967,
#52968,#52969,#52970,#52971,#52972,#52973,#52974,#52975,#52976,#52977,#52978,
#52979,#52980,#52981,#52982,#52983,#52984,#52985,#52986,#52987,#52988,#52989,
#52990,#52991,#52992,#52993,#52994,#52995,#52996),.UNSPECIFIED.,.F.,.F.)
B_SPLINE_CURVE_WITH_KNOTS((6,1,1,1,1,1,1,1,1,1,1,1,1,1,1,1,1,1,1,1,1,1,
1,1,1,1,1,1,1,1,1,1,1,1,1,1,1,1,1,1,1,1,1,1,1,1,1,1,1,1,1,1,1,1,1,1,1,1,
1,1,1,1,1,1,1,6),(-1.,-0.984615384615383,-0.969230769230768,-0.953846153846152,
-0.938461538461537,-0.923076923076922,-0.907692307692306,-0.892307692307691,
-0.876923076923076,-0.86153846153846,-0.846153846153845,-0.83076923076923,
-0.815384615384614,-0.799999999999999,-0.784615384615384,-0.769230769230768,
-0.753846153846153,-0.738461538461538,-0.723076923076922,-0.707692307692307,
-0.692307692307692,-0.676923076923076,-0.661538461538461,-0.646153846153846,
-0.63076923076923,-0.615384615384615,-0.6,-0.584615384615384,-0.569230769230769,
-0.553846153846154,-0.538461538461538,-0.523076923076923,-0.507692307692308,
-0.492307692307692,-0.476923076923077,-0.461538461538462,-0.446153846153846,
-0.430769230769231,-0.415384615384615,-0.4,-0.384615384615385,-0.369230769230769,
-0.353846153846154,-0.338461538461538,-0.323076923076923,-0.307692307692308,
-0.292307692307692,-0.276923076923077,-0.261538461538462,-0.246153846153846,
-0.230769230769231,-0.215384615384615,-0.2,-0.184615384615385,-0.169230769230769,
-0.153846153846154,-0.138461538461538,-0.123076923076923,-0.107692307692308,
-0.0923076923076923,-0.0769230769230769,-0.0615384615384615,-0.0461538461538462,
-0.0307692307692308,-0.0153846153846154,-0.00577184337452479),
 .UNSPECIFIED.)
CURVE()
GEOMETRIC_REPRESENTATION_ITEM()
RATIONAL_B_SPLINE_CURVE((1.,1.,1.,1.,1.,1.,1.,1.,1.,1.,1.,1.,1.,1.,1.,1.,
1.,1.,1.,1.,1.,1.,1.,1.,1.,1.,1.,1.,1.,1.,1.,1.,1.,1.,1.,1.,1.,1.,1.,1.,
1.,1.,1.,1.,1.,1.,1.,1.,1.,1.,1.,1.,1.,1.,1.,1.,1.,1.,1.,1.,1.,1.,1.,1.,
1.,1.,1.,1.,1.,1.))
REPRESENTATION_ITEM('')
);
#350=(
BOUNDED_CURVE()
B_SPLINE_CURVE(5,(#53147,#53148,#53149,#53150,#53151,#53152,#53153,#53154,
#53155,#53156,#53157,#53158,#53159,#53160,#53161,#53162,#53163,#53164,#53165,
#53166,#53167,#53168,#53169,#53170,#53171,#53172,#53173,#53174,#53175,#53176,
#53177,#53178,#53179,#53180,#53181,#53182,#53183,#53184,#53185,#53186,#53187,
#53188,#53189,#53190,#53191,#53192,#53193,#53194,#53195,#53196,#53197,#53198,
#53199,#53200,#53201,#53202,#53203,#53204,#53205,#53206,#53207,#53208,#53209,
#53210,#53211,#53212,#53213,#53214,#53215,#53216),.UNSPECIFIED.,.F.,.F.)
B_SPLINE_CURVE_WITH_KNOTS((6,1,1,1,1,1,1,1,1,1,1,1,1,1,1,1,1,1,1,1,1,1,
1,1,1,1,1,1,1,1,1,1,1,1,1,1,1,1,1,1,1,1,1,1,1,1,1,1,1,1,1,1,1,1,1,1,1,1,
1,1,1,1,1,1,1,6),(-0.99422815673967,-0.984615384615383,-0.969230769230768,
-0.953846153846152,-0.938461538461537,-0.923076923076922,-0.907692307692306,
-0.892307692307691,-0.876923076923076,-0.86153846153846,-0.846153846153845,
-0.83076923076923,-0.815384615384614,-0.799999999999999,-0.784615384615384,
-0.769230769230768,-0.753846153846153,-0.738461538461538,-0.723076923076922,
-0.707692307692307,-0.692307692307692,-0.676923076923076,-0.661538461538461,
-0.646153846153846,-0.63076923076923,-0.615384615384615,-0.6,-0.584615384615384,
-0.569230769230769,-0.553846153846154,-0.538461538461538,-0.523076923076923,
-0.507692307692308,-0.492307692307692,-0.476923076923077,-0.461538461538462,
-0.446153846153846,-0.430769230769231,-0.415384615384615,-0.4,-0.384615384615385,
-0.369230769230769,-0.353846153846154,-0.338461538461538,-0.323076923076923,
-0.307692307692308,-0.292307692307692,-0.276923076923077,-0.261538461538462,
-0.246153846153846,-0.230769230769231,-0.215384615384615,-0.2,-0.184615384615385,
-0.169230769230769,-0.153846153846154,-0.138461538461538,-0.123076923076923,
-0.107692307692308,-0.0923076923076923,-0.0769230769230769,-0.0615384615384615,
-0.0461538461538462,-0.0307692307692308,-0.0153846153846154,0.),
 .UNSPECIFIED.)
CURVE()
GEOMETRIC_REPRESENTATION_ITEM()
RATIONAL_B_SPLINE_CURVE((1.,1.,1.,1.,1.,1.,1.,1.,1.,1.,1.,1.,1.,1.,1.,1.,
1.,1.,1.,1.,1.,1.,1.,1.,1.,1.,1.,1.,1.,1.,1.,1.,1.,1.,1.,1.,1.,1.,1.,1.,
1.,1.,1.,1.,1.,1.,1.,1.,1.,1.,1.,1.,1.,1.,1.,1.,1.,1.,1.,1.,1.,1.,1.,1.,
1.,1.,1.,1.,1.,1.))
REPRESENTATION_ITEM('')
);
#351=(
BOUNDED_CURVE()
B_SPLINE_CURVE(5,(#53369,#53370,#53371,#53372,#53373,#53374,#53375,#53376,
#53377,#53378,#53379,#53380,#53381,#53382,#53383,#53384,#53385,#53386,#53387,
#53388,#53389,#53390,#53391,#53392,#53393,#53394,#53395,#53396,#53397,#53398,
#53399,#53400,#53401,#53402,#53403,#53404,#53405,#53406,#53407,#53408,#53409,
#53410,#53411,#53412,#53413,#53414,#53415,#53416,#53417,#53418,#53419,#53420,
#53421,#53422,#53423,#53424,#53425,#53426,#53427,#53428,#53429,#53430,#53431,
#53432,#53433,#53434,#53435,#53436,#53437,#53438),.UNSPECIFIED.,.F.,.F.)
B_SPLINE_CURVE_WITH_KNOTS((6,1,1,1,1,1,1,1,1,1,1,1,1,1,1,1,1,1,1,1,1,1,
1,1,1,1,1,1,1,1,1,1,1,1,1,1,1,1,1,1,1,1,1,1,1,1,1,1,1,1,1,1,1,1,1,1,1,1,
1,1,1,1,1,1,1,6),(-1.,-0.984615384615383,-0.969230769230768,-0.953846153846152,
-0.938461538461537,-0.923076923076922,-0.907692307692306,-0.892307692307691,
-0.876923076923076,-0.86153846153846,-0.846153846153845,-0.83076923076923,
-0.815384615384614,-0.799999999999999,-0.784615384615384,-0.769230769230768,
-0.753846153846153,-0.738461538461538,-0.723076923076922,-0.707692307692307,
-0.692307692307692,-0.676923076923076,-0.661538461538461,-0.646153846153846,
-0.63076923076923,-0.615384615384615,-0.6,-0.584615384615384,-0.569230769230769,
-0.553846153846154,-0.538461538461538,-0.523076923076923,-0.507692307692308,
-0.492307692307692,-0.476923076923077,-0.461538461538462,-0.446153846153846,
-0.430769230769231,-0.415384615384615,-0.4,-0.384615384615385,-0.369230769230769,
-0.353846153846154,-0.338461538461538,-0.323076923076923,-0.307692307692308,
-0.292307692307692,-0.276923076923077,-0.261538461538462,-0.246153846153846,
-0.230769230769231,-0.215384615384615,-0.2,-0.184615384615385,-0.169230769230769,
-0.153846153846154,-0.138461538461538,-0.123076923076923,-0.107692307692308,
-0.0923076923076923,-0.0769230769230769,-0.0615384615384615,-0.0461538461538462,
-0.0307692307692308,-0.0153846153846154,-0.0057718433745009),
 .UNSPECIFIED.)
CURVE()
GEOMETRIC_REPRESENTATION_ITEM()
RATIONAL_B_SPLINE_CURVE((1.,1.,1.,1.,1.,1.,1.,1.,1.,1.,1.,1.,1.,1.,1.,1.,
1.,1.,1.,1.,1.,1.,1.,1.,1.,1.,1.,1.,1.,1.,1.,1.,1.,1.,1.,1.,1.,1.,1.,1.,
1.,1.,1.,1.,1.,1.,1.,1.,1.,1.,1.,1.,1.,1.,1.,1.,1.,1.,1.,1.,1.,1.,1.,1.,
1.,1.,1.,1.,1.,1.))
REPRESENTATION_ITEM('')
);
#352=(
BOUNDED_CURVE()
B_SPLINE_CURVE(5,(#53589,#53590,#53591,#53592,#53593,#53594,#53595,#53596,
#53597,#53598,#53599,#53600,#53601,#53602,#53603,#53604,#53605,#53606,#53607,
#53608,#53609,#53610,#53611,#53612,#53613,#53614,#53615,#53616,#53617,#53618,
#53619,#53620,#53621,#53622,#53623,#53624,#53625,#53626,#53627,#53628,#53629,
#53630,#53631,#53632,#53633,#53634,#53635,#53636,#53637,#53638,#53639,#53640,
#53641,#53642,#53643,#53644,#53645,#53646,#53647,#53648,#53649,#53650,#53651,
#53652,#53653,#53654,#53655,#53656,#53657,#53658),.UNSPECIFIED.,.F.,.F.)
B_SPLINE_CURVE_WITH_KNOTS((6,1,1,1,1,1,1,1,1,1,1,1,1,1,1,1,1,1,1,1,1,1,
1,1,1,1,1,1,1,1,1,1,1,1,1,1,1,1,1,1,1,1,1,1,1,1,1,1,1,1,1,1,1,1,1,1,1,1,
1,1,1,1,1,1,1,6),(-0.99422815673967,-0.984615384615383,-0.969230769230768,
-0.953846153846152,-0.938461538461537,-0.923076923076922,-0.907692307692306,
-0.892307692307691,-0.876923076923076,-0.86153846153846,-0.846153846153845,
-0.83076923076923,-0.815384615384614,-0.799999999999999,-0.784615384615384,
-0.769230769230768,-0.753846153846153,-0.738461538461538,-0.723076923076922,
-0.707692307692307,-0.692307692307692,-0.676923076923076,-0.661538461538461,
-0.646153846153846,-0.63076923076923,-0.615384615384615,-0.6,-0.584615384615384,
-0.569230769230769,-0.553846153846154,-0.538461538461538,-0.523076923076923,
-0.507692307692308,-0.492307692307692,-0.476923076923077,-0.461538461538462,
-0.446153846153846,-0.430769230769231,-0.415384615384615,-0.4,-0.384615384615385,
-0.369230769230769,-0.353846153846154,-0.338461538461538,-0.323076923076923,
-0.307692307692308,-0.292307692307692,-0.276923076923077,-0.261538461538462,
-0.246153846153846,-0.230769230769231,-0.215384615384615,-0.2,-0.184615384615385,
-0.169230769230769,-0.153846153846154,-0.138461538461538,-0.123076923076923,
-0.107692307692308,-0.0923076923076923,-0.0769230769230769,-0.0615384615384615,
-0.0461538461538462,-0.0307692307692308,-0.0153846153846154,0.),
 .UNSPECIFIED.)
CURVE()
GEOMETRIC_REPRESENTATION_ITEM()
RATIONAL_B_SPLINE_CURVE((1.,1.,1.,1.,1.,1.,1.,1.,1.,1.,1.,1.,1.,1.,1.,1.,
1.,1.,1.,1.,1.,1.,1.,1.,1.,1.,1.,1.,1.,1.,1.,1.,1.,1.,1.,1.,1.,1.,1.,1.,
1.,1.,1.,1.,1.,1.,1.,1.,1.,1.,1.,1.,1.,1.,1.,1.,1.,1.,1.,1.,1.,1.,1.,1.,
1.,1.,1.,1.,1.,1.))
REPRESENTATION_ITEM('')
);
#353=(
BOUNDED_CURVE()
B_SPLINE_CURVE(5,(#53811,#53812,#53813,#53814,#53815,#53816,#53817,#53818,
#53819,#53820,#53821,#53822,#53823,#53824,#53825,#53826,#53827,#53828,#53829,
#53830,#53831,#53832,#53833,#53834,#53835,#53836,#53837,#53838,#53839,#53840,
#53841,#53842,#53843,#53844,#53845,#53846,#53847,#53848,#53849,#53850,#53851,
#53852,#53853,#53854,#53855,#53856,#53857,#53858,#53859,#53860,#53861,#53862,
#53863,#53864,#53865,#53866,#53867,#53868,#53869,#53870,#53871,#53872,#53873,
#53874,#53875,#53876,#53877,#53878,#53879,#53880),.UNSPECIFIED.,.F.,.F.)
B_SPLINE_CURVE_WITH_KNOTS((6,1,1,1,1,1,1,1,1,1,1,1,1,1,1,1,1,1,1,1,1,1,
1,1,1,1,1,1,1,1,1,1,1,1,1,1,1,1,1,1,1,1,1,1,1,1,1,1,1,1,1,1,1,1,1,1,1,1,
1,1,1,1,1,1,1,6),(-1.,-0.984615384615383,-0.969230769230768,-0.953846153846152,
-0.938461538461537,-0.923076923076922,-0.907692307692306,-0.892307692307691,
-0.876923076923076,-0.86153846153846,-0.846153846153845,-0.83076923076923,
-0.815384615384614,-0.799999999999999,-0.784615384615384,-0.769230769230768,
-0.753846153846153,-0.738461538461538,-0.723076923076922,-0.707692307692307,
-0.692307692307692,-0.676923076923076,-0.661538461538461,-0.646153846153846,
-0.63076923076923,-0.615384615384615,-0.6,-0.584615384615384,-0.569230769230769,
-0.553846153846154,-0.538461538461538,-0.523076923076923,-0.507692307692308,
-0.492307692307692,-0.476923076923077,-0.461538461538462,-0.446153846153846,
-0.430769230769231,-0.415384615384615,-0.4,-0.384615384615385,-0.369230769230769,
-0.353846153846154,-0.338461538461538,-0.323076923076923,-0.307692307692308,
-0.292307692307692,-0.276923076923077,-0.261538461538462,-0.246153846153846,
-0.230769230769231,-0.215384615384615,-0.2,-0.184615384615385,-0.169230769230769,
-0.153846153846154,-0.138461538461538,-0.123076923076923,-0.107692307692308,
-0.0923076923076923,-0.0769230769230769,-0.0615384615384615,-0.0461538461538462,
-0.0307692307692308,-0.0153846153846154,-0.00577184337450701),
 .UNSPECIFIED.)
CURVE()
GEOMETRIC_REPRESENTATION_ITEM()
RATIONAL_B_SPLINE_CURVE((1.,1.,1.,1.,1.,1.,1.,1.,1.,1.,1.,1.,1.,1.,1.,1.,
1.,1.,1.,1.,1.,1.,1.,1.,1.,1.,1.,1.,1.,1.,1.,1.,1.,1.,1.,1.,1.,1.,1.,1.,
1.,1.,1.,1.,1.,1.,1.,1.,1.,1.,1.,1.,1.,1.,1.,1.,1.,1.,1.,1.,1.,1.,1.,1.,
1.,1.,1.,1.,1.,1.))
REPRESENTATION_ITEM('')
);
#354=(
BOUNDED_CURVE()
B_SPLINE_CURVE(5,(#54031,#54032,#54033,#54034,#54035,#54036,#54037,#54038,
#54039,#54040,#54041,#54042,#54043,#54044,#54045,#54046,#54047,#54048,#54049,
#54050,#54051,#54052,#54053,#54054,#54055,#54056,#54057,#54058,#54059,#54060,
#54061,#54062,#54063,#54064,#54065,#54066,#54067,#54068,#54069,#54070,#54071,
#54072,#54073,#54074,#54075,#54076,#54077,#54078,#54079,#54080,#54081,#54082,
#54083,#54084,#54085,#54086,#54087,#54088,#54089,#54090,#54091,#54092,#54093,
#54094,#54095,#54096,#54097,#54098,#54099,#54100),.UNSPECIFIED.,.F.,.F.)
B_SPLINE_CURVE_WITH_KNOTS((6,1,1,1,1,1,1,1,1,1,1,1,1,1,1,1,1,1,1,1,1,1,
1,1,1,1,1,1,1,1,1,1,1,1,1,1,1,1,1,1,1,1,1,1,1,1,1,1,1,1,1,1,1,1,1,1,1,1,
1,1,1,1,1,1,1,6),(-0.994228156739689,-0.984615384615383,-0.969230769230768,
-0.953846153846152,-0.938461538461537,-0.923076923076922,-0.907692307692306,
-0.892307692307691,-0.876923076923076,-0.86153846153846,-0.846153846153845,
-0.83076923076923,-0.815384615384614,-0.799999999999999,-0.784615384615384,
-0.769230769230768,-0.753846153846153,-0.738461538461538,-0.723076923076922,
-0.707692307692307,-0.692307692307692,-0.676923076923076,-0.661538461538461,
-0.646153846153846,-0.63076923076923,-0.615384615384615,-0.6,-0.584615384615384,
-0.569230769230769,-0.553846153846154,-0.538461538461538,-0.523076923076923,
-0.507692307692308,-0.492307692307692,-0.476923076923077,-0.461538461538462,
-0.446153846153846,-0.430769230769231,-0.415384615384615,-0.4,-0.384615384615385,
-0.369230769230769,-0.353846153846154,-0.338461538461538,-0.323076923076923,
-0.307692307692308,-0.292307692307692,-0.276923076923077,-0.261538461538462,
-0.246153846153846,-0.230769230769231,-0.215384615384615,-0.2,-0.184615384615385,
-0.169230769230769,-0.153846153846154,-0.138461538461538,-0.123076923076923,
-0.107692307692308,-0.0923076923076923,-0.0769230769230769,-0.0615384615384615,
-0.0461538461538462,-0.0307692307692308,-0.0153846153846154,0.),
 .UNSPECIFIED.)
CURVE()
GEOMETRIC_REPRESENTATION_ITEM()
RATIONAL_B_SPLINE_CURVE((1.,1.,1.,1.,1.,1.,1.,1.,1.,1.,1.,1.,1.,1.,1.,1.,
1.,1.,1.,1.,1.,1.,1.,1.,1.,1.,1.,1.,1.,1.,1.,1.,1.,1.,1.,1.,1.,1.,1.,1.,
1.,1.,1.,1.,1.,1.,1.,1.,1.,1.,1.,1.,1.,1.,1.,1.,1.,1.,1.,1.,1.,1.,1.,1.,
1.,1.,1.,1.,1.,1.))
REPRESENTATION_ITEM('')
);
#355=(
BOUNDED_CURVE()
B_SPLINE_CURVE(5,(#54253,#54254,#54255,#54256,#54257,#54258,#54259,#54260,
#54261,#54262,#54263,#54264,#54265,#54266,#54267,#54268,#54269,#54270,#54271,
#54272,#54273,#54274,#54275,#54276,#54277,#54278,#54279,#54280,#54281,#54282,
#54283,#54284,#54285,#54286,#54287,#54288,#54289,#54290,#54291,#54292,#54293,
#54294,#54295,#54296,#54297,#54298,#54299,#54300,#54301,#54302,#54303,#54304,
#54305,#54306,#54307,#54308,#54309,#54310,#54311,#54312,#54313,#54314,#54315,
#54316,#54317,#54318,#54319,#54320,#54321,#54322),.UNSPECIFIED.,.F.,.F.)
B_SPLINE_CURVE_WITH_KNOTS((6,1,1,1,1,1,1,1,1,1,1,1,1,1,1,1,1,1,1,1,1,1,
1,1,1,1,1,1,1,1,1,1,1,1,1,1,1,1,1,1,1,1,1,1,1,1,1,1,1,1,1,1,1,1,1,1,1,1,
1,1,1,1,1,1,1,6),(-1.,-0.984615384615383,-0.969230769230768,-0.953846153846152,
-0.938461538461537,-0.923076923076922,-0.907692307692306,-0.892307692307691,
-0.876923076923076,-0.86153846153846,-0.846153846153845,-0.83076923076923,
-0.815384615384614,-0.799999999999999,-0.784615384615384,-0.769230769230768,
-0.753846153846153,-0.738461538461538,-0.723076923076922,-0.707692307692307,
-0.692307692307692,-0.676923076923076,-0.661538461538461,-0.646153846153846,
-0.63076923076923,-0.615384615384615,-0.6,-0.584615384615384,-0.569230769230769,
-0.553846153846154,-0.538461538461538,-0.523076923076923,-0.507692307692308,
-0.492307692307692,-0.476923076923077,-0.461538461538462,-0.446153846153846,
-0.430769230769231,-0.415384615384615,-0.4,-0.384615384615385,-0.369230769230769,
-0.353846153846154,-0.338461538461538,-0.323076923076923,-0.307692307692308,
-0.292307692307692,-0.276923076923077,-0.261538461538462,-0.246153846153846,
-0.230769230769231,-0.215384615384615,-0.2,-0.184615384615385,-0.169230769230769,
-0.153846153846154,-0.138461538461538,-0.123076923076923,-0.107692307692308,
-0.0923076923076923,-0.0769230769230769,-0.0615384615384615,-0.0461538461538462,
-0.0307692307692308,-0.0153846153846154,-0.00577184337452382),
 .UNSPECIFIED.)
CURVE()
GEOMETRIC_REPRESENTATION_ITEM()
RATIONAL_B_SPLINE_CURVE((1.,1.,1.,1.,1.,1.,1.,1.,1.,1.,1.,1.,1.,1.,1.,1.,
1.,1.,1.,1.,1.,1.,1.,1.,1.,1.,1.,1.,1.,1.,1.,1.,1.,1.,1.,1.,1.,1.,1.,1.,
1.,1.,1.,1.,1.,1.,1.,1.,1.,1.,1.,1.,1.,1.,1.,1.,1.,1.,1.,1.,1.,1.,1.,1.,
1.,1.,1.,1.,1.,1.))
REPRESENTATION_ITEM('')
);
#356=(
BOUNDED_CURVE()
B_SPLINE_CURVE(5,(#54473,#54474,#54475,#54476,#54477,#54478,#54479,#54480,
#54481,#54482,#54483,#54484,#54485,#54486,#54487,#54488,#54489,#54490,#54491,
#54492,#54493,#54494,#54495,#54496,#54497,#54498,#54499,#54500,#54501,#54502,
#54503,#54504,#54505,#54506,#54507,#54508,#54509,#54510,#54511,#54512,#54513,
#54514,#54515,#54516,#54517,#54518,#54519,#54520,#54521,#54522,#54523,#54524,
#54525,#54526,#54527,#54528,#54529,#54530,#54531,#54532,#54533,#54534,#54535,
#54536,#54537,#54538,#54539,#54540,#54541,#54542),.UNSPECIFIED.,.F.,.F.)
B_SPLINE_CURVE_WITH_KNOTS((6,1,1,1,1,1,1,1,1,1,1,1,1,1,1,1,1,1,1,1,1,1,
1,1,1,1,1,1,1,1,1,1,1,1,1,1,1,1,1,1,1,1,1,1,1,1,1,1,1,1,1,1,1,1,1,1,1,1,
1,1,1,1,1,1,1,6),(-0.994228156739677,-0.984615384615383,-0.969230769230768,
-0.953846153846152,-0.938461538461537,-0.923076923076922,-0.907692307692306,
-0.892307692307691,-0.876923076923076,-0.86153846153846,-0.846153846153845,
-0.83076923076923,-0.815384615384614,-0.799999999999999,-0.784615384615384,
-0.769230769230768,-0.753846153846153,-0.738461538461538,-0.723076923076922,
-0.707692307692307,-0.692307692307692,-0.676923076923076,-0.661538461538461,
-0.646153846153846,-0.63076923076923,-0.615384615384615,-0.6,-0.584615384615384,
-0.569230769230769,-0.553846153846154,-0.538461538461538,-0.523076923076923,
-0.507692307692308,-0.492307692307692,-0.476923076923077,-0.461538461538462,
-0.446153846153846,-0.430769230769231,-0.415384615384615,-0.4,-0.384615384615385,
-0.369230769230769,-0.353846153846154,-0.338461538461538,-0.323076923076923,
-0.307692307692308,-0.292307692307692,-0.276923076923077,-0.261538461538462,
-0.246153846153846,-0.230769230769231,-0.215384615384615,-0.2,-0.184615384615385,
-0.169230769230769,-0.153846153846154,-0.138461538461538,-0.123076923076923,
-0.107692307692308,-0.0923076923076923,-0.0769230769230769,-0.0615384615384615,
-0.0461538461538462,-0.0307692307692308,-0.0153846153846154,0.),
 .UNSPECIFIED.)
CURVE()
GEOMETRIC_REPRESENTATION_ITEM()
RATIONAL_B_SPLINE_CURVE((1.,1.,1.,1.,1.,1.,1.,1.,1.,1.,1.,1.,1.,1.,1.,1.,
1.,1.,1.,1.,1.,1.,1.,1.,1.,1.,1.,1.,1.,1.,1.,1.,1.,1.,1.,1.,1.,1.,1.,1.,
1.,1.,1.,1.,1.,1.,1.,1.,1.,1.,1.,1.,1.,1.,1.,1.,1.,1.,1.,1.,1.,1.,1.,1.,
1.,1.,1.,1.,1.,1.))
REPRESENTATION_ITEM('')
);
#357=(
BOUNDED_CURVE()
B_SPLINE_CURVE(5,(#54695,#54696,#54697,#54698,#54699,#54700,#54701,#54702,
#54703,#54704,#54705,#54706,#54707,#54708,#54709,#54710,#54711,#54712,#54713,
#54714,#54715,#54716,#54717,#54718,#54719,#54720,#54721,#54722,#54723,#54724,
#54725,#54726,#54727,#54728,#54729,#54730,#54731,#54732,#54733,#54734,#54735,
#54736,#54737,#54738,#54739,#54740,#54741,#54742,#54743,#54744,#54745,#54746,
#54747,#54748,#54749,#54750,#54751,#54752,#54753,#54754,#54755,#54756,#54757,
#54758,#54759,#54760,#54761,#54762,#54763,#54764),.UNSPECIFIED.,.F.,.F.)
B_SPLINE_CURVE_WITH_KNOTS((6,1,1,1,1,1,1,1,1,1,1,1,1,1,1,1,1,1,1,1,1,1,
1,1,1,1,1,1,1,1,1,1,1,1,1,1,1,1,1,1,1,1,1,1,1,1,1,1,1,1,1,1,1,1,1,1,1,1,
1,1,1,1,1,1,1,6),(-1.,-0.984615384615383,-0.969230769230768,-0.953846153846152,
-0.938461538461537,-0.923076923076922,-0.907692307692306,-0.892307692307691,
-0.876923076923076,-0.86153846153846,-0.846153846153845,-0.83076923076923,
-0.815384615384614,-0.799999999999999,-0.784615384615384,-0.769230769230768,
-0.753846153846153,-0.738461538461538,-0.723076923076922,-0.707692307692307,
-0.692307692307692,-0.676923076923076,-0.661538461538461,-0.646153846153846,
-0.63076923076923,-0.615384615384615,-0.6,-0.584615384615384,-0.569230769230769,
-0.553846153846154,-0.538461538461538,-0.523076923076923,-0.507692307692308,
-0.492307692307692,-0.476923076923077,-0.461538461538462,-0.446153846153846,
-0.430769230769231,-0.415384615384615,-0.4,-0.384615384615385,-0.369230769230769,
-0.353846153846154,-0.338461538461538,-0.323076923076923,-0.307692307692308,
-0.292307692307692,-0.276923076923077,-0.261538461538462,-0.246153846153846,
-0.230769230769231,-0.215384615384615,-0.2,-0.184615384615385,-0.169230769230769,
-0.153846153846154,-0.138461538461538,-0.123076923076923,-0.107692307692308,
-0.0923076923076923,-0.0769230769230769,-0.0615384615384615,-0.0461538461538462,
-0.0307692307692308,-0.0153846153846154,-0.0057718433744938),
 .UNSPECIFIED.)
CURVE()
GEOMETRIC_REPRESENTATION_ITEM()
RATIONAL_B_SPLINE_CURVE((1.,1.,1.,1.,1.,1.,1.,1.,1.,1.,1.,1.,1.,1.,1.,1.,
1.,1.,1.,1.,1.,1.,1.,1.,1.,1.,1.,1.,1.,1.,1.,1.,1.,1.,1.,1.,1.,1.,1.,1.,
1.,1.,1.,1.,1.,1.,1.,1.,1.,1.,1.,1.,1.,1.,1.,1.,1.,1.,1.,1.,1.,1.,1.,1.,
1.,1.,1.,1.,1.,1.))
REPRESENTATION_ITEM('')
);
#358=(
BOUNDED_CURVE()
B_SPLINE_CURVE(5,(#54915,#54916,#54917,#54918,#54919,#54920,#54921,#54922,
#54923,#54924,#54925,#54926,#54927,#54928,#54929,#54930,#54931,#54932,#54933,
#54934,#54935,#54936,#54937,#54938,#54939,#54940,#54941,#54942,#54943,#54944,
#54945,#54946,#54947,#54948,#54949,#54950,#54951,#54952,#54953,#54954,#54955,
#54956,#54957,#54958,#54959,#54960,#54961,#54962,#54963,#54964,#54965,#54966,
#54967,#54968,#54969,#54970,#54971,#54972,#54973,#54974,#54975,#54976,#54977,
#54978,#54979,#54980,#54981,#54982,#54983,#54984),.UNSPECIFIED.,.F.,.F.)
B_SPLINE_CURVE_WITH_KNOTS((6,1,1,1,1,1,1,1,1,1,1,1,1,1,1,1,1,1,1,1,1,1,
1,1,1,1,1,1,1,1,1,1,1,1,1,1,1,1,1,1,1,1,1,1,1,1,1,1,1,1,1,1,1,1,1,1,1,1,
1,1,1,1,1,1,1,6),(-0.994228156739743,-0.984615384615383,-0.969230769230768,
-0.953846153846152,-0.938461538461537,-0.923076923076922,-0.907692307692306,
-0.892307692307691,-0.876923076923076,-0.86153846153846,-0.846153846153845,
-0.83076923076923,-0.815384615384614,-0.799999999999999,-0.784615384615384,
-0.769230769230768,-0.753846153846153,-0.738461538461538,-0.723076923076922,
-0.707692307692307,-0.692307692307692,-0.676923076923076,-0.661538461538461,
-0.646153846153846,-0.63076923076923,-0.615384615384615,-0.6,-0.584615384615384,
-0.569230769230769,-0.553846153846154,-0.538461538461538,-0.523076923076923,
-0.507692307692308,-0.492307692307692,-0.476923076923077,-0.461538461538462,
-0.446153846153846,-0.430769230769231,-0.415384615384615,-0.4,-0.384615384615385,
-0.369230769230769,-0.353846153846154,-0.338461538461538,-0.323076923076923,
-0.307692307692308,-0.292307692307692,-0.276923076923077,-0.261538461538462,
-0.246153846153846,-0.230769230769231,-0.215384615384615,-0.2,-0.184615384615385,
-0.169230769230769,-0.153846153846154,-0.138461538461538,-0.123076923076923,
-0.107692307692308,-0.0923076923076923,-0.0769230769230769,-0.0615384615384615,
-0.0461538461538462,-0.0307692307692308,-0.0153846153846154,0.),
 .UNSPECIFIED.)
CURVE()
GEOMETRIC_REPRESENTATION_ITEM()
RATIONAL_B_SPLINE_CURVE((1.,1.,1.,1.,1.,1.,1.,1.,1.,1.,1.,1.,1.,1.,1.,1.,
1.,1.,1.,1.,1.,1.,1.,1.,1.,1.,1.,1.,1.,1.,1.,1.,1.,1.,1.,1.,1.,1.,1.,1.,
1.,1.,1.,1.,1.,1.,1.,1.,1.,1.,1.,1.,1.,1.,1.,1.,1.,1.,1.,1.,1.,1.,1.,1.,
1.,1.,1.,1.,1.,1.))
REPRESENTATION_ITEM('')
);
#359=(
BOUNDED_CURVE()
B_SPLINE_CURVE(5,(#55137,#55138,#55139,#55140,#55141,#55142,#55143,#55144,
#55145,#55146,#55147,#55148,#55149,#55150,#55151,#55152,#55153,#55154,#55155,
#55156,#55157,#55158,#55159,#55160,#55161,#55162,#55163,#55164,#55165,#55166,
#55167,#55168,#55169,#55170,#55171,#55172,#55173,#55174,#55175,#55176,#55177,
#55178,#55179,#55180,#55181,#55182,#55183,#55184,#55185,#55186,#55187,#55188,
#55189,#55190,#55191,#55192,#55193,#55194,#55195,#55196,#55197,#55198,#55199,
#55200,#55201,#55202,#55203,#55204,#55205,#55206),.UNSPECIFIED.,.F.,.F.)
B_SPLINE_CURVE_WITH_KNOTS((6,1,1,1,1,1,1,1,1,1,1,1,1,1,1,1,1,1,1,1,1,1,
1,1,1,1,1,1,1,1,1,1,1,1,1,1,1,1,1,1,1,1,1,1,1,1,1,1,1,1,1,1,1,1,1,1,1,1,
1,1,1,1,1,1,1,6),(-1.,-0.984615384615383,-0.969230769230768,-0.953846153846152,
-0.938461538461537,-0.923076923076922,-0.907692307692306,-0.892307692307691,
-0.876923076923076,-0.86153846153846,-0.846153846153845,-0.83076923076923,
-0.815384615384614,-0.799999999999999,-0.784615384615384,-0.769230769230768,
-0.753846153846153,-0.738461538461538,-0.723076923076922,-0.707692307692307,
-0.692307692307692,-0.676923076923076,-0.661538461538461,-0.646153846153846,
-0.63076923076923,-0.615384615384615,-0.6,-0.584615384615384,-0.569230769230769,
-0.553846153846154,-0.538461538461538,-0.523076923076923,-0.507692307692308,
-0.492307692307692,-0.476923076923077,-0.461538461538462,-0.446153846153846,
-0.430769230769231,-0.415384615384615,-0.4,-0.384615384615385,-0.369230769230769,
-0.353846153846154,-0.338461538461538,-0.323076923076923,-0.307692307692308,
-0.292307692307692,-0.276923076923077,-0.261538461538462,-0.246153846153846,
-0.230769230769231,-0.215384615384615,-0.2,-0.184615384615385,-0.169230769230769,
-0.153846153846154,-0.138461538461538,-0.123076923076923,-0.107692307692308,
-0.0923076923076923,-0.0769230769230769,-0.0615384615384615,-0.0461538461538462,
-0.0307692307692308,-0.0153846153846154,-0.0057718433745291),
 .UNSPECIFIED.)
CURVE()
GEOMETRIC_REPRESENTATION_ITEM()
RATIONAL_B_SPLINE_CURVE((1.,1.,1.,1.,1.,1.,1.,1.,1.,1.,1.,1.,1.,1.,1.,1.,
1.,1.,1.,1.,1.,1.,1.,1.,1.,1.,1.,1.,1.,1.,1.,1.,1.,1.,1.,1.,1.,1.,1.,1.,
1.,1.,1.,1.,1.,1.,1.,1.,1.,1.,1.,1.,1.,1.,1.,1.,1.,1.,1.,1.,1.,1.,1.,1.,
1.,1.,1.,1.,1.,1.))
REPRESENTATION_ITEM('')
);
#360=(
BOUNDED_CURVE()
B_SPLINE_CURVE(5,(#55357,#55358,#55359,#55360,#55361,#55362,#55363,#55364,
#55365,#55366,#55367,#55368,#55369,#55370,#55371,#55372,#55373,#55374,#55375,
#55376,#55377,#55378,#55379,#55380,#55381,#55382,#55383,#55384,#55385,#55386,
#55387,#55388,#55389,#55390,#55391,#55392,#55393,#55394,#55395,#55396,#55397,
#55398,#55399,#55400,#55401,#55402,#55403,#55404,#55405,#55406,#55407,#55408,
#55409,#55410,#55411,#55412,#55413,#55414,#55415,#55416,#55417,#55418,#55419,
#55420,#55421,#55422,#55423,#55424,#55425,#55426),.UNSPECIFIED.,.F.,.F.)
B_SPLINE_CURVE_WITH_KNOTS((6,1,1,1,1,1,1,1,1,1,1,1,1,1,1,1,1,1,1,1,1,1,
1,1,1,1,1,1,1,1,1,1,1,1,1,1,1,1,1,1,1,1,1,1,1,1,1,1,1,1,1,1,1,1,1,1,1,1,
1,1,1,1,1,1,1,6),(-0.994228156739665,-0.984615384615383,-0.969230769230768,
-0.953846153846152,-0.938461538461537,-0.923076923076922,-0.907692307692306,
-0.892307692307691,-0.876923076923076,-0.86153846153846,-0.846153846153845,
-0.83076923076923,-0.815384615384614,-0.799999999999999,-0.784615384615384,
-0.769230769230768,-0.753846153846153,-0.738461538461538,-0.723076923076922,
-0.707692307692307,-0.692307692307692,-0.676923076923076,-0.661538461538461,
-0.646153846153846,-0.63076923076923,-0.615384615384615,-0.6,-0.584615384615384,
-0.569230769230769,-0.553846153846154,-0.538461538461538,-0.523076923076923,
-0.507692307692308,-0.492307692307692,-0.476923076923077,-0.461538461538462,
-0.446153846153846,-0.430769230769231,-0.415384615384615,-0.4,-0.384615384615385,
-0.369230769230769,-0.353846153846154,-0.338461538461538,-0.323076923076923,
-0.307692307692308,-0.292307692307692,-0.276923076923077,-0.261538461538462,
-0.246153846153846,-0.230769230769231,-0.215384615384615,-0.2,-0.184615384615385,
-0.169230769230769,-0.153846153846154,-0.138461538461538,-0.123076923076923,
-0.107692307692308,-0.0923076923076923,-0.0769230769230769,-0.0615384615384615,
-0.0461538461538462,-0.0307692307692308,-0.0153846153846154,0.),
 .UNSPECIFIED.)
CURVE()
GEOMETRIC_REPRESENTATION_ITEM()
RATIONAL_B_SPLINE_CURVE((1.,1.,1.,1.,1.,1.,1.,1.,1.,1.,1.,1.,1.,1.,1.,1.,
1.,1.,1.,1.,1.,1.,1.,1.,1.,1.,1.,1.,1.,1.,1.,1.,1.,1.,1.,1.,1.,1.,1.,1.,
1.,1.,1.,1.,1.,1.,1.,1.,1.,1.,1.,1.,1.,1.,1.,1.,1.,1.,1.,1.,1.,1.,1.,1.,
1.,1.,1.,1.,1.,1.))
REPRESENTATION_ITEM('')
);
#361=(
BOUNDED_CURVE()
B_SPLINE_CURVE(5,(#55579,#55580,#55581,#55582,#55583,#55584,#55585,#55586,
#55587,#55588,#55589,#55590,#55591,#55592,#55593,#55594,#55595,#55596,#55597,
#55598,#55599,#55600,#55601,#55602,#55603,#55604,#55605,#55606,#55607,#55608,
#55609,#55610,#55611,#55612,#55613,#55614,#55615,#55616,#55617,#55618,#55619,
#55620,#55621,#55622,#55623,#55624,#55625,#55626,#55627,#55628,#55629,#55630,
#55631,#55632,#55633,#55634,#55635,#55636,#55637,#55638,#55639,#55640,#55641,
#55642,#55643,#55644,#55645,#55646,#55647,#55648),.UNSPECIFIED.,.F.,.F.)
B_SPLINE_CURVE_WITH_KNOTS((6,1,1,1,1,1,1,1,1,1,1,1,1,1,1,1,1,1,1,1,1,1,
1,1,1,1,1,1,1,1,1,1,1,1,1,1,1,1,1,1,1,1,1,1,1,1,1,1,1,1,1,1,1,1,1,1,1,1,
1,1,1,1,1,1,1,6),(-1.,-0.984615384615383,-0.969230769230768,-0.953846153846152,
-0.938461538461537,-0.923076923076922,-0.907692307692306,-0.892307692307691,
-0.876923076923076,-0.86153846153846,-0.846153846153845,-0.83076923076923,
-0.815384615384614,-0.799999999999999,-0.784615384615384,-0.769230769230768,
-0.753846153846153,-0.738461538461538,-0.723076923076922,-0.707692307692307,
-0.692307692307692,-0.676923076923076,-0.661538461538461,-0.646153846153846,
-0.63076923076923,-0.615384615384615,-0.6,-0.584615384615384,-0.569230769230769,
-0.553846153846154,-0.538461538461538,-0.523076923076923,-0.507692307692308,
-0.492307692307692,-0.476923076923077,-0.461538461538462,-0.446153846153846,
-0.430769230769231,-0.415384615384615,-0.4,-0.384615384615385,-0.369230769230769,
-0.353846153846154,-0.338461538461538,-0.323076923076923,-0.307692307692308,
-0.292307692307692,-0.276923076923077,-0.261538461538462,-0.246153846153846,
-0.230769230769231,-0.215384615384615,-0.2,-0.184615384615385,-0.169230769230769,
-0.153846153846154,-0.138461538461538,-0.123076923076923,-0.107692307692308,
-0.0923076923076923,-0.0769230769230769,-0.0615384615384615,-0.0461538461538462,
-0.0307692307692308,-0.0153846153846154,-0.00577184337450666),
 .UNSPECIFIED.)
CURVE()
GEOMETRIC_REPRESENTATION_ITEM()
RATIONAL_B_SPLINE_CURVE((1.,1.,1.,1.,1.,1.,1.,1.,1.,1.,1.,1.,1.,1.,1.,1.,
1.,1.,1.,1.,1.,1.,1.,1.,1.,1.,1.,1.,1.,1.,1.,1.,1.,1.,1.,1.,1.,1.,1.,1.,
1.,1.,1.,1.,1.,1.,1.,1.,1.,1.,1.,1.,1.,1.,1.,1.,1.,1.,1.,1.,1.,1.,1.,1.,
1.,1.,1.,1.,1.,1.))
REPRESENTATION_ITEM('')
);
#362=(
BOUNDED_CURVE()
B_SPLINE_CURVE(5,(#55799,#55800,#55801,#55802,#55803,#55804,#55805,#55806,
#55807,#55808,#55809,#55810,#55811,#55812,#55813,#55814,#55815,#55816,#55817,
#55818,#55819,#55820,#55821,#55822,#55823,#55824,#55825,#55826,#55827,#55828,
#55829,#55830,#55831,#55832,#55833,#55834,#55835,#55836,#55837,#55838,#55839,
#55840,#55841,#55842,#55843,#55844,#55845,#55846,#55847,#55848,#55849,#55850,
#55851,#55852,#55853,#55854,#55855,#55856,#55857,#55858,#55859,#55860,#55861,
#55862,#55863,#55864,#55865,#55866,#55867,#55868),.UNSPECIFIED.,.F.,.F.)
B_SPLINE_CURVE_WITH_KNOTS((6,1,1,1,1,1,1,1,1,1,1,1,1,1,1,1,1,1,1,1,1,1,
1,1,1,1,1,1,1,1,1,1,1,1,1,1,1,1,1,1,1,1,1,1,1,1,1,1,1,1,1,1,1,1,1,1,1,1,
1,1,1,1,1,1,1,6),(-0.994228156739758,-0.984615384615383,-0.969230769230768,
-0.953846153846152,-0.938461538461537,-0.923076923076922,-0.907692307692306,
-0.892307692307691,-0.876923076923076,-0.86153846153846,-0.846153846153845,
-0.83076923076923,-0.815384615384614,-0.799999999999999,-0.784615384615384,
-0.769230769230768,-0.753846153846153,-0.738461538461538,-0.723076923076922,
-0.707692307692307,-0.692307692307692,-0.676923076923076,-0.661538461538461,
-0.646153846153846,-0.63076923076923,-0.615384615384615,-0.6,-0.584615384615384,
-0.569230769230769,-0.553846153846154,-0.538461538461538,-0.523076923076923,
-0.507692307692308,-0.492307692307692,-0.476923076923077,-0.461538461538462,
-0.446153846153846,-0.430769230769231,-0.415384615384615,-0.4,-0.384615384615385,
-0.369230769230769,-0.353846153846154,-0.338461538461538,-0.323076923076923,
-0.307692307692308,-0.292307692307692,-0.276923076923077,-0.261538461538462,
-0.246153846153846,-0.230769230769231,-0.215384615384615,-0.2,-0.184615384615385,
-0.169230769230769,-0.153846153846154,-0.138461538461538,-0.123076923076923,
-0.107692307692308,-0.0923076923076923,-0.0769230769230769,-0.0615384615384615,
-0.0461538461538462,-0.0307692307692308,-0.0153846153846154,0.),
 .UNSPECIFIED.)
CURVE()
GEOMETRIC_REPRESENTATION_ITEM()
RATIONAL_B_SPLINE_CURVE((1.,1.,1.,1.,1.,1.,1.,1.,1.,1.,1.,1.,1.,1.,1.,1.,
1.,1.,1.,1.,1.,1.,1.,1.,1.,1.,1.,1.,1.,1.,1.,1.,1.,1.,1.,1.,1.,1.,1.,1.,
1.,1.,1.,1.,1.,1.,1.,1.,1.,1.,1.,1.,1.,1.,1.,1.,1.,1.,1.,1.,1.,1.,1.,1.,
1.,1.,1.,1.,1.,1.))
REPRESENTATION_ITEM('')
);
#363=(
BOUNDED_CURVE()
B_SPLINE_CURVE(5,(#56021,#56022,#56023,#56024,#56025,#56026,#56027,#56028,
#56029,#56030,#56031,#56032,#56033,#56034,#56035,#56036,#56037,#56038,#56039,
#56040,#56041,#56042,#56043,#56044,#56045,#56046,#56047,#56048,#56049,#56050,
#56051,#56052,#56053,#56054,#56055,#56056,#56057,#56058,#56059,#56060,#56061,
#56062,#56063,#56064,#56065,#56066,#56067,#56068,#56069,#56070,#56071,#56072,
#56073,#56074,#56075,#56076,#56077,#56078,#56079,#56080,#56081,#56082,#56083,
#56084,#56085,#56086,#56087,#56088,#56089,#56090),.UNSPECIFIED.,.F.,.F.)
B_SPLINE_CURVE_WITH_KNOTS((6,1,1,1,1,1,1,1,1,1,1,1,1,1,1,1,1,1,1,1,1,1,
1,1,1,1,1,1,1,1,1,1,1,1,1,1,1,1,1,1,1,1,1,1,1,1,1,1,1,1,1,1,1,1,1,1,1,1,
1,1,1,1,1,1,1,6),(-1.,-0.984615384615383,-0.969230769230768,-0.953846153846152,
-0.938461538461537,-0.923076923076922,-0.907692307692306,-0.892307692307691,
-0.876923076923076,-0.86153846153846,-0.846153846153845,-0.83076923076923,
-0.815384615384614,-0.799999999999999,-0.784615384615384,-0.769230769230768,
-0.753846153846153,-0.738461538461538,-0.723076923076922,-0.707692307692307,
-0.692307692307692,-0.676923076923076,-0.661538461538461,-0.646153846153846,
-0.63076923076923,-0.615384615384615,-0.6,-0.584615384615384,-0.569230769230769,
-0.553846153846154,-0.538461538461538,-0.523076923076923,-0.507692307692308,
-0.492307692307692,-0.476923076923077,-0.461538461538462,-0.446153846153846,
-0.430769230769231,-0.415384615384615,-0.4,-0.384615384615385,-0.369230769230769,
-0.353846153846154,-0.338461538461538,-0.323076923076923,-0.307692307692308,
-0.292307692307692,-0.276923076923077,-0.261538461538462,-0.246153846153846,
-0.230769230769231,-0.215384615384615,-0.2,-0.184615384615385,-0.169230769230769,
-0.153846153846154,-0.138461538461538,-0.123076923076923,-0.107692307692308,
-0.0923076923076923,-0.0769230769230769,-0.0615384615384615,-0.0461538461538462,
-0.0307692307692308,-0.0153846153846154,-0.00577184337451981),
 .UNSPECIFIED.)
CURVE()
GEOMETRIC_REPRESENTATION_ITEM()
RATIONAL_B_SPLINE_CURVE((1.,1.,1.,1.,1.,1.,1.,1.,1.,1.,1.,1.,1.,1.,1.,1.,
1.,1.,1.,1.,1.,1.,1.,1.,1.,1.,1.,1.,1.,1.,1.,1.,1.,1.,1.,1.,1.,1.,1.,1.,
1.,1.,1.,1.,1.,1.,1.,1.,1.,1.,1.,1.,1.,1.,1.,1.,1.,1.,1.,1.,1.,1.,1.,1.,
1.,1.,1.,1.,1.,1.))
REPRESENTATION_ITEM('')
);
#364=(
BOUNDED_CURVE()
B_SPLINE_CURVE(5,(#56241,#56242,#56243,#56244,#56245,#56246,#56247,#56248,
#56249,#56250,#56251,#56252,#56253,#56254,#56255,#56256,#56257,#56258,#56259,
#56260,#56261,#56262,#56263,#56264,#56265,#56266,#56267,#56268,#56269,#56270,
#56271,#56272,#56273,#56274,#56275,#56276,#56277,#56278,#56279,#56280,#56281,
#56282,#56283,#56284,#56285,#56286,#56287,#56288,#56289,#56290,#56291,#56292,
#56293,#56294,#56295,#56296,#56297,#56298,#56299,#56300,#56301,#56302,#56303,
#56304,#56305,#56306,#56307,#56308,#56309,#56310),.UNSPECIFIED.,.F.,.F.)
B_SPLINE_CURVE_WITH_KNOTS((6,1,1,1,1,1,1,1,1,1,1,1,1,1,1,1,1,1,1,1,1,1,
1,1,1,1,1,1,1,1,1,1,1,1,1,1,1,1,1,1,1,1,1,1,1,1,1,1,1,1,1,1,1,1,1,1,1,1,
1,1,1,1,1,1,1,6),(-0.994228156739659,-0.984615384615383,-0.969230769230768,
-0.953846153846152,-0.938461538461537,-0.923076923076922,-0.907692307692306,
-0.892307692307691,-0.876923076923076,-0.86153846153846,-0.846153846153845,
-0.83076923076923,-0.815384615384614,-0.799999999999999,-0.784615384615384,
-0.769230769230768,-0.753846153846153,-0.738461538461538,-0.723076923076922,
-0.707692307692307,-0.692307692307692,-0.676923076923076,-0.661538461538461,
-0.646153846153846,-0.63076923076923,-0.615384615384615,-0.6,-0.584615384615384,
-0.569230769230769,-0.553846153846154,-0.538461538461538,-0.523076923076923,
-0.507692307692308,-0.492307692307692,-0.476923076923077,-0.461538461538462,
-0.446153846153846,-0.430769230769231,-0.415384615384615,-0.4,-0.384615384615385,
-0.369230769230769,-0.353846153846154,-0.338461538461538,-0.323076923076923,
-0.307692307692308,-0.292307692307692,-0.276923076923077,-0.261538461538462,
-0.246153846153846,-0.230769230769231,-0.215384615384615,-0.2,-0.184615384615385,
-0.169230769230769,-0.153846153846154,-0.138461538461538,-0.123076923076923,
-0.107692307692308,-0.0923076923076923,-0.0769230769230769,-0.0615384615384615,
-0.0461538461538462,-0.0307692307692308,-0.0153846153846154,0.),
 .UNSPECIFIED.)
CURVE()
GEOMETRIC_REPRESENTATION_ITEM()
RATIONAL_B_SPLINE_CURVE((1.,1.,1.,1.,1.,1.,1.,1.,1.,1.,1.,1.,1.,1.,1.,1.,
1.,1.,1.,1.,1.,1.,1.,1.,1.,1.,1.,1.,1.,1.,1.,1.,1.,1.,1.,1.,1.,1.,1.,1.,
1.,1.,1.,1.,1.,1.,1.,1.,1.,1.,1.,1.,1.,1.,1.,1.,1.,1.,1.,1.,1.,1.,1.,1.,
1.,1.,1.,1.,1.,1.))
REPRESENTATION_ITEM('')
);
#365=(
BOUNDED_CURVE()
B_SPLINE_CURVE(5,(#56463,#56464,#56465,#56466,#56467,#56468,#56469,#56470,
#56471,#56472,#56473,#56474,#56475,#56476,#56477,#56478,#56479,#56480,#56481,
#56482,#56483,#56484,#56485,#56486,#56487,#56488,#56489,#56490,#56491,#56492,
#56493,#56494,#56495,#56496,#56497,#56498,#56499,#56500,#56501,#56502,#56503,
#56504,#56505,#56506,#56507,#56508,#56509,#56510,#56511,#56512,#56513,#56514,
#56515,#56516,#56517,#56518,#56519,#56520,#56521,#56522,#56523,#56524,#56525,
#56526,#56527,#56528,#56529,#56530,#56531,#56532),.UNSPECIFIED.,.F.,.F.)
B_SPLINE_CURVE_WITH_KNOTS((6,1,1,1,1,1,1,1,1,1,1,1,1,1,1,1,1,1,1,1,1,1,
1,1,1,1,1,1,1,1,1,1,1,1,1,1,1,1,1,1,1,1,1,1,1,1,1,1,1,1,1,1,1,1,1,1,1,1,
1,1,1,1,1,1,1,6),(-1.,-0.984615384615383,-0.969230769230768,-0.953846153846152,
-0.938461538461537,-0.923076923076922,-0.907692307692306,-0.892307692307691,
-0.876923076923076,-0.86153846153846,-0.846153846153845,-0.83076923076923,
-0.815384615384614,-0.799999999999999,-0.784615384615384,-0.769230769230768,
-0.753846153846153,-0.738461538461538,-0.723076923076922,-0.707692307692307,
-0.692307692307692,-0.676923076923076,-0.661538461538461,-0.646153846153846,
-0.63076923076923,-0.615384615384615,-0.6,-0.584615384615384,-0.569230769230769,
-0.553846153846154,-0.538461538461538,-0.523076923076923,-0.507692307692308,
-0.492307692307692,-0.476923076923077,-0.461538461538462,-0.446153846153846,
-0.430769230769231,-0.415384615384615,-0.4,-0.384615384615385,-0.369230769230769,
-0.353846153846154,-0.338461538461538,-0.323076923076923,-0.307692307692308,
-0.292307692307692,-0.276923076923077,-0.261538461538462,-0.246153846153846,
-0.230769230769231,-0.215384615384615,-0.2,-0.184615384615385,-0.169230769230769,
-0.153846153846154,-0.138461538461538,-0.123076923076923,-0.107692307692308,
-0.0923076923076923,-0.0769230769230769,-0.0615384615384615,-0.0461538461538462,
-0.0307692307692308,-0.0153846153846154,-0.00577184337450306),
 .UNSPECIFIED.)
CURVE()
GEOMETRIC_REPRESENTATION_ITEM()
RATIONAL_B_SPLINE_CURVE((1.,1.,1.,1.,1.,1.,1.,1.,1.,1.,1.,1.,1.,1.,1.,1.,
1.,1.,1.,1.,1.,1.,1.,1.,1.,1.,1.,1.,1.,1.,1.,1.,1.,1.,1.,1.,1.,1.,1.,1.,
1.,1.,1.,1.,1.,1.,1.,1.,1.,1.,1.,1.,1.,1.,1.,1.,1.,1.,1.,1.,1.,1.,1.,1.,
1.,1.,1.,1.,1.,1.))
REPRESENTATION_ITEM('')
);
#366=(
BOUNDED_CURVE()
B_SPLINE_CURVE(5,(#56683,#56684,#56685,#56686,#56687,#56688,#56689,#56690,
#56691,#56692,#56693,#56694,#56695,#56696,#56697,#56698,#56699,#56700,#56701,
#56702,#56703,#56704,#56705,#56706,#56707,#56708,#56709,#56710,#56711,#56712,
#56713,#56714,#56715,#56716,#56717,#56718,#56719,#56720,#56721,#56722,#56723,
#56724,#56725,#56726,#56727,#56728,#56729,#56730,#56731,#56732,#56733,#56734,
#56735,#56736,#56737,#56738,#56739,#56740,#56741,#56742,#56743,#56744,#56745,
#56746,#56747,#56748,#56749,#56750,#56751,#56752),.UNSPECIFIED.,.F.,.F.)
B_SPLINE_CURVE_WITH_KNOTS((6,1,1,1,1,1,1,1,1,1,1,1,1,1,1,1,1,1,1,1,1,1,
1,1,1,1,1,1,1,1,1,1,1,1,1,1,1,1,1,1,1,1,1,1,1,1,1,1,1,1,1,1,1,1,1,1,1,1,
1,1,1,1,1,1,1,6),(-0.994228156739675,-0.984615384615383,-0.969230769230768,
-0.953846153846152,-0.938461538461537,-0.923076923076922,-0.907692307692306,
-0.892307692307691,-0.876923076923076,-0.86153846153846,-0.846153846153845,
-0.83076923076923,-0.815384615384614,-0.799999999999999,-0.784615384615384,
-0.769230769230768,-0.753846153846153,-0.738461538461538,-0.723076923076922,
-0.707692307692307,-0.692307692307692,-0.676923076923076,-0.661538461538461,
-0.646153846153846,-0.63076923076923,-0.615384615384615,-0.6,-0.584615384615384,
-0.569230769230769,-0.553846153846154,-0.538461538461538,-0.523076923076923,
-0.507692307692308,-0.492307692307692,-0.476923076923077,-0.461538461538462,
-0.446153846153846,-0.430769230769231,-0.415384615384615,-0.4,-0.384615384615385,
-0.369230769230769,-0.353846153846154,-0.338461538461538,-0.323076923076923,
-0.307692307692308,-0.292307692307692,-0.276923076923077,-0.261538461538462,
-0.246153846153846,-0.230769230769231,-0.215384615384615,-0.2,-0.184615384615385,
-0.169230769230769,-0.153846153846154,-0.138461538461538,-0.123076923076923,
-0.107692307692308,-0.0923076923076923,-0.0769230769230769,-0.0615384615384615,
-0.0461538461538462,-0.0307692307692308,-0.0153846153846154,0.),
 .UNSPECIFIED.)
CURVE()
GEOMETRIC_REPRESENTATION_ITEM()
RATIONAL_B_SPLINE_CURVE((1.,1.,1.,1.,1.,1.,1.,1.,1.,1.,1.,1.,1.,1.,1.,1.,
1.,1.,1.,1.,1.,1.,1.,1.,1.,1.,1.,1.,1.,1.,1.,1.,1.,1.,1.,1.,1.,1.,1.,1.,
1.,1.,1.,1.,1.,1.,1.,1.,1.,1.,1.,1.,1.,1.,1.,1.,1.,1.,1.,1.,1.,1.,1.,1.,
1.,1.,1.,1.,1.,1.))
REPRESENTATION_ITEM('')
);
#367=(
BOUNDED_CURVE()
B_SPLINE_CURVE(5,(#56905,#56906,#56907,#56908,#56909,#56910,#56911,#56912,
#56913,#56914,#56915,#56916,#56917,#56918,#56919,#56920,#56921,#56922,#56923,
#56924,#56925,#56926,#56927,#56928,#56929,#56930,#56931,#56932,#56933,#56934,
#56935,#56936,#56937,#56938,#56939,#56940,#56941,#56942,#56943,#56944,#56945,
#56946,#56947,#56948,#56949,#56950,#56951,#56952,#56953,#56954,#56955,#56956,
#56957,#56958,#56959,#56960,#56961,#56962,#56963,#56964,#56965,#56966,#56967,
#56968,#56969,#56970,#56971,#56972,#56973,#56974),.UNSPECIFIED.,.F.,.F.)
B_SPLINE_CURVE_WITH_KNOTS((6,1,1,1,1,1,1,1,1,1,1,1,1,1,1,1,1,1,1,1,1,1,
1,1,1,1,1,1,1,1,1,1,1,1,1,1,1,1,1,1,1,1,1,1,1,1,1,1,1,1,1,1,1,1,1,1,1,1,
1,1,1,1,1,1,1,6),(-1.,-0.984615384615383,-0.969230769230768,-0.953846153846152,
-0.938461538461537,-0.923076923076922,-0.907692307692306,-0.892307692307691,
-0.876923076923076,-0.86153846153846,-0.846153846153845,-0.83076923076923,
-0.815384615384614,-0.799999999999999,-0.784615384615384,-0.769230769230768,
-0.753846153846153,-0.738461538461538,-0.723076923076922,-0.707692307692307,
-0.692307692307692,-0.676923076923076,-0.661538461538461,-0.646153846153846,
-0.63076923076923,-0.615384615384615,-0.6,-0.584615384615384,-0.569230769230769,
-0.553846153846154,-0.538461538461538,-0.523076923076923,-0.507692307692308,
-0.492307692307692,-0.476923076923077,-0.461538461538462,-0.446153846153846,
-0.430769230769231,-0.415384615384615,-0.4,-0.384615384615385,-0.369230769230769,
-0.353846153846154,-0.338461538461538,-0.323076923076923,-0.307692307692308,
-0.292307692307692,-0.276923076923077,-0.261538461538462,-0.246153846153846,
-0.230769230769231,-0.215384615384615,-0.2,-0.184615384615385,-0.169230769230769,
-0.153846153846154,-0.138461538461538,-0.123076923076923,-0.107692307692308,
-0.0923076923076923,-0.0769230769230769,-0.0615384615384615,-0.0461538461538462,
-0.0307692307692308,-0.0153846153846154,-0.00577184337450328),
 .UNSPECIFIED.)
CURVE()
GEOMETRIC_REPRESENTATION_ITEM()
RATIONAL_B_SPLINE_CURVE((1.,1.,1.,1.,1.,1.,1.,1.,1.,1.,1.,1.,1.,1.,1.,1.,
1.,1.,1.,1.,1.,1.,1.,1.,1.,1.,1.,1.,1.,1.,1.,1.,1.,1.,1.,1.,1.,1.,1.,1.,
1.,1.,1.,1.,1.,1.,1.,1.,1.,1.,1.,1.,1.,1.,1.,1.,1.,1.,1.,1.,1.,1.,1.,1.,
1.,1.,1.,1.,1.,1.))
REPRESENTATION_ITEM('')
);
#368=(
BOUNDED_CURVE()
B_SPLINE_CURVE(5,(#57127,#57128,#57129,#57130,#57131,#57132,#57133,#57134,
#57135,#57136,#57137,#57138,#57139,#57140,#57141,#57142,#57143,#57144,#57145,
#57146,#57147,#57148,#57149,#57150,#57151,#57152,#57153,#57154,#57155,#57156,
#57157,#57158,#57159,#57160,#57161,#57162,#57163,#57164,#57165,#57166,#57167,
#57168,#57169,#57170,#57171,#57172,#57173,#57174,#57175,#57176,#57177,#57178,
#57179,#57180,#57181,#57182,#57183,#57184,#57185,#57186,#57187,#57188,#57189,
#57190,#57191,#57192,#57193,#57194,#57195,#57196),.UNSPECIFIED.,.F.,.F.)
B_SPLINE_CURVE_WITH_KNOTS((6,1,1,1,1,1,1,1,1,1,1,1,1,1,1,1,1,1,1,1,1,1,
1,1,1,1,1,1,1,1,1,1,1,1,1,1,1,1,1,1,1,1,1,1,1,1,1,1,1,1,1,1,1,1,1,1,1,1,
1,1,1,1,1,1,1,6),(-0.994228156739672,-0.984615384615383,-0.969230769230768,
-0.953846153846152,-0.938461538461537,-0.923076923076922,-0.907692307692306,
-0.892307692307691,-0.876923076923076,-0.86153846153846,-0.846153846153845,
-0.83076923076923,-0.815384615384614,-0.799999999999999,-0.784615384615384,
-0.769230769230768,-0.753846153846153,-0.738461538461538,-0.723076923076922,
-0.707692307692307,-0.692307692307692,-0.676923076923076,-0.661538461538461,
-0.646153846153846,-0.63076923076923,-0.615384615384615,-0.6,-0.584615384615384,
-0.569230769230769,-0.553846153846154,-0.538461538461538,-0.523076923076923,
-0.507692307692308,-0.492307692307692,-0.476923076923077,-0.461538461538462,
-0.446153846153846,-0.430769230769231,-0.415384615384615,-0.4,-0.384615384615385,
-0.369230769230769,-0.353846153846154,-0.338461538461538,-0.323076923076923,
-0.307692307692308,-0.292307692307692,-0.276923076923077,-0.261538461538462,
-0.246153846153846,-0.230769230769231,-0.215384615384615,-0.2,-0.184615384615385,
-0.169230769230769,-0.153846153846154,-0.138461538461538,-0.123076923076923,
-0.107692307692308,-0.0923076923076923,-0.0769230769230769,-0.0615384615384615,
-0.0461538461538462,-0.0307692307692308,-0.0153846153846154,0.),
 .UNSPECIFIED.)
CURVE()
GEOMETRIC_REPRESENTATION_ITEM()
RATIONAL_B_SPLINE_CURVE((1.,1.,1.,1.,1.,1.,1.,1.,1.,1.,1.,1.,1.,1.,1.,1.,
1.,1.,1.,1.,1.,1.,1.,1.,1.,1.,1.,1.,1.,1.,1.,1.,1.,1.,1.,1.,1.,1.,1.,1.,
1.,1.,1.,1.,1.,1.,1.,1.,1.,1.,1.,1.,1.,1.,1.,1.,1.,1.,1.,1.,1.,1.,1.,1.,
1.,1.,1.,1.,1.,1.))
REPRESENTATION_ITEM('')
);
#369=(
BOUNDED_CURVE()
B_SPLINE_CURVE(5,(#57355,#57356,#57357,#57358,#57359,#57360,#57361,#57362,
#57363,#57364,#57365,#57366,#57367,#57368,#57369,#57370,#57371,#57372,#57373,
#57374,#57375,#57376,#57377,#57378,#57379,#57380,#57381,#57382,#57383,#57384,
#57385,#57386,#57387,#57388,#57389,#57390,#57391,#57392,#57393,#57394,#57395,
#57396,#57397,#57398,#57399,#57400,#57401,#57402,#57403,#57404,#57405,#57406,
#57407,#57408,#57409,#57410,#57411,#57412,#57413,#57414,#57415,#57416,#57417,
#57418,#57419,#57420,#57421,#57422,#57423,#57424),.UNSPECIFIED.,.F.,.F.)
B_SPLINE_CURVE_WITH_KNOTS((6,1,1,1,1,1,1,1,1,1,1,1,1,1,1,1,1,1,1,1,1,1,
1,1,1,1,1,1,1,1,1,1,1,1,1,1,1,1,1,1,1,1,1,1,1,1,1,1,1,1,1,1,1,1,1,1,1,1,
1,1,1,1,1,1,1,6),(-0.994228156739704,-0.984615384615383,-0.969230769230768,
-0.953846153846152,-0.938461538461537,-0.923076923076922,-0.907692307692306,
-0.892307692307691,-0.876923076923076,-0.86153846153846,-0.846153846153845,
-0.83076923076923,-0.815384615384614,-0.799999999999999,-0.784615384615384,
-0.769230769230768,-0.753846153846153,-0.738461538461538,-0.723076923076922,
-0.707692307692307,-0.692307692307692,-0.676923076923076,-0.661538461538461,
-0.646153846153846,-0.63076923076923,-0.615384615384615,-0.6,-0.584615384615384,
-0.569230769230769,-0.553846153846154,-0.538461538461538,-0.523076923076923,
-0.507692307692308,-0.492307692307692,-0.476923076923077,-0.461538461538462,
-0.446153846153846,-0.430769230769231,-0.415384615384615,-0.4,-0.384615384615385,
-0.369230769230769,-0.353846153846154,-0.338461538461538,-0.323076923076923,
-0.307692307692308,-0.292307692307692,-0.276923076923077,-0.261538461538462,
-0.246153846153846,-0.230769230769231,-0.215384615384615,-0.2,-0.184615384615385,
-0.169230769230769,-0.153846153846154,-0.138461538461538,-0.123076923076923,
-0.107692307692308,-0.0923076923076923,-0.0769230769230769,-0.0615384615384615,
-0.0461538461538462,-0.0307692307692308,-0.0153846153846154,0.),
 .UNSPECIFIED.)
CURVE()
GEOMETRIC_REPRESENTATION_ITEM()
RATIONAL_B_SPLINE_CURVE((1.,1.,1.,1.,1.,1.,1.,1.,1.,1.,1.,1.,1.,1.,1.,1.,
1.,1.,1.,1.,1.,1.,1.,1.,1.,1.,1.,1.,1.,1.,1.,1.,1.,1.,1.,1.,1.,1.,1.,1.,
1.,1.,1.,1.,1.,1.,1.,1.,1.,1.,1.,1.,1.,1.,1.,1.,1.,1.,1.,1.,1.,1.,1.,1.,
1.,1.,1.,1.,1.,1.))
REPRESENTATION_ITEM('')
);
#370=(
BOUNDED_CURVE()
B_SPLINE_CURVE(5,(#57566,#57567,#57568,#57569,#57570,#57571,#57572,#57573,
#57574,#57575,#57576,#57577,#57578,#57579,#57580,#57581,#57582,#57583,#57584,
#57585,#57586,#57587,#57588,#57589,#57590,#57591,#57592,#57593,#57594,#57595,
#57596,#57597,#57598,#57599,#57600,#57601,#57602,#57603,#57604,#57605,#57606,
#57607,#57608,#57609,#57610,#57611,#57612,#57613,#57614,#57615,#57616,#57617,
#57618,#57619,#57620,#57621,#57622,#57623,#57624,#57625,#57626,#57627,#57628,
#57629,#57630,#57631,#57632,#57633,#57634,#57635),.UNSPECIFIED.,.F.,.F.)
B_SPLINE_CURVE_WITH_KNOTS((6,1,1,1,1,1,1,1,1,1,1,1,1,1,1,1,1,1,1,1,1,1,
1,1,1,1,1,1,1,1,1,1,1,1,1,1,1,1,1,1,1,1,1,1,1,1,1,1,1,1,1,1,1,1,1,1,1,1,
1,1,1,1,1,1,1,6),(-1.,-0.984615384615383,-0.969230769230768,-0.953846153846152,
-0.938461538461537,-0.923076923076922,-0.907692307692306,-0.892307692307691,
-0.876923076923076,-0.86153846153846,-0.846153846153845,-0.83076923076923,
-0.815384615384614,-0.799999999999999,-0.784615384615384,-0.769230769230768,
-0.753846153846153,-0.738461538461538,-0.723076923076922,-0.707692307692307,
-0.692307692307692,-0.676923076923076,-0.661538461538461,-0.646153846153846,
-0.63076923076923,-0.615384615384615,-0.6,-0.584615384615384,-0.569230769230769,
-0.553846153846154,-0.538461538461538,-0.523076923076923,-0.507692307692308,
-0.492307692307692,-0.476923076923077,-0.461538461538462,-0.446153846153846,
-0.430769230769231,-0.415384615384615,-0.4,-0.384615384615385,-0.369230769230769,
-0.353846153846154,-0.338461538461538,-0.323076923076923,-0.307692307692308,
-0.292307692307692,-0.276923076923077,-0.261538461538462,-0.246153846153846,
-0.230769230769231,-0.215384615384615,-0.2,-0.184615384615385,-0.169230769230769,
-0.153846153846154,-0.138461538461538,-0.123076923076923,-0.107692307692308,
-0.0923076923076923,-0.0769230769230769,-0.0615384615384615,-0.0461538461538462,
-0.0307692307692308,-0.0153846153846154,-0.00577184337451611),
 .UNSPECIFIED.)
CURVE()
GEOMETRIC_REPRESENTATION_ITEM()
RATIONAL_B_SPLINE_CURVE((1.,1.,1.,1.,1.,1.,1.,1.,1.,1.,1.,1.,1.,1.,1.,1.,
1.,1.,1.,1.,1.,1.,1.,1.,1.,1.,1.,1.,1.,1.,1.,1.,1.,1.,1.,1.,1.,1.,1.,1.,
1.,1.,1.,1.,1.,1.,1.,1.,1.,1.,1.,1.,1.,1.,1.,1.,1.,1.,1.,1.,1.,1.,1.,1.,
1.,1.,1.,1.,1.,1.))
REPRESENTATION_ITEM('')
);
#371=ORIENTED_CLOSED_SHELL('',*,#13601,.F.);
#372=ORIENTED_CLOSED_SHELL('',*,#13611,.F.);
#373=ORIENTED_CLOSED_SHELL('',*,#13642,.F.);
#374=BREP_WITH_VOIDS('Body1',#13600,(#371));
#375=BREP_WITH_VOIDS('Body1',#13612,(#372));
#376=BREP_WITH_VOIDS('Body1',#13643,(#373));
#377=ITEM_DEFINED_TRANSFORMATION($,$,#14497,#14619);
#378=ITEM_DEFINED_TRANSFORMATION($,$,#14517,#14620);
#379=ITEM_DEFINED_TRANSFORMATION($,$,#14537,#14621);
#380=ITEM_DEFINED_TRANSFORMATION($,$,#14552,#14622);
#381=ITEM_DEFINED_TRANSFORMATION($,$,#14602,#14623);
#382=ITEM_DEFINED_TRANSFORMATION($,$,#14802,#14863);
#383=ITEM_DEFINED_TRANSFORMATION($,$,#14841,#14864);
#384=ITEM_DEFINED_TRANSFORMATION($,$,#14852,#14865);
#385=ITEM_DEFINED_TRANSFORMATION($,$,#14908,#15036);
#386=ITEM_DEFINED_TRANSFORMATION($,$,#14928,#15037);
#387=ITEM_DEFINED_TRANSFORMATION($,$,#14948,#15038);
#388=ITEM_DEFINED_TRANSFORMATION($,$,#14965,#15039);
#389=ITEM_DEFINED_TRANSFORMATION($,$,#15019,#15040);
#390=ITEM_DEFINED_TRANSFORMATION($,$,#14197,#15503);
#391=ITEM_DEFINED_TRANSFORMATION($,$,#14240,#15504);
#392=ITEM_DEFINED_TRANSFORMATION($,$,#14247,#15505);
#393=ITEM_DEFINED_TRANSFORMATION($,$,#14254,#15506);
#394=ITEM_DEFINED_TRANSFORMATION($,$,#14324,#15507);
#395=ITEM_DEFINED_TRANSFORMATION($,$,#14333,#15508);
#396=ITEM_DEFINED_TRANSFORMATION($,$,#14367,#15509);
#397=ITEM_DEFINED_TRANSFORMATION($,$,#14389,#15510);
#398=ITEM_DEFINED_TRANSFORMATION($,$,#14432,#15511);
#399=ITEM_DEFINED_TRANSFORMATION($,$,#14441,#15512);
#400=ITEM_DEFINED_TRANSFORMATION($,$,#14447,#15513);
#401=ITEM_DEFINED_TRANSFORMATION($,$,#14453,#15514);
#402=ITEM_DEFINED_TRANSFORMATION($,$,#14624,#15515);
#403=ITEM_DEFINED_TRANSFORMATION($,$,#14624,#15516);
#404=ITEM_DEFINED_TRANSFORMATION($,$,#14624,#15517);
#405=ITEM_DEFINED_TRANSFORMATION($,$,#14624,#15518);
#406=ITEM_DEFINED_TRANSFORMATION($,$,#14883,#15519);
#407=ITEM_DEFINED_TRANSFORMATION($,$,#14883,#15520);
#408=ITEM_DEFINED_TRANSFORMATION($,$,#14883,#15521);
#409=ITEM_DEFINED_TRANSFORMATION($,$,#14883,#15522);
#410=ITEM_DEFINED_TRANSFORMATION($,$,#14496,#15523);
#411=ITEM_DEFINED_TRANSFORMATION($,$,#14496,#15524);
#412=ITEM_DEFINED_TRANSFORMATION($,$,#15479,#15525);
#413=ITEM_DEFINED_TRANSFORMATION($,$,#15479,#15526);
#414=ITEM_DEFINED_TRANSFORMATION($,$,#15479,#15527);
#415=ITEM_DEFINED_TRANSFORMATION($,$,#15479,#15528);
#416=ITEM_DEFINED_TRANSFORMATION($,$,#14624,#15529);
#417=ITEM_DEFINED_TRANSFORMATION($,$,#14624,#15530);
#418=ITEM_DEFINED_TRANSFORMATION($,$,#14624,#15531);
#419=ITEM_DEFINED_TRANSFORMATION($,$,#14624,#15532);
#420=ITEM_DEFINED_TRANSFORMATION($,$,#14866,#15533);
#421=ITEM_DEFINED_TRANSFORMATION($,$,#14651,#15534);
#422=ITEM_DEFINED_TRANSFORMATION($,$,#14694,#15535);
#423=ITEM_DEFINED_TRANSFORMATION($,$,#14701,#15536);
#424=ITEM_DEFINED_TRANSFORMATION($,$,#14771,#15537);
#425=ITEM_DEFINED_TRANSFORMATION($,$,#14780,#15538);
#426=ITEM_DEFINED_TRANSFORMATION($,$,#14801,#15539);
#427=ITEM_DEFINED_TRANSFORMATION($,$,#14883,#15540);
#428=ITEM_DEFINED_TRANSFORMATION($,$,#14883,#15541);
#429=ITEM_DEFINED_TRANSFORMATION($,$,#14883,#15542);
#430=ITEM_DEFINED_TRANSFORMATION($,$,#14883,#15543);
#431=ITEM_DEFINED_TRANSFORMATION($,$,#14866,#15544);
#432=ITEM_DEFINED_TRANSFORMATION($,$,#14883,#15545);
#433=ITEM_DEFINED_TRANSFORMATION($,$,#14883,#15546);
#434=ITEM_DEFINED_TRANSFORMATION($,$,#14883,#15547);
#435=ITEM_DEFINED_TRANSFORMATION($,$,#14883,#15548);
#436=ITEM_DEFINED_TRANSFORMATION($,$,#14907,#15549);
#437=ITEM_DEFINED_TRANSFORMATION($,$,#14907,#15550);
#438=ITEM_DEFINED_TRANSFORMATION($,$,#15479,#15551);
#439=ITEM_DEFINED_TRANSFORMATION($,$,#15479,#15552);
#440=ITEM_DEFINED_TRANSFORMATION($,$,#15479,#15553);
#441=ITEM_DEFINED_TRANSFORMATION($,$,#15479,#15554);
#442=ITEM_DEFINED_TRANSFORMATION($,$,#15042,#15555);
#443=ITEM_DEFINED_TRANSFORMATION($,$,#15067,#15556);
#444=ITEM_DEFINED_TRANSFORMATION($,$,#15076,#15557);
#445=ITEM_DEFINED_TRANSFORMATION($,$,#15085,#15558);
#446=ITEM_DEFINED_TRANSFORMATION($,$,#15094,#15559);
#447=ITEM_DEFINED_TRANSFORMATION($,$,#15112,#15560);
#448=ITEM_DEFINED_TRANSFORMATION($,$,#15119,#15561);
#449=ITEM_DEFINED_TRANSFORMATION($,$,#15291,#15562);
#450=ITEM_DEFINED_TRANSFORMATION($,$,#15128,#15563);
#451=ITEM_DEFINED_TRANSFORMATION($,$,#15479,#15564);
#452=ITEM_DEFINED_TRANSFORMATION($,$,#15222,#15565);
#453=ITEM_DEFINED_TRANSFORMATION($,$,#15247,#15566);
#454=ITEM_DEFINED_TRANSFORMATION($,$,#15256,#15567);
#455=ITEM_DEFINED_TRANSFORMATION($,$,#15265,#15568);
#456=ITEM_DEFINED_TRANSFORMATION($,$,#15275,#15569);
#457=ITEM_DEFINED_TRANSFORMATION($,$,#15282,#15570);
#458=ITEM_DEFINED_TRANSFORMATION($,$,#15291,#15571);
#459=ITEM_DEFINED_TRANSFORMATION($,$,#15306,#15572);
#460=ITEM_DEFINED_TRANSFORMATION($,$,#15479,#15573);
#461=ITEM_DEFINED_TRANSFORMATION($,$,#14196,#15574);
#462=ITEM_DEFINED_TRANSFORMATION($,$,#14650,#15575);
#463=ITEM_DEFINED_TRANSFORMATION($,$,#15041,#15576);
#464=ITEM_DEFINED_TRANSFORMATION($,$,#15221,#15577);
#465=(
REPRESENTATION_RELATIONSHIP($,$,#58124,#58123)
REPRESENTATION_RELATIONSHIP_WITH_TRANSFORMATION(#377)
SHAPE_REPRESENTATION_RELATIONSHIP()
);
#466=(
REPRESENTATION_RELATIONSHIP($,$,#58125,#58123)
REPRESENTATION_RELATIONSHIP_WITH_TRANSFORMATION(#378)
SHAPE_REPRESENTATION_RELATIONSHIP()
);
#467=(
REPRESENTATION_RELATIONSHIP($,$,#58126,#58123)
REPRESENTATION_RELATIONSHIP_WITH_TRANSFORMATION(#379)
SHAPE_REPRESENTATION_RELATIONSHIP()
);
#468=(
REPRESENTATION_RELATIONSHIP($,$,#58127,#58123)
REPRESENTATION_RELATIONSHIP_WITH_TRANSFORMATION(#380)
SHAPE_REPRESENTATION_RELATIONSHIP()
);
#469=(
REPRESENTATION_RELATIONSHIP($,$,#58128,#58123)
REPRESENTATION_RELATIONSHIP_WITH_TRANSFORMATION(#381)
SHAPE_REPRESENTATION_RELATIONSHIP()
);
#470=(
REPRESENTATION_RELATIONSHIP($,$,#58137,#58136)
REPRESENTATION_RELATIONSHIP_WITH_TRANSFORMATION(#382)
SHAPE_REPRESENTATION_RELATIONSHIP()
);
#471=(
REPRESENTATION_RELATIONSHIP($,$,#58138,#58136)
REPRESENTATION_RELATIONSHIP_WITH_TRANSFORMATION(#383)
SHAPE_REPRESENTATION_RELATIONSHIP()
);
#472=(
REPRESENTATION_RELATIONSHIP($,$,#58139,#58136)
REPRESENTATION_RELATIONSHIP_WITH_TRANSFORMATION(#384)
SHAPE_REPRESENTATION_RELATIONSHIP()
);
#473=(
REPRESENTATION_RELATIONSHIP($,$,#58143,#58142)
REPRESENTATION_RELATIONSHIP_WITH_TRANSFORMATION(#385)
SHAPE_REPRESENTATION_RELATIONSHIP()
);
#474=(
REPRESENTATION_RELATIONSHIP($,$,#58144,#58142)
REPRESENTATION_RELATIONSHIP_WITH_TRANSFORMATION(#386)
SHAPE_REPRESENTATION_RELATIONSHIP()
);
#475=(
REPRESENTATION_RELATIONSHIP($,$,#58145,#58142)
REPRESENTATION_RELATIONSHIP_WITH_TRANSFORMATION(#387)
SHAPE_REPRESENTATION_RELATIONSHIP()
);
#476=(
REPRESENTATION_RELATIONSHIP($,$,#58146,#58142)
REPRESENTATION_RELATIONSHIP_WITH_TRANSFORMATION(#388)
SHAPE_REPRESENTATION_RELATIONSHIP()
);
#477=(
REPRESENTATION_RELATIONSHIP($,$,#58147,#58142)
REPRESENTATION_RELATIONSHIP_WITH_TRANSFORMATION(#389)
SHAPE_REPRESENTATION_RELATIONSHIP()
);
#478=(
REPRESENTATION_RELATIONSHIP($,$,#58111,#58110)
REPRESENTATION_RELATIONSHIP_WITH_TRANSFORMATION(#390)
SHAPE_REPRESENTATION_RELATIONSHIP()
);
#479=(
REPRESENTATION_RELATIONSHIP($,$,#58112,#58110)
REPRESENTATION_RELATIONSHIP_WITH_TRANSFORMATION(#391)
SHAPE_REPRESENTATION_RELATIONSHIP()
);
#480=(
REPRESENTATION_RELATIONSHIP($,$,#58113,#58110)
REPRESENTATION_RELATIONSHIP_WITH_TRANSFORMATION(#392)
SHAPE_REPRESENTATION_RELATIONSHIP()
);
#481=(
REPRESENTATION_RELATIONSHIP($,$,#58114,#58110)
REPRESENTATION_RELATIONSHIP_WITH_TRANSFORMATION(#393)
SHAPE_REPRESENTATION_RELATIONSHIP()
);
#482=(
REPRESENTATION_RELATIONSHIP($,$,#58115,#58110)
REPRESENTATION_RELATIONSHIP_WITH_TRANSFORMATION(#394)
SHAPE_REPRESENTATION_RELATIONSHIP()
);
#483=(
REPRESENTATION_RELATIONSHIP($,$,#58116,#58110)
REPRESENTATION_RELATIONSHIP_WITH_TRANSFORMATION(#395)
SHAPE_REPRESENTATION_RELATIONSHIP()
);
#484=(
REPRESENTATION_RELATIONSHIP($,$,#58117,#58110)
REPRESENTATION_RELATIONSHIP_WITH_TRANSFORMATION(#396)
SHAPE_REPRESENTATION_RELATIONSHIP()
);
#485=(
REPRESENTATION_RELATIONSHIP($,$,#58118,#58110)
REPRESENTATION_RELATIONSHIP_WITH_TRANSFORMATION(#397)
SHAPE_REPRESENTATION_RELATIONSHIP()
);
#486=(
REPRESENTATION_RELATIONSHIP($,$,#58119,#58110)
REPRESENTATION_RELATIONSHIP_WITH_TRANSFORMATION(#398)
SHAPE_REPRESENTATION_RELATIONSHIP()
);
#487=(
REPRESENTATION_RELATIONSHIP($,$,#58120,#58110)
REPRESENTATION_RELATIONSHIP_WITH_TRANSFORMATION(#399)
SHAPE_REPRESENTATION_RELATIONSHIP()
);
#488=(
REPRESENTATION_RELATIONSHIP($,$,#58121,#58110)
REPRESENTATION_RELATIONSHIP_WITH_TRANSFORMATION(#400)
SHAPE_REPRESENTATION_RELATIONSHIP()
);
#489=(
REPRESENTATION_RELATIONSHIP($,$,#58122,#58110)
REPRESENTATION_RELATIONSHIP_WITH_TRANSFORMATION(#401)
SHAPE_REPRESENTATION_RELATIONSHIP()
);
#490=(
REPRESENTATION_RELATIONSHIP($,$,#58129,#58110)
REPRESENTATION_RELATIONSHIP_WITH_TRANSFORMATION(#402)
SHAPE_REPRESENTATION_RELATIONSHIP()
);
#491=(
REPRESENTATION_RELATIONSHIP($,$,#58129,#58110)
REPRESENTATION_RELATIONSHIP_WITH_TRANSFORMATION(#403)
SHAPE_REPRESENTATION_RELATIONSHIP()
);
#492=(
REPRESENTATION_RELATIONSHIP($,$,#58129,#58110)
REPRESENTATION_RELATIONSHIP_WITH_TRANSFORMATION(#404)
SHAPE_REPRESENTATION_RELATIONSHIP()
);
#493=(
REPRESENTATION_RELATIONSHIP($,$,#58129,#58110)
REPRESENTATION_RELATIONSHIP_WITH_TRANSFORMATION(#405)
SHAPE_REPRESENTATION_RELATIONSHIP()
);
#494=(
REPRESENTATION_RELATIONSHIP($,$,#58141,#58110)
REPRESENTATION_RELATIONSHIP_WITH_TRANSFORMATION(#406)
SHAPE_REPRESENTATION_RELATIONSHIP()
);
#495=(
REPRESENTATION_RELATIONSHIP($,$,#58141,#58110)
REPRESENTATION_RELATIONSHIP_WITH_TRANSFORMATION(#407)
SHAPE_REPRESENTATION_RELATIONSHIP()
);
#496=(
REPRESENTATION_RELATIONSHIP($,$,#58141,#58110)
REPRESENTATION_RELATIONSHIP_WITH_TRANSFORMATION(#408)
SHAPE_REPRESENTATION_RELATIONSHIP()
);
#497=(
REPRESENTATION_RELATIONSHIP($,$,#58141,#58110)
REPRESENTATION_RELATIONSHIP_WITH_TRANSFORMATION(#409)
SHAPE_REPRESENTATION_RELATIONSHIP()
);
#498=(
REPRESENTATION_RELATIONSHIP($,$,#58123,#58110)
REPRESENTATION_RELATIONSHIP_WITH_TRANSFORMATION(#410)
SHAPE_REPRESENTATION_RELATIONSHIP()
);
#499=(
REPRESENTATION_RELATIONSHIP($,$,#58123,#58110)
REPRESENTATION_RELATIONSHIP_WITH_TRANSFORMATION(#411)
SHAPE_REPRESENTATION_RELATIONSHIP()
);
#500=(
REPRESENTATION_RELATIONSHIP($,$,#58166,#58110)
REPRESENTATION_RELATIONSHIP_WITH_TRANSFORMATION(#412)
SHAPE_REPRESENTATION_RELATIONSHIP()
);
#501=(
REPRESENTATION_RELATIONSHIP($,$,#58166,#58110)
REPRESENTATION_RELATIONSHIP_WITH_TRANSFORMATION(#413)
SHAPE_REPRESENTATION_RELATIONSHIP()
);
#502=(
REPRESENTATION_RELATIONSHIP($,$,#58166,#58110)
REPRESENTATION_RELATIONSHIP_WITH_TRANSFORMATION(#414)
SHAPE_REPRESENTATION_RELATIONSHIP()
);
#503=(
REPRESENTATION_RELATIONSHIP($,$,#58166,#58110)
REPRESENTATION_RELATIONSHIP_WITH_TRANSFORMATION(#415)
SHAPE_REPRESENTATION_RELATIONSHIP()
);
#504=(
REPRESENTATION_RELATIONSHIP($,$,#58129,#58110)
REPRESENTATION_RELATIONSHIP_WITH_TRANSFORMATION(#416)
SHAPE_REPRESENTATION_RELATIONSHIP()
);
#505=(
REPRESENTATION_RELATIONSHIP($,$,#58129,#58110)
REPRESENTATION_RELATIONSHIP_WITH_TRANSFORMATION(#417)
SHAPE_REPRESENTATION_RELATIONSHIP()
);
#506=(
REPRESENTATION_RELATIONSHIP($,$,#58129,#58110)
REPRESENTATION_RELATIONSHIP_WITH_TRANSFORMATION(#418)
SHAPE_REPRESENTATION_RELATIONSHIP()
);
#507=(
REPRESENTATION_RELATIONSHIP($,$,#58129,#58110)
REPRESENTATION_RELATIONSHIP_WITH_TRANSFORMATION(#419)
SHAPE_REPRESENTATION_RELATIONSHIP()
);
#508=(
REPRESENTATION_RELATIONSHIP($,$,#58140,#58110)
REPRESENTATION_RELATIONSHIP_WITH_TRANSFORMATION(#420)
SHAPE_REPRESENTATION_RELATIONSHIP()
);
#509=(
REPRESENTATION_RELATIONSHIP($,$,#58131,#58130)
REPRESENTATION_RELATIONSHIP_WITH_TRANSFORMATION(#421)
SHAPE_REPRESENTATION_RELATIONSHIP()
);
#510=(
REPRESENTATION_RELATIONSHIP($,$,#58132,#58130)
REPRESENTATION_RELATIONSHIP_WITH_TRANSFORMATION(#422)
SHAPE_REPRESENTATION_RELATIONSHIP()
);
#511=(
REPRESENTATION_RELATIONSHIP($,$,#58133,#58130)
REPRESENTATION_RELATIONSHIP_WITH_TRANSFORMATION(#423)
SHAPE_REPRESENTATION_RELATIONSHIP()
);
#512=(
REPRESENTATION_RELATIONSHIP($,$,#58134,#58130)
REPRESENTATION_RELATIONSHIP_WITH_TRANSFORMATION(#424)
SHAPE_REPRESENTATION_RELATIONSHIP()
);
#513=(
REPRESENTATION_RELATIONSHIP($,$,#58135,#58130)
REPRESENTATION_RELATIONSHIP_WITH_TRANSFORMATION(#425)
SHAPE_REPRESENTATION_RELATIONSHIP()
);
#514=(
REPRESENTATION_RELATIONSHIP($,$,#58136,#58130)
REPRESENTATION_RELATIONSHIP_WITH_TRANSFORMATION(#426)
SHAPE_REPRESENTATION_RELATIONSHIP()
);
#515=(
REPRESENTATION_RELATIONSHIP($,$,#58141,#58130)
REPRESENTATION_RELATIONSHIP_WITH_TRANSFORMATION(#427)
SHAPE_REPRESENTATION_RELATIONSHIP()
);
#516=(
REPRESENTATION_RELATIONSHIP($,$,#58141,#58130)
REPRESENTATION_RELATIONSHIP_WITH_TRANSFORMATION(#428)
SHAPE_REPRESENTATION_RELATIONSHIP()
);
#517=(
REPRESENTATION_RELATIONSHIP($,$,#58141,#58130)
REPRESENTATION_RELATIONSHIP_WITH_TRANSFORMATION(#429)
SHAPE_REPRESENTATION_RELATIONSHIP()
);
#518=(
REPRESENTATION_RELATIONSHIP($,$,#58141,#58130)
REPRESENTATION_RELATIONSHIP_WITH_TRANSFORMATION(#430)
SHAPE_REPRESENTATION_RELATIONSHIP()
);
#519=(
REPRESENTATION_RELATIONSHIP($,$,#58140,#58130)
REPRESENTATION_RELATIONSHIP_WITH_TRANSFORMATION(#431)
SHAPE_REPRESENTATION_RELATIONSHIP()
);
#520=(
REPRESENTATION_RELATIONSHIP($,$,#58141,#58130)
REPRESENTATION_RELATIONSHIP_WITH_TRANSFORMATION(#432)
SHAPE_REPRESENTATION_RELATIONSHIP()
);
#521=(
REPRESENTATION_RELATIONSHIP($,$,#58141,#58130)
REPRESENTATION_RELATIONSHIP_WITH_TRANSFORMATION(#433)
SHAPE_REPRESENTATION_RELATIONSHIP()
);
#522=(
REPRESENTATION_RELATIONSHIP($,$,#58141,#58130)
REPRESENTATION_RELATIONSHIP_WITH_TRANSFORMATION(#434)
SHAPE_REPRESENTATION_RELATIONSHIP()
);
#523=(
REPRESENTATION_RELATIONSHIP($,$,#58141,#58130)
REPRESENTATION_RELATIONSHIP_WITH_TRANSFORMATION(#435)
SHAPE_REPRESENTATION_RELATIONSHIP()
);
#524=(
REPRESENTATION_RELATIONSHIP($,$,#58142,#58130)
REPRESENTATION_RELATIONSHIP_WITH_TRANSFORMATION(#436)
SHAPE_REPRESENTATION_RELATIONSHIP()
);
#525=(
REPRESENTATION_RELATIONSHIP($,$,#58142,#58130)
REPRESENTATION_RELATIONSHIP_WITH_TRANSFORMATION(#437)
SHAPE_REPRESENTATION_RELATIONSHIP()
);
#526=(
REPRESENTATION_RELATIONSHIP($,$,#58166,#58130)
REPRESENTATION_RELATIONSHIP_WITH_TRANSFORMATION(#438)
SHAPE_REPRESENTATION_RELATIONSHIP()
);
#527=(
REPRESENTATION_RELATIONSHIP($,$,#58166,#58130)
REPRESENTATION_RELATIONSHIP_WITH_TRANSFORMATION(#439)
SHAPE_REPRESENTATION_RELATIONSHIP()
);
#528=(
REPRESENTATION_RELATIONSHIP($,$,#58166,#58130)
REPRESENTATION_RELATIONSHIP_WITH_TRANSFORMATION(#440)
SHAPE_REPRESENTATION_RELATIONSHIP()
);
#529=(
REPRESENTATION_RELATIONSHIP($,$,#58166,#58130)
REPRESENTATION_RELATIONSHIP_WITH_TRANSFORMATION(#441)
SHAPE_REPRESENTATION_RELATIONSHIP()
);
#530=(
REPRESENTATION_RELATIONSHIP($,$,#58149,#58148)
REPRESENTATION_RELATIONSHIP_WITH_TRANSFORMATION(#442)
SHAPE_REPRESENTATION_RELATIONSHIP()
);
#531=(
REPRESENTATION_RELATIONSHIP($,$,#58150,#58148)
REPRESENTATION_RELATIONSHIP_WITH_TRANSFORMATION(#443)
SHAPE_REPRESENTATION_RELATIONSHIP()
);
#532=(
REPRESENTATION_RELATIONSHIP($,$,#58151,#58148)
REPRESENTATION_RELATIONSHIP_WITH_TRANSFORMATION(#444)
SHAPE_REPRESENTATION_RELATIONSHIP()
);
#533=(
REPRESENTATION_RELATIONSHIP($,$,#58152,#58148)
REPRESENTATION_RELATIONSHIP_WITH_TRANSFORMATION(#445)
SHAPE_REPRESENTATION_RELATIONSHIP()
);
#534=(
REPRESENTATION_RELATIONSHIP($,$,#58153,#58148)
REPRESENTATION_RELATIONSHIP_WITH_TRANSFORMATION(#446)
SHAPE_REPRESENTATION_RELATIONSHIP()
);
#535=(
REPRESENTATION_RELATIONSHIP($,$,#58154,#58148)
REPRESENTATION_RELATIONSHIP_WITH_TRANSFORMATION(#447)
SHAPE_REPRESENTATION_RELATIONSHIP()
);
#536=(
REPRESENTATION_RELATIONSHIP($,$,#58155,#58148)
REPRESENTATION_RELATIONSHIP_WITH_TRANSFORMATION(#448)
SHAPE_REPRESENTATION_RELATIONSHIP()
);
#537=(
REPRESENTATION_RELATIONSHIP($,$,#58164,#58148)
REPRESENTATION_RELATIONSHIP_WITH_TRANSFORMATION(#449)
SHAPE_REPRESENTATION_RELATIONSHIP()
);
#538=(
REPRESENTATION_RELATIONSHIP($,$,#58156,#58148)
REPRESENTATION_RELATIONSHIP_WITH_TRANSFORMATION(#450)
SHAPE_REPRESENTATION_RELATIONSHIP()
);
#539=(
REPRESENTATION_RELATIONSHIP($,$,#58166,#58148)
REPRESENTATION_RELATIONSHIP_WITH_TRANSFORMATION(#451)
SHAPE_REPRESENTATION_RELATIONSHIP()
);
#540=(
REPRESENTATION_RELATIONSHIP($,$,#58158,#58157)
REPRESENTATION_RELATIONSHIP_WITH_TRANSFORMATION(#452)
SHAPE_REPRESENTATION_RELATIONSHIP()
);
#541=(
REPRESENTATION_RELATIONSHIP($,$,#58159,#58157)
REPRESENTATION_RELATIONSHIP_WITH_TRANSFORMATION(#453)
SHAPE_REPRESENTATION_RELATIONSHIP()
);
#542=(
REPRESENTATION_RELATIONSHIP($,$,#58160,#58157)
REPRESENTATION_RELATIONSHIP_WITH_TRANSFORMATION(#454)
SHAPE_REPRESENTATION_RELATIONSHIP()
);
#543=(
REPRESENTATION_RELATIONSHIP($,$,#58161,#58157)
REPRESENTATION_RELATIONSHIP_WITH_TRANSFORMATION(#455)
SHAPE_REPRESENTATION_RELATIONSHIP()
);
#544=(
REPRESENTATION_RELATIONSHIP($,$,#58162,#58157)
REPRESENTATION_RELATIONSHIP_WITH_TRANSFORMATION(#456)
SHAPE_REPRESENTATION_RELATIONSHIP()
);
#545=(
REPRESENTATION_RELATIONSHIP($,$,#58163,#58157)
REPRESENTATION_RELATIONSHIP_WITH_TRANSFORMATION(#457)
SHAPE_REPRESENTATION_RELATIONSHIP()
);
#546=(
REPRESENTATION_RELATIONSHIP($,$,#58164,#58157)
REPRESENTATION_RELATIONSHIP_WITH_TRANSFORMATION(#458)
SHAPE_REPRESENTATION_RELATIONSHIP()
);
#547=(
REPRESENTATION_RELATIONSHIP($,$,#58165,#58157)
REPRESENTATION_RELATIONSHIP_WITH_TRANSFORMATION(#459)
SHAPE_REPRESENTATION_RELATIONSHIP()
);
#548=(
REPRESENTATION_RELATIONSHIP($,$,#58166,#58157)
REPRESENTATION_RELATIONSHIP_WITH_TRANSFORMATION(#460)
SHAPE_REPRESENTATION_RELATIONSHIP()
);
#549=(
REPRESENTATION_RELATIONSHIP($,$,#58110,#58109)
REPRESENTATION_RELATIONSHIP_WITH_TRANSFORMATION(#461)
SHAPE_REPRESENTATION_RELATIONSHIP()
);
#550=(
REPRESENTATION_RELATIONSHIP($,$,#58130,#58109)
REPRESENTATION_RELATIONSHIP_WITH_TRANSFORMATION(#462)
SHAPE_REPRESENTATION_RELATIONSHIP()
);
#551=(
REPRESENTATION_RELATIONSHIP($,$,#58148,#58109)
REPRESENTATION_RELATIONSHIP_WITH_TRANSFORMATION(#463)
SHAPE_REPRESENTATION_RELATIONSHIP()
);
#552=(
REPRESENTATION_RELATIONSHIP($,$,#58157,#58109)
REPRESENTATION_RELATIONSHIP_WITH_TRANSFORMATION(#464)
SHAPE_REPRESENTATION_RELATIONSHIP()
);
#553=CONTEXT_DEPENDENT_SHAPE_REPRESENTATION(#465,#57983);
#554=CONTEXT_DEPENDENT_SHAPE_REPRESENTATION(#466,#57984);
#555=CONTEXT_DEPENDENT_SHAPE_REPRESENTATION(#467,#57985);
#556=CONTEXT_DEPENDENT_SHAPE_REPRESENTATION(#468,#57986);
#557=CONTEXT_DEPENDENT_SHAPE_REPRESENTATION(#469,#57987);
#558=CONTEXT_DEPENDENT_SHAPE_REPRESENTATION(#470,#57999);
#559=CONTEXT_DEPENDENT_SHAPE_REPRESENTATION(#471,#58000);
#560=CONTEXT_DEPENDENT_SHAPE_REPRESENTATION(#472,#58001);
#561=CONTEXT_DEPENDENT_SHAPE_REPRESENTATION(#473,#58010);
#562=CONTEXT_DEPENDENT_SHAPE_REPRESENTATION(#474,#58011);
#563=CONTEXT_DEPENDENT_SHAPE_REPRESENTATION(#475,#58012);
#564=CONTEXT_DEPENDENT_SHAPE_REPRESENTATION(#476,#58013);
#565=CONTEXT_DEPENDENT_SHAPE_REPRESENTATION(#477,#58014);
#566=CONTEXT_DEPENDENT_SHAPE_REPRESENTATION(#478,#58034);
#567=CONTEXT_DEPENDENT_SHAPE_REPRESENTATION(#479,#58035);
#568=CONTEXT_DEPENDENT_SHAPE_REPRESENTATION(#480,#58036);
#569=CONTEXT_DEPENDENT_SHAPE_REPRESENTATION(#481,#58037);
#570=CONTEXT_DEPENDENT_SHAPE_REPRESENTATION(#482,#58038);
#571=CONTEXT_DEPENDENT_SHAPE_REPRESENTATION(#483,#58039);
#572=CONTEXT_DEPENDENT_SHAPE_REPRESENTATION(#484,#58040);
#573=CONTEXT_DEPENDENT_SHAPE_REPRESENTATION(#485,#58041);
#574=CONTEXT_DEPENDENT_SHAPE_REPRESENTATION(#486,#58042);
#575=CONTEXT_DEPENDENT_SHAPE_REPRESENTATION(#487,#58043);
#576=CONTEXT_DEPENDENT_SHAPE_REPRESENTATION(#488,#58044);
#577=CONTEXT_DEPENDENT_SHAPE_REPRESENTATION(#489,#58045);
#578=CONTEXT_DEPENDENT_SHAPE_REPRESENTATION(#490,#58046);
#579=CONTEXT_DEPENDENT_SHAPE_REPRESENTATION(#491,#58047);
#580=CONTEXT_DEPENDENT_SHAPE_REPRESENTATION(#492,#58048);
#581=CONTEXT_DEPENDENT_SHAPE_REPRESENTATION(#493,#58049);
#582=CONTEXT_DEPENDENT_SHAPE_REPRESENTATION(#494,#58050);
#583=CONTEXT_DEPENDENT_SHAPE_REPRESENTATION(#495,#58051);
#584=CONTEXT_DEPENDENT_SHAPE_REPRESENTATION(#496,#58052);
#585=CONTEXT_DEPENDENT_SHAPE_REPRESENTATION(#497,#58053);
#586=CONTEXT_DEPENDENT_SHAPE_REPRESENTATION(#498,#58054);
#587=CONTEXT_DEPENDENT_SHAPE_REPRESENTATION(#499,#58055);
#588=CONTEXT_DEPENDENT_SHAPE_REPRESENTATION(#500,#58056);
#589=CONTEXT_DEPENDENT_SHAPE_REPRESENTATION(#501,#58057);
#590=CONTEXT_DEPENDENT_SHAPE_REPRESENTATION(#502,#58058);
#591=CONTEXT_DEPENDENT_SHAPE_REPRESENTATION(#503,#58059);
#592=CONTEXT_DEPENDENT_SHAPE_REPRESENTATION(#504,#58060);
#593=CONTEXT_DEPENDENT_SHAPE_REPRESENTATION(#505,#58061);
#594=CONTEXT_DEPENDENT_SHAPE_REPRESENTATION(#506,#58062);
#595=CONTEXT_DEPENDENT_SHAPE_REPRESENTATION(#507,#58063);
#596=CONTEXT_DEPENDENT_SHAPE_REPRESENTATION(#508,#58064);
#597=CONTEXT_DEPENDENT_SHAPE_REPRESENTATION(#509,#58065);
#598=CONTEXT_DEPENDENT_SHAPE_REPRESENTATION(#510,#58066);
#599=CONTEXT_DEPENDENT_SHAPE_REPRESENTATION(#511,#58067);
#600=CONTEXT_DEPENDENT_SHAPE_REPRESENTATION(#512,#58068);
#601=CONTEXT_DEPENDENT_SHAPE_REPRESENTATION(#513,#58069);
#602=CONTEXT_DEPENDENT_SHAPE_REPRESENTATION(#514,#58070);
#603=CONTEXT_DEPENDENT_SHAPE_REPRESENTATION(#515,#58071);
#604=CONTEXT_DEPENDENT_SHAPE_REPRESENTATION(#516,#58072);
#605=CONTEXT_DEPENDENT_SHAPE_REPRESENTATION(#517,#58073);
#606=CONTEXT_DEPENDENT_SHAPE_REPRESENTATION(#518,#58074);
#607=CONTEXT_DEPENDENT_SHAPE_REPRESENTATION(#519,#58075);
#608=CONTEXT_DEPENDENT_SHAPE_REPRESENTATION(#520,#58076);
#609=CONTEXT_DEPENDENT_SHAPE_REPRESENTATION(#521,#58077);
#610=CONTEXT_DEPENDENT_SHAPE_REPRESENTATION(#522,#58078);
#611=CONTEXT_DEPENDENT_SHAPE_REPRESENTATION(#523,#58079);
#612=CONTEXT_DEPENDENT_SHAPE_REPRESENTATION(#524,#58080);
#613=CONTEXT_DEPENDENT_SHAPE_REPRESENTATION(#525,#58081);
#614=CONTEXT_DEPENDENT_SHAPE_REPRESENTATION(#526,#58082);
#615=CONTEXT_DEPENDENT_SHAPE_REPRESENTATION(#527,#58083);
#616=CONTEXT_DEPENDENT_SHAPE_REPRESENTATION(#528,#58084);
#617=CONTEXT_DEPENDENT_SHAPE_REPRESENTATION(#529,#58085);
#618=CONTEXT_DEPENDENT_SHAPE_REPRESENTATION(#530,#58086);
#619=CONTEXT_DEPENDENT_SHAPE_REPRESENTATION(#531,#58087);
#620=CONTEXT_DEPENDENT_SHAPE_REPRESENTATION(#532,#58088);
#621=CONTEXT_DEPENDENT_SHAPE_REPRESENTATION(#533,#58089);
#622=CONTEXT_DEPENDENT_SHAPE_REPRESENTATION(#534,#58090);
#623=CONTEXT_DEPENDENT_SHAPE_REPRESENTATION(#535,#58091);
#624=CONTEXT_DEPENDENT_SHAPE_REPRESENTATION(#536,#58092);
#625=CONTEXT_DEPENDENT_SHAPE_REPRESENTATION(#537,#58093);
#626=CONTEXT_DEPENDENT_SHAPE_REPRESENTATION(#538,#58094);
#627=CONTEXT_DEPENDENT_SHAPE_REPRESENTATION(#539,#58095);
#628=CONTEXT_DEPENDENT_SHAPE_REPRESENTATION(#540,#58096);
#629=CONTEXT_DEPENDENT_SHAPE_REPRESENTATION(#541,#58097);
#630=CONTEXT_DEPENDENT_SHAPE_REPRESENTATION(#542,#58098);
#631=CONTEXT_DEPENDENT_SHAPE_REPRESENTATION(#543,#58099);
#632=CONTEXT_DEPENDENT_SHAPE_REPRESENTATION(#544,#58100);
#633=CONTEXT_DEPENDENT_SHAPE_REPRESENTATION(#545,#58101);
#634=CONTEXT_DEPENDENT_SHAPE_REPRESENTATION(#546,#58102);
#635=CONTEXT_DEPENDENT_SHAPE_REPRESENTATION(#547,#58103);
#636=CONTEXT_DEPENDENT_SHAPE_REPRESENTATION(#548,#58104);
#637=CONTEXT_DEPENDENT_SHAPE_REPRESENTATION(#549,#58105);
#638=CONTEXT_DEPENDENT_SHAPE_REPRESENTATION(#550,#58106);
#639=CONTEXT_DEPENDENT_SHAPE_REPRESENTATION(#551,#58107);
#640=CONTEXT_DEPENDENT_SHAPE_REPRESENTATION(#552,#58108);
#641=NEXT_ASSEMBLY_USAGE_OCCURRENCE('Inner ring:1','Inner ring:1',
'Inner ring:1',#58182,#58183,'Inner ring:1');
#642=NEXT_ASSEMBLY_USAGE_OCCURRENCE('Outer ring:1','Outer ring:1',
'Outer ring:1',#58182,#58184,'Outer ring:1');
#643=NEXT_ASSEMBLY_USAGE_OCCURRENCE('Balls:1','Balls:1','Balls:1',#58182,
#58185,'Balls:1');
#644=NEXT_ASSEMBLY_USAGE_OCCURRENCE('Cage:1','Cage:1','Cage:1',#58182,#58186,
'Cage:1');
#645=NEXT_ASSEMBLY_USAGE_OCCURRENCE('Seals 2RS:1','Seals 2RS:1',
'Seals 2RS:1',#58182,#58187,'Seals 2RS:1');
#646=NEXT_ASSEMBLY_USAGE_OCCURRENCE('Block:1','Block:1','Block:1',#58195,
#58196,'Block:1');
#647=NEXT_ASSEMBLY_USAGE_OCCURRENCE('End cap +:1','End cap +:1',
'End cap +:1',#58195,#58197,'End cap +:1');
#648=NEXT_ASSEMBLY_USAGE_OCCURRENCE('End cap:1','End cap:1','End cap:1',
#58195,#58198,'End cap:1');
#649=NEXT_ASSEMBLY_USAGE_OCCURRENCE('Inner ring (1):1',
'Inner ring (1):1','Inner ring (1):1',#58201,#58202,'Inner ring (1):1');
#650=NEXT_ASSEMBLY_USAGE_OCCURRENCE('Outer ring (1):1',
'Outer ring (1):1','Outer ring (1):1',#58201,#58203,'Outer ring (1):1');
#651=NEXT_ASSEMBLY_USAGE_OCCURRENCE('Balls (1):1','Balls (1):1',
'Balls (1):1',#58201,#58204,'Balls (1):1');
#652=NEXT_ASSEMBLY_USAGE_OCCURRENCE('Cage (1):1','Cage (1):1',
'Cage (1):1',#58201,#58205,'Cage (1):1');
#653=NEXT_ASSEMBLY_USAGE_OCCURRENCE('Seals 2RS (1):1','Seals 2RS (1):1',
'Seals 2RS (1):1',#58201,#58206,'Seals 2RS (1):1');
#654=NEXT_ASSEMBLY_USAGE_OCCURRENCE('Base:1','Base:1','Base:1',#58169,#58170,
'Base:1');
#655=NEXT_ASSEMBLY_USAGE_OCCURRENCE('Foot strip:1','Foot strip:1',
'Foot strip:1',#58169,#58171,'Foot strip:1');
#656=NEXT_ASSEMBLY_USAGE_OCCURRENCE('Foot strip (1):1',
'Foot strip (1):1','Foot strip (1):1',#58169,#58172,'Foot strip (1):1');
#657=NEXT_ASSEMBLY_USAGE_OCCURRENCE('Input bearing post:1',
'Input bearing post:1','Input bearing post:1',#58169,#58173,
'Input bearing post:1');
#658=NEXT_ASSEMBLY_USAGE_OCCURRENCE('Input outer race spacer:1',
'Input outer race spacer:1','Input outer race spacer:1',#58169,#58174,
'Input outer race spacer:1');
#659=NEXT_ASSEMBLY_USAGE_OCCURRENCE('Input bearing cap:1',
'Input bearing cap:1','Input bearing cap:1',#58169,#58175,
'Input bearing cap:1');
#660=NEXT_ASSEMBLY_USAGE_OCCURRENCE('Indicator stand:1',
'Indicator stand:1','Indicator stand:1',#58169,#58176,
'Indicator stand:1');
#661=NEXT_ASSEMBLY_USAGE_OCCURRENCE('Indicator arm:1','Indicator arm:1',
'Indicator arm:1',#58169,#58177,'Indicator arm:1');
#662=NEXT_ASSEMBLY_USAGE_OCCURRENCE('Indicator body envelope:1',
'Indicator body envelope:1','Indicator body envelope:1',#58169,#58178,
'Indicator body envelope:1');
#663=NEXT_ASSEMBLY_USAGE_OCCURRENCE('Indicator face:1',
'Indicator face:1','Indicator face:1',#58169,#58179,'Indicator face:1');
#664=NEXT_ASSEMBLY_USAGE_OCCURRENCE('Retracted indicator probe:1',
'Retracted indicator probe:1','Retracted indicator probe:1',#58169,#58180,
'Retracted indicator probe:1');
#665=NEXT_ASSEMBLY_USAGE_OCCURRENCE(
'Linear Guide Rail - 15 mm, 220 mm Long:2',
'Linear Guide Rail - 15 mm, 220 mm Long:2',
'Linear Guide Rail - 15 mm, 220 mm Long:2',#58169,#58181,
'Linear Guide Rail - 15 mm, 220 mm Long:2');
#666=NEXT_ASSEMBLY_USAGE_OCCURRENCE('Cap Screw - M4x16:2',
'Cap Screw - M4x16:2','Cap Screw - M4x16:2',#58169,#58188,
'Cap Screw - M4x16:2');
#667=NEXT_ASSEMBLY_USAGE_OCCURRENCE('Cap Screw - M4x16:3',
'Cap Screw - M4x16:3','Cap Screw - M4x16:3',#58169,#58188,
'Cap Screw - M4x16:3');
#668=NEXT_ASSEMBLY_USAGE_OCCURRENCE('Cap Screw - M4x16:4',
'Cap Screw - M4x16:4','Cap Screw - M4x16:4',#58169,#58188,
'Cap Screw - M4x16:4');
#669=NEXT_ASSEMBLY_USAGE_OCCURRENCE('Cap Screw - M4x16:5',
'Cap Screw - M4x16:5','Cap Screw - M4x16:5',#58169,#58188,
'Cap Screw - M4x16:5');
#670=NEXT_ASSEMBLY_USAGE_OCCURRENCE('M5x14 Cap Screw:6',
'M5x14 Cap Screw:6','M5x14 Cap Screw:6',#58169,#58200,
'M5x14 Cap Screw:6');
#671=NEXT_ASSEMBLY_USAGE_OCCURRENCE('M5x14 Cap Screw:7',
'M5x14 Cap Screw:7','M5x14 Cap Screw:7',#58169,#58200,
'M5x14 Cap Screw:7');
#672=NEXT_ASSEMBLY_USAGE_OCCURRENCE('M5x14 Cap Screw:8',
'M5x14 Cap Screw:8','M5x14 Cap Screw:8',#58169,#58200,
'M5x14 Cap Screw:8');
#673=NEXT_ASSEMBLY_USAGE_OCCURRENCE('M5x14 Cap Screw:9',
'M5x14 Cap Screw:9','M5x14 Cap Screw:9',#58169,#58200,
'M5x14 Cap Screw:9');
#674=NEXT_ASSEMBLY_USAGE_OCCURRENCE(
'Sealed Ball Bearing - 12 x 32 x 10 mm:2',
'Sealed Ball Bearing - 12 x 32 x 10 mm:2',
'Sealed Ball Bearing - 12 x 32 x 10 mm:2',#58169,#58182,
'Sealed Ball Bearing - 12 x 32 x 10 mm:2');
#675=NEXT_ASSEMBLY_USAGE_OCCURRENCE(
'Sealed Ball Bearing - 12 x 32 x 10 mm:3',
'Sealed Ball Bearing - 12 x 32 x 10 mm:3',
'Sealed Ball Bearing - 12 x 32 x 10 mm:3',#58169,#58182,
'Sealed Ball Bearing - 12 x 32 x 10 mm:3');
#676=NEXT_ASSEMBLY_USAGE_OCCURRENCE('M4x10 Cap Screw:2',
'M4x10 Cap Screw:2','M4x10 Cap Screw:2',#58169,#58225,
'M4x10 Cap Screw:2');
#677=NEXT_ASSEMBLY_USAGE_OCCURRENCE('M4x10 Cap Screw:3',
'M4x10 Cap Screw:3','M4x10 Cap Screw:3',#58169,#58225,
'M4x10 Cap Screw:3');
#678=NEXT_ASSEMBLY_USAGE_OCCURRENCE('M4x10 Cap Screw:4',
'M4x10 Cap Screw:4','M4x10 Cap Screw:4',#58169,#58225,
'M4x10 Cap Screw:4');
#679=NEXT_ASSEMBLY_USAGE_OCCURRENCE('M4x10 Cap Screw:5',
'M4x10 Cap Screw:5','M4x10 Cap Screw:5',#58169,#58225,
'M4x10 Cap Screw:5');
#680=NEXT_ASSEMBLY_USAGE_OCCURRENCE('Cap Screw - M4x16:6',
'Cap Screw - M4x16:6','Cap Screw - M4x16:6',#58169,#58188,
'Cap Screw - M4x16:6');
#681=NEXT_ASSEMBLY_USAGE_OCCURRENCE('Cap Screw - M4x16:7',
'Cap Screw - M4x16:7','Cap Screw - M4x16:7',#58169,#58188,
'Cap Screw - M4x16:7');
#682=NEXT_ASSEMBLY_USAGE_OCCURRENCE('Cap Screw - M4x16:8',
'Cap Screw - M4x16:8','Cap Screw - M4x16:8',#58169,#58188,
'Cap Screw - M4x16:8');
#683=NEXT_ASSEMBLY_USAGE_OCCURRENCE('Cap Screw - M4x16:9',
'Cap Screw - M4x16:9','Cap Screw - M4x16:9',#58169,#58188,
'Cap Screw - M4x16:9');
#684=NEXT_ASSEMBLY_USAGE_OCCURRENCE('Socket Set Screw - M4x6:3',
'Socket Set Screw - M4x6:3','Socket Set Screw - M4x6:3',#58169,#58199,
'Socket Set Screw - M4x6:3');
#685=NEXT_ASSEMBLY_USAGE_OCCURRENCE('Carrier plate:1','Carrier plate:1',
'Carrier plate:1',#58189,#58190,'Carrier plate:1');
#686=NEXT_ASSEMBLY_USAGE_OCCURRENCE('Retracted rail lock pad:1',
'Retracted rail lock pad:1','Retracted rail lock pad:1',#58189,#58191,
'Retracted rail lock pad:1');
#687=NEXT_ASSEMBLY_USAGE_OCCURRENCE('Output bearing post:1',
'Output bearing post:1','Output bearing post:1',#58189,#58192,
'Output bearing post:1');
#688=NEXT_ASSEMBLY_USAGE_OCCURRENCE('Output outer race spacer:1',
'Output outer race spacer:1','Output outer race spacer:1',#58189,#58193,
'Output outer race spacer:1');
#689=NEXT_ASSEMBLY_USAGE_OCCURRENCE('Output bearing cap:1',
'Output bearing cap:1','Output bearing cap:1',#58189,#58194,
'Output bearing cap:1');
#690=NEXT_ASSEMBLY_USAGE_OCCURRENCE(
'Flanged Linear Guide Carriage - 15 mm:2',
'Flanged Linear Guide Carriage - 15 mm:2',
'Flanged Linear Guide Carriage - 15 mm:2',#58189,#58195,
'Flanged Linear Guide Carriage - 15 mm:2');
#691=NEXT_ASSEMBLY_USAGE_OCCURRENCE('M5x14 Cap Screw:2',
'M5x14 Cap Screw:2','M5x14 Cap Screw:2',#58189,#58200,
'M5x14 Cap Screw:2');
#692=NEXT_ASSEMBLY_USAGE_OCCURRENCE('M5x14 Cap Screw:3',
'M5x14 Cap Screw:3','M5x14 Cap Screw:3',#58189,#58200,
'M5x14 Cap Screw:3');
#693=NEXT_ASSEMBLY_USAGE_OCCURRENCE('M5x14 Cap Screw:4',
'M5x14 Cap Screw:4','M5x14 Cap Screw:4',#58189,#58200,
'M5x14 Cap Screw:4');
#694=NEXT_ASSEMBLY_USAGE_OCCURRENCE('M5x14 Cap Screw:5',
'M5x14 Cap Screw:5','M5x14 Cap Screw:5',#58189,#58200,
'M5x14 Cap Screw:5');
#695=NEXT_ASSEMBLY_USAGE_OCCURRENCE('Socket Set Screw - M4x6:2',
'Socket Set Screw - M4x6:2','Socket Set Screw - M4x6:2',#58189,#58199,
'Socket Set Screw - M4x6:2');
#696=NEXT_ASSEMBLY_USAGE_OCCURRENCE('M5x14 Cap Screw:10',
'M5x14 Cap Screw:10','M5x14 Cap Screw:10',#58189,#58200,
'M5x14 Cap Screw:10');
#697=NEXT_ASSEMBLY_USAGE_OCCURRENCE('M5x14 Cap Screw:11',
'M5x14 Cap Screw:11','M5x14 Cap Screw:11',#58189,#58200,
'M5x14 Cap Screw:11');
#698=NEXT_ASSEMBLY_USAGE_OCCURRENCE('M5x14 Cap Screw:12',
'M5x14 Cap Screw:12','M5x14 Cap Screw:12',#58189,#58200,
'M5x14 Cap Screw:12');
#699=NEXT_ASSEMBLY_USAGE_OCCURRENCE('M5x14 Cap Screw:13',
'M5x14 Cap Screw:13','M5x14 Cap Screw:13',#58189,#58200,
'M5x14 Cap Screw:13');
#700=NEXT_ASSEMBLY_USAGE_OCCURRENCE(
'Sealed Ball Bearing - 20 x 47 x 14 mm:2',
'Sealed Ball Bearing - 20 x 47 x 14 mm:2',
'Sealed Ball Bearing - 20 x 47 x 14 mm:2',#58189,#58201,
'Sealed Ball Bearing - 20 x 47 x 14 mm:2');
#701=NEXT_ASSEMBLY_USAGE_OCCURRENCE(
'Sealed Ball Bearing - 20 x 47 x 14 mm:3',
'Sealed Ball Bearing - 20 x 47 x 14 mm:3',
'Sealed Ball Bearing - 20 x 47 x 14 mm:3',#58189,#58201,
'Sealed Ball Bearing - 20 x 47 x 14 mm:3');
#702=NEXT_ASSEMBLY_USAGE_OCCURRENCE('M4x10 Cap Screw:7',
'M4x10 Cap Screw:7','M4x10 Cap Screw:7',#58189,#58225,
'M4x10 Cap Screw:7');
#703=NEXT_ASSEMBLY_USAGE_OCCURRENCE('M4x10 Cap Screw:8',
'M4x10 Cap Screw:8','M4x10 Cap Screw:8',#58189,#58225,
'M4x10 Cap Screw:8');
#704=NEXT_ASSEMBLY_USAGE_OCCURRENCE('M4x10 Cap Screw:9',
'M4x10 Cap Screw:9','M4x10 Cap Screw:9',#58189,#58225,
'M4x10 Cap Screw:9');
#705=NEXT_ASSEMBLY_USAGE_OCCURRENCE('M4x10 Cap Screw:10',
'M4x10 Cap Screw:10','M4x10 Cap Screw:10',#58189,#58225,
'M4x10 Cap Screw:10');
#706=NEXT_ASSEMBLY_USAGE_OCCURRENCE('Input arbor:1','Input arbor:1',
'Input arbor:1',#58207,#58208,'Input arbor:1');
#707=NEXT_ASSEMBLY_USAGE_OCCURRENCE('Input inner sleeve 10 mm:1',
'Input inner sleeve 10 mm:1','Input inner sleeve 10 mm:1',#58207,#58209,
'Input inner sleeve 10 mm:1');
#708=NEXT_ASSEMBLY_USAGE_OCCURRENCE('Input inner sleeve 8 mm:1',
'Input inner sleeve 8 mm:1','Input inner sleeve 8 mm:1',#58207,#58210,
'Input inner sleeve 8 mm:1');
#709=NEXT_ASSEMBLY_USAGE_OCCURRENCE('Input lower sleeve:1',
'Input lower sleeve:1','Input lower sleeve:1',#58207,#58211,
'Input lower sleeve:1');
#710=NEXT_ASSEMBLY_USAGE_OCCURRENCE('Input collar:1','Input collar:1',
'Input collar:1',#58207,#58212,'Input collar:1');
#711=NEXT_ASSEMBLY_USAGE_OCCURRENCE('Input parallel key:1',
'Input parallel key:1','Input parallel key:1',#58207,#58213,
'Input parallel key:1');
#712=NEXT_ASSEMBLY_USAGE_OCCURRENCE('Input keeper:1','Input keeper:1',
'Input keeper:1',#58207,#58214,'Input keeper:1');
#713=NEXT_ASSEMBLY_USAGE_OCCURRENCE('M4x4 collar screw:2',
'M4x4 collar screw:2','M4x4 collar screw:2',#58207,#58223,
'M4x4 collar screw:2');
#714=NEXT_ASSEMBLY_USAGE_OCCURRENCE(
'Spur Gear - Module 2, 20 Teeth, 12 mm Bore:2',
'Spur Gear - Module 2, 20 Teeth, 12 mm Bore:2',
'Spur Gear - Module 2, 20 Teeth, 12 mm Bore:2',#58207,#58215,
'Spur Gear - Module 2, 20 Teeth, 12 mm Bore:2');
#715=NEXT_ASSEMBLY_USAGE_OCCURRENCE('M4x10 Cap Screw:6',
'M4x10 Cap Screw:6','M4x10 Cap Screw:6',#58207,#58225,
'M4x10 Cap Screw:6');
#716=NEXT_ASSEMBLY_USAGE_OCCURRENCE('Output arbor:1','Output arbor:1',
'Output arbor:1',#58216,#58217,'Output arbor:1');
#717=NEXT_ASSEMBLY_USAGE_OCCURRENCE('Output inner sleeve 6 mm:1',
'Output inner sleeve 6 mm:1','Output inner sleeve 6 mm:1',#58216,#58218,
'Output inner sleeve 6 mm:1');
#718=NEXT_ASSEMBLY_USAGE_OCCURRENCE('Output inner sleeve 8 mm:1',
'Output inner sleeve 8 mm:1','Output inner sleeve 8 mm:1',#58216,#58219,
'Output inner sleeve 8 mm:1');
#719=NEXT_ASSEMBLY_USAGE_OCCURRENCE('Output collar:1','Output collar:1',
'Output collar:1',#58216,#58220,'Output collar:1');
#720=NEXT_ASSEMBLY_USAGE_OCCURRENCE('Output parallel key:1',
'Output parallel key:1','Output parallel key:1',#58216,#58221,
'Output parallel key:1');
#721=NEXT_ASSEMBLY_USAGE_OCCURRENCE('Output keeper:1','Output keeper:1',
'Output keeper:1',#58216,#58222,'Output keeper:1');
#722=NEXT_ASSEMBLY_USAGE_OCCURRENCE('M4x4 collar screw:3',
'M4x4 collar screw:3','M4x4 collar screw:3',#58216,#58223,
'M4x4 collar screw:3');
#723=NEXT_ASSEMBLY_USAGE_OCCURRENCE(
'Spur Gear - Module 2, 40 Teeth, 20 mm Bore:2',
'Spur Gear - Module 2, 40 Teeth, 20 mm Bore:2',
'Spur Gear - Module 2, 40 Teeth, 20 mm Bore:2',#58216,#58224,
'Spur Gear - Module 2, 40 Teeth, 20 mm Bore:2');
#724=NEXT_ASSEMBLY_USAGE_OCCURRENCE('M4x10 Cap Screw:11',
'M4x10 Cap Screw:11','M4x10 Cap Screw:11',#58216,#58225,
'M4x10 Cap Screw:11');
#725=NEXT_ASSEMBLY_USAGE_OCCURRENCE('Base and indicator stand:1',
'Base and indicator stand:1','Base and indicator stand:1',#58168,#58169,
'Base and indicator stand:1');
#726=NEXT_ASSEMBLY_USAGE_OCCURRENCE('Sliding bearing carrier:1',
'Sliding bearing carrier:1','Sliding bearing carrier:1',#58168,#58189,
'Sliding bearing carrier:1');
#727=NEXT_ASSEMBLY_USAGE_OCCURRENCE('Input gear and arbor:1',
'Input gear and arbor:1','Input gear and arbor:1',#58168,#58207,
'Input gear and arbor:1');
#728=NEXT_ASSEMBLY_USAGE_OCCURRENCE('Output gear and arbor:1',
'Output gear and arbor:1','Output gear and arbor:1',#58168,#58216,
'Output gear and arbor:1');
#729=SPHERICAL_SURFACE('',#14538,0.29765);
#730=SPHERICAL_SURFACE('',#14540,0.29765);
#731=SPHERICAL_SURFACE('',#14542,0.29765);
#732=SPHERICAL_SURFACE('',#14544,0.29765);
#733=SPHERICAL_SURFACE('',#14546,0.29765);
#734=SPHERICAL_SURFACE('',#14548,0.29765);
#735=SPHERICAL_SURFACE('',#14550,0.29765);
#736=SPHERICAL_SURFACE('',#14553,0.309556);
#737=SPHERICAL_SURFACE('',#14569,0.309556);
#738=SPHERICAL_SURFACE('',#14574,0.309556);
#739=SPHERICAL_SURFACE('',#14580,0.309556);
#740=SPHERICAL_SURFACE('',#14585,0.309556);
#741=SPHERICAL_SURFACE('',#14590,0.309556);
#742=SPHERICAL_SURFACE('',#14598,0.309556);
#743=SPHERICAL_SURFACE('',#14949,0.3969);
#744=SPHERICAL_SURFACE('',#14951,0.3969);
#745=SPHERICAL_SURFACE('',#14953,0.3969);
#746=SPHERICAL_SURFACE('',#14955,0.3969);
#747=SPHERICAL_SURFACE('',#14957,0.3969);
#748=SPHERICAL_SURFACE('',#14959,0.3969);
#749=SPHERICAL_SURFACE('',#14961,0.3969);
#750=SPHERICAL_SURFACE('',#14963,0.3969);
#751=SPHERICAL_SURFACE('',#14966,0.412776);
#752=SPHERICAL_SURFACE('',#14982,0.412776);
#753=SPHERICAL_SURFACE('',#14987,0.412776);
#754=SPHERICAL_SURFACE('',#14992,0.412776);
#755=SPHERICAL_SURFACE('',#14997,0.412776);
#756=SPHERICAL_SURFACE('',#15002,0.412776);
#757=SPHERICAL_SURFACE('',#15007,0.412776);
#758=SPHERICAL_SURFACE('',#15015,0.412776);
#759=CONICAL_SURFACE('',#14509,0.63,0.785398163397448);
#760=CONICAL_SURFACE('',#14516,0.63,0.785398163397448);
#761=CONICAL_SURFACE('',#14529,1.57,0.785398163397449);
#762=CONICAL_SURFACE('',#14533,1.57,0.785398163397449);
#763=CONICAL_SURFACE('',#14627,0.325,0.785398163397448);
#764=CONICAL_SURFACE('',#14631,0.335,0.785398163397448);
#765=CONICAL_SURFACE('',#14635,0.21,0.463647609000806);
#766=CONICAL_SURFACE('',#14639,0.18,0.785398163397448);
#767=CONICAL_SURFACE('',#14876,0.185,0.785398163397449);
#768=CONICAL_SURFACE('',#14880,0.1625,0.785398163397449);
#769=CONICAL_SURFACE('',#14896,0.4,0.785398163397448);
#770=CONICAL_SURFACE('',#14900,0.41,0.785398163397448);
#771=CONICAL_SURFACE('',#14904,0.26,0.463647609000806);
#772=CONICAL_SURFACE('',#14920,1.05,0.785398163397449);
#773=CONICAL_SURFACE('',#14927,1.05,0.785398163397449);
#774=CONICAL_SURFACE('',#14940,2.3,0.785398163397449);
#775=CONICAL_SURFACE('',#14944,2.3,0.785398163397449);
#776=CONICAL_SURFACE('',#15303,0.185,0.785398163397449);
#777=CONICAL_SURFACE('',#15492,0.325,0.785398163397448);
#778=CONICAL_SURFACE('',#15496,0.335,0.785398163397448);
#779=CONICAL_SURFACE('',#15500,0.21,0.463647609000806);
#780=TOROIDAL_SURFACE('',#14498,1.1,0.309556);
#781=TOROIDAL_SURFACE('',#14518,1.1,0.309556);
#782=TOROIDAL_SURFACE('',#14909,1.675,0.412776);
#783=TOROIDAL_SURFACE('',#14929,1.675,0.412776);
#784=B_SPLINE_CURVE_WITH_KNOTS('',3,(#19392,#19393,#19394,#19395,#19396,
#19397,#19398,#19399,#19400,#19401),.UNSPECIFIED.,.F.,.F.,(4,2,2,2,4),(0.,
0.0944273339541119,0.188854667908224,0.283277491997423,0.377700316086621),
 .UNSPECIFIED.);
#785=B_SPLINE_CURVE_WITH_KNOTS('',3,(#19402,#19403,#19404,#19405,#19406,
#19407,#19408,#19409,#19410,#19411,#19412,#19413,#19414,#19415,#19416,#19417,
#19418,#19419,#19420,#19421,#19422,#19423,#19424,#19425,#19426,#19427),
 .UNSPECIFIED.,.F.,.F.,(4,2,2,2,2,2,2,2,2,2,2,2,4),(0.377700316086621,0.47212314017582,
0.56654596426502,0.660973298219131,0.755400632173242,0.849827966127354,
0.944255300081465,1.03867812417066,1.13310094825986,1.22752377234906,1.32194659643826,
1.41637393039237,1.51080126434648),.UNSPECIFIED.);
#786=B_SPLINE_CURVE_WITH_KNOTS('',3,(#19431,#19432,#19433,#19434,#19435,
#19436,#19437,#19438,#19439,#19440,#19441,#19442,#19443,#19444,#19445,#19446,
#19447,#19448,#19449,#19450,#19451,#19452,#19453,#19454,#19455,#19456),
 .UNSPECIFIED.,.F.,.F.,(4,2,2,2,2,2,2,2,2,2,2,2,4),(0.,0.0942593862034407,
0.188518772406881,0.282777622143722,0.377036471880563,0.471295321617403,
0.565554171354244,0.659813557557685,0.754072943761126,0.848332329964567,
0.942591716168009,1.03685056590485,1.13110941564169),.UNSPECIFIED.);
#787=B_SPLINE_CURVE_WITH_KNOTS('',3,(#19457,#19458,#19459,#19460,#19461,
#19462,#19463,#19464,#19465,#19466),.UNSPECIFIED.,.F.,.F.,(4,2,2,2,4),(1.13110941564169,
1.22536826537853,1.31962711511537,1.41388650131881,1.50814588752225),
 .UNSPECIFIED.);
#788=B_SPLINE_CURVE_WITH_KNOTS('',3,(#19722,#19723,#19724,#19725,#19726,
#19727,#19728,#19729,#19730,#19731,#19732,#19733,#19734,#19735),
 .UNSPECIFIED.,.F.,.F.,(4,2,2,2,2,2,4),(0.598759573717661,0.624973342427789,
0.687463163426142,0.749952984424494,0.812442805422847,0.874932626421199,
0.901146395131325),.UNSPECIFIED.);
#789=B_SPLINE_CURVE_WITH_KNOTS('',3,(#19739,#19740,#19741,#19742,#19743,
#19744,#19745,#19746),.UNSPECIFIED.,.F.,.F.,(4,2,2,4),(0.249984328141498,
0.31247414913985,0.374963970138203,0.401177738848332),.UNSPECIFIED.);
#790=B_SPLINE_CURVE_WITH_KNOTS('',3,(#19750,#19751,#19752,#19753,#19754,
#19755,#19756,#19757),.UNSPECIFIED.,.F.,.F.,(4,2,2,4),(0.0987909174346634,
0.125004686144793,0.187494507143146,0.249984328141498),.UNSPECIFIED.);
#791=B_SPLINE_CURVE_WITH_KNOTS('',3,(#20144,#20145,#20146,#20147,#20148,
#20149,#20150,#20151,#20152,#20153,#20154,#20155,#20156,#20157,#20158,#20159,
#20160,#20161,#20162,#20163,#20164,#20165),.UNSPECIFIED.,.F.,.F.,(4,2,2,
2,2,2,2,2,2,2,4),(0.0591825211272536,0.157966726598481,0.236950089897721,
0.315933453196962,0.391576304923761,0.46721915665056,0.54286200837736,0.618504860104159,
0.697488223403399,0.77647158670264,0.875255792173867),.UNSPECIFIED.);
#792=B_SPLINE_CURVE_WITH_KNOTS('',3,(#20169,#20170,#20171,#20172,#20173,
#20174,#20175,#20176,#20177,#20178,#20179,#20180,#20181,#20182,#20183,#20184,
#20185,#20186,#20187,#20188,#20189,#20190),.UNSPECIFIED.,.F.,.F.,(4,2,2,
2,2,2,2,2,2,2,4),(0.0581119756758434,0.106553146291161,0.213106292582322,
0.30849933801665,0.386091982889075,0.4636846277615,0.541277272633925,0.61886991750635,
0.714262962940678,0.820816109231839,0.869257279847157),.UNSPECIFIED.);
#793=B_SPLINE_CURVE_WITH_KNOTS('',3,(#20196,#20197,#20198,#20199,#20200,
#20201,#20202,#20203,#20204,#20205,#20206,#20207,#20208,#20209,#20210,#20211,
#20212,#20213,#20214,#20215,#20216,#20217),.UNSPECIFIED.,.F.,.F.,(4,2,2,
2,2,2,2,2,2,2,4),(0.0581119756758434,0.106553146291161,0.213106292582322,
0.30849933801665,0.386091982889075,0.4636846277615,0.541277272633925,0.61886991750635,
0.714262962940679,0.820816109231839,0.869257279847157),.UNSPECIFIED.);
#794=B_SPLINE_CURVE_WITH_KNOTS('',3,(#20221,#20222,#20223,#20224,#20225,
#20226,#20227,#20228,#20229,#20230,#20231,#20232,#20233,#20234,#20235,#20236,
#20237,#20238,#20239,#20240,#20241,#20242),.UNSPECIFIED.,.F.,.F.,(4,2,2,
2,2,2,2,2,2,2,4),(0.0581119756758433,0.106553146291161,0.213106292582322,
0.308499338016649,0.386091982889075,0.4636846277615,0.541277272633925,0.61886991750635,
0.714262962940678,0.820816109231839,0.869257279847157),.UNSPECIFIED.);
#795=B_SPLINE_CURVE_WITH_KNOTS('',3,(#20251,#20252,#20253,#20254,#20255,
#20256,#20257,#20258,#20259,#20260,#20261,#20262,#20263,#20264,#20265,#20266,
#20267,#20268,#20269,#20270,#20271,#20272),.UNSPECIFIED.,.F.,.F.,(4,2,2,
2,2,2,2,2,2,2,4),(0.0581119756758433,0.106553146291161,0.213106292582322,
0.30849933801665,0.386091982889075,0.4636846277615,0.541277272633925,0.61886991750635,
0.714262962940678,0.820816109231839,0.869257279847157),.UNSPECIFIED.);
#796=B_SPLINE_CURVE_WITH_KNOTS('',3,(#20276,#20277,#20278,#20279,#20280,
#20281,#20282,#20283,#20284,#20285,#20286,#20287,#20288,#20289,#20290,#20291,
#20292,#20293,#20294,#20295,#20296,#20297),.UNSPECIFIED.,.F.,.F.,(4,2,2,
2,2,2,2,2,2,2,4),(0.0581119756758434,0.106553146291161,0.213106292582322,
0.30849933801665,0.386091982889075,0.4636846277615,0.541277272633925,0.61886991750635,
0.714262962940678,0.820816109231839,0.869257279847157),.UNSPECIFIED.);
#797=B_SPLINE_CURVE_WITH_KNOTS('',3,(#20301,#20302,#20303,#20304,#20305,
#20306,#20307,#20308,#20309,#20310,#20311,#20312,#20313,#20314,#20315,#20316,
#20317,#20318,#20319,#20320,#20321,#20322),.UNSPECIFIED.,.F.,.F.,(4,2,2,
2,2,2,2,2,2,2,4),(0.0581119756758434,0.106553146291161,0.213106292582322,
0.30849933801665,0.386091982889075,0.4636846277615,0.541277272633925,0.61886991750635,
0.714262962940678,0.820816109231839,0.869257279847157),.UNSPECIFIED.);
#798=B_SPLINE_CURVE_WITH_KNOTS('',3,(#20326,#20327,#20328,#20329,#20330,
#20331,#20332,#20333,#20334,#20335,#20336,#20337,#20338,#20339,#20340,#20341,
#20342,#20343,#20344,#20345,#20346,#20347),.UNSPECIFIED.,.F.,.F.,(4,2,2,
2,2,2,2,2,2,2,4),(0.0581119756758433,0.106553146291161,0.213106292582322,
0.30849933801665,0.386091982889075,0.4636846277615,0.541277272633925,0.61886991750635,
0.714262962940678,0.820816109231839,0.869257279847157),.UNSPECIFIED.);
#799=B_SPLINE_CURVE_WITH_KNOTS('',3,(#20355,#20356,#20357,#20358,#20359,
#20360,#20361,#20362,#20363,#20364,#20365,#20366,#20367,#20368,#20369,#20370,
#20371,#20372,#20373,#20374,#20375,#20376),.UNSPECIFIED.,.F.,.F.,(4,2,2,
2,2,2,2,2,2,2,4),(0.0591825211272536,0.157966726598481,0.236950089897721,
0.315933453196962,0.391576304923761,0.467219156650561,0.54286200837736,
0.618504860104159,0.697488223403399,0.77647158670264,0.875255792173867),
 .UNSPECIFIED.);
#800=B_SPLINE_CURVE_WITH_KNOTS('',3,(#20384,#20385,#20386,#20387,#20388,
#20389,#20390,#20391,#20392,#20393,#20394,#20395,#20396,#20397,#20398,#20399,
#20400,#20401,#20402,#20403,#20404,#20405),.UNSPECIFIED.,.F.,.F.,(4,2,2,
2,2,2,2,2,2,2,4),(0.0591825211272536,0.157966726598481,0.236950089897722,
0.315933453196962,0.391576304923761,0.467219156650561,0.54286200837736,
0.618504860104159,0.697488223403399,0.77647158670264,0.875255792173867),
 .UNSPECIFIED.);
#801=B_SPLINE_CURVE_WITH_KNOTS('',3,(#20415,#20416,#20417,#20418,#20419,
#20420,#20421,#20422,#20423,#20424,#20425,#20426,#20427,#20428,#20429,#20430,
#20431,#20432,#20433,#20434,#20435,#20436),.UNSPECIFIED.,.F.,.F.,(4,2,2,
2,2,2,2,2,2,2,4),(0.0591825211272536,0.157966726598481,0.236950089897721,
0.315933453196962,0.391576304923761,0.46721915665056,0.54286200837736,0.618504860104159,
0.697488223403399,0.77647158670264,0.875255792173867),.UNSPECIFIED.);
#802=B_SPLINE_CURVE_WITH_KNOTS('',3,(#20444,#20445,#20446,#20447,#20448,
#20449,#20450,#20451,#20452,#20453,#20454,#20455,#20456,#20457,#20458,#20459,
#20460,#20461,#20462,#20463,#20464,#20465),.UNSPECIFIED.,.F.,.F.,(4,2,2,
2,2,2,2,2,2,2,4),(0.0591825211272536,0.157966726598481,0.236950089897721,
0.315933453196962,0.391576304923761,0.46721915665056,0.542862008377359,
0.618504860104159,0.697488223403399,0.776471586702639,0.875255792173867),
 .UNSPECIFIED.);
#803=B_SPLINE_CURVE_WITH_KNOTS('',3,(#20473,#20474,#20475,#20476,#20477,
#20478,#20479,#20480,#20481,#20482,#20483,#20484,#20485,#20486,#20487,#20488,
#20489,#20490,#20491,#20492,#20493,#20494),.UNSPECIFIED.,.F.,.F.,(4,2,2,
2,2,2,2,2,2,2,4),(0.0591825211272536,0.157966726598481,0.236950089897721,
0.315933453196962,0.391576304923761,0.46721915665056,0.54286200837736,0.618504860104159,
0.697488223403399,0.77647158670264,0.875255792173867),.UNSPECIFIED.);
#804=B_SPLINE_CURVE_WITH_KNOTS('',3,(#20503,#20504,#20505,#20506,#20507,
#20508,#20509,#20510,#20511,#20512,#20513,#20514,#20515,#20516,#20517,#20518,
#20519,#20520,#20521,#20522,#20523,#20524),.UNSPECIFIED.,.F.,.F.,(4,2,2,
2,2,2,2,2,2,2,4),(0.0591825211272536,0.157966726598481,0.236950089897721,
0.315933453196962,0.391576304923761,0.46721915665056,0.542862008377359,
0.618504860104159,0.697488223403399,0.776471586702639,0.875255792173867),
 .UNSPECIFIED.);
#805=B_SPLINE_CURVE_WITH_KNOTS('',3,(#20786,#20787,#20788,#20789,#20790,
#20791,#20792,#20793,#20794,#20795),.UNSPECIFIED.,.F.,.F.,(4,2,2,2,4),(0.,
0.0943388977190341,0.188677795438068,0.283014752973434,0.377351710508801),
 .UNSPECIFIED.);
#806=B_SPLINE_CURVE_WITH_KNOTS('',3,(#20796,#20797,#20798,#20799,#20800,
#20801,#20802,#20803,#20804,#20805,#20806,#20807,#20808,#20809,#20810,#20811,
#20812,#20813,#20814,#20815,#20816,#20817,#20818,#20819,#20820,#20821),
 .UNSPECIFIED.,.F.,.F.,(4,2,2,2,2,2,2,2,2,2,2,2,4),(0.377351710508801,0.471688668044167,
0.566025625579534,0.660364523298568,0.754703421017602,0.849042318736636,
0.94338121645567,1.03771817399104,1.1320551315264,1.22639208906177,1.32072904659714,
1.41506794431617,1.5094068420352),.UNSPECIFIED.);
#807=B_SPLINE_CURVE_WITH_KNOTS('',3,(#20825,#20826,#20827,#20828,#20829,
#20830,#20831,#20832,#20833,#20834,#20835,#20836,#20837,#20838,#20839,#20840,
#20841,#20842,#20843,#20844,#20845,#20846,#20847,#20848,#20849,#20850),
 .UNSPECIFIED.,.F.,.F.,(4,2,2,2,2,2,2,2,2,2,2,2,4),(0.,0.0942186410044056,
0.188437282008811,0.282655768798836,0.376874255588861,0.471092742378886,
0.565311229168911,0.659529870173316,0.753748511177722,0.847967152182128,
0.942185793186533,1.03640427997656,1.13062276676658),.UNSPECIFIED.);
#808=B_SPLINE_CURVE_WITH_KNOTS('',3,(#20851,#20852,#20853,#20854,#20855,
#20856,#20857,#20858,#20859,#20860),.UNSPECIFIED.,.F.,.F.,(4,2,2,2,4),(1.13062276676658,
1.22484125355661,1.31905974034663,1.41327838135104,1.50749702235544),
 .UNSPECIFIED.);
#809=B_SPLINE_CURVE_WITH_KNOTS('',3,(#21520,#21521,#21522,#21523,#21524,
#21525,#21526,#21527,#21528,#21529,#21530,#21531,#21532,#21533,#21534,#21535,
#21536,#21537,#21538,#21539,#21540,#21541),.UNSPECIFIED.,.F.,.F.,(4,2,2,
2,2,2,2,2,2,2,4),(0.0789094028588958,0.210573405340968,0.315860108011452,
0.421146810681936,0.522142632548711,0.623138454415485,0.72413427628226,
0.825130098149035,0.930416800819519,1.03570350349,1.16736750597208),
 .UNSPECIFIED.);
#810=B_SPLINE_CURVE_WITH_KNOTS('',3,(#21545,#21546,#21547,#21548,#21549,
#21550,#21551,#21552,#21553,#21554,#21555,#21556,#21557,#21558,#21559,#21560,
#21561,#21562,#21563,#21564,#21565,#21566),.UNSPECIFIED.,.F.,.F.,(4,2,2,
2,2,2,2,2,2,2,4),(0.0774793363974613,0.142088896491891,0.284177792983782,
0.411119756996526,0.514392970548519,0.617666184100513,0.720939397652506,
0.8242126112045,0.951154575217244,1.09324347170913,1.15785303180356),
 .UNSPECIFIED.);
#811=B_SPLINE_CURVE_WITH_KNOTS('',3,(#21572,#21573,#21574,#21575,#21576,
#21577,#21578,#21579,#21580,#21581,#21582,#21583,#21584,#21585,#21586,#21587,
#21588,#21589,#21590,#21591,#21592,#21593),.UNSPECIFIED.,.F.,.F.,(4,2,2,
2,2,2,2,2,2,2,4),(0.0774793363974613,0.142088896491891,0.284177792983782,
0.411119756996525,0.514392970548519,0.617666184100513,0.720939397652506,
0.8242126112045,0.951154575217243,1.09324347170913,1.15785303180356),
 .UNSPECIFIED.);
#812=B_SPLINE_CURVE_WITH_KNOTS('',3,(#21597,#21598,#21599,#21600,#21601,
#21602,#21603,#21604,#21605,#21606,#21607,#21608,#21609,#21610,#21611,#21612,
#21613,#21614,#21615,#21616,#21617,#21618),.UNSPECIFIED.,.F.,.F.,(4,2,2,
2,2,2,2,2,2,2,4),(0.0774793363974614,0.142088896491891,0.284177792983781,
0.411119756996525,0.514392970548519,0.617666184100512,0.720939397652506,
0.824212611204499,0.951154575217243,1.09324347170913,1.15785303180356),
 .UNSPECIFIED.);
#813=B_SPLINE_CURVE_WITH_KNOTS('',3,(#21622,#21623,#21624,#21625,#21626,
#21627,#21628,#21629,#21630,#21631,#21632,#21633),.UNSPECIFIED.,.F.,.F.,
(4,2,2,2,2,4),(0.0774793363974613,0.142088896491891,0.284177792983781,0.411119756996525,
0.514392970548519,0.617666184100512),.UNSPECIFIED.);
#814=B_SPLINE_CURVE_WITH_KNOTS('',3,(#21638,#21639,#21640,#21641,#21642,
#21643,#21644,#21645,#21646,#21647,#21648,#21649),.UNSPECIFIED.,.F.,.F.,
(4,2,2,2,2,4),(0.617666184100512,0.720939397652506,0.824212611204499,0.951154575217243,
1.09324347170913,1.15785303180356),.UNSPECIFIED.);
#815=B_SPLINE_CURVE_WITH_KNOTS('',3,(#21653,#21654,#21655,#21656,#21657,
#21658,#21659,#21660,#21661,#21662,#21663,#21664,#21665,#21666,#21667,#21668,
#21669,#21670,#21671,#21672,#21673,#21674),.UNSPECIFIED.,.F.,.F.,(4,2,2,
2,2,2,2,2,2,2,4),(0.0774793363974613,0.142088896491891,0.284177792983782,
0.411119756996526,0.514392970548519,0.617666184100513,0.720939397652507,
0.8242126112045,0.951154575217245,1.09324347170914,1.15785303180356),
 .UNSPECIFIED.);
#816=B_SPLINE_CURVE_WITH_KNOTS('',3,(#21678,#21679,#21680,#21681,#21682,
#21683,#21684,#21685,#21686,#21687,#21688,#21689,#21690,#21691,#21692,#21693,
#21694,#21695,#21696,#21697,#21698,#21699),.UNSPECIFIED.,.F.,.F.,(4,2,2,
2,2,2,2,2,2,2,4),(0.0774793363974613,0.142088896491891,0.284177792983782,
0.411119756996526,0.514392970548519,0.617666184100513,0.720939397652506,
0.824212611204499,0.951154575217243,1.09324347170913,1.15785303180356),
 .UNSPECIFIED.);
#817=B_SPLINE_CURVE_WITH_KNOTS('',3,(#21703,#21704,#21705,#21706,#21707,
#21708,#21709,#21710,#21711,#21712,#21713,#21714,#21715,#21716,#21717,#21718,
#21719,#21720,#21721,#21722,#21723,#21724),.UNSPECIFIED.,.F.,.F.,(4,2,2,
2,2,2,2,2,2,2,4),(0.0774793363974613,0.142088896491891,0.284177792983782,
0.411119756996526,0.514392970548519,0.617666184100513,0.720939397652506,
0.8242126112045,0.951154575217244,1.09324347170913,1.15785303180356),
 .UNSPECIFIED.);
#818=B_SPLINE_CURVE_WITH_KNOTS('',3,(#21728,#21729,#21730,#21731,#21732,
#21733,#21734,#21735,#21736,#21737,#21738,#21739,#21740,#21741,#21742,#21743,
#21744,#21745,#21746,#21747,#21748,#21749),.UNSPECIFIED.,.F.,.F.,(4,2,2,
2,2,2,2,2,2,2,4),(0.0774793363974613,0.142088896491891,0.284177792983782,
0.411119756996526,0.514392970548519,0.617666184100513,0.720939397652506,
0.8242126112045,0.951154575217243,1.09324347170913,1.15785303180356),
 .UNSPECIFIED.);
#819=B_SPLINE_CURVE_WITH_KNOTS('',3,(#21757,#21758,#21759,#21760,#21761,
#21762,#21763,#21764,#21765,#21766,#21767,#21768,#21769,#21770,#21771,#21772,
#21773,#21774,#21775,#21776,#21777,#21778),.UNSPECIFIED.,.F.,.F.,(4,2,2,
2,2,2,2,2,2,2,4),(0.0789094028588958,0.210573405340968,0.315860108011452,
0.421146810681936,0.522142632548711,0.623138454415485,0.72413427628226,
0.825130098149035,0.930416800819519,1.03570350349,1.16736750597208),
 .UNSPECIFIED.);
#820=B_SPLINE_CURVE_WITH_KNOTS('',3,(#21786,#21787,#21788,#21789,#21790,
#21791,#21792,#21793,#21794,#21795,#21796,#21797,#21798,#21799,#21800,#21801,
#21802,#21803,#21804,#21805,#21806,#21807),.UNSPECIFIED.,.F.,.F.,(4,2,2,
2,2,2,2,2,2,2,4),(0.0789094028588958,0.210573405340969,0.315860108011453,
0.421146810681937,0.522142632548712,0.623138454415486,0.724134276282261,
0.825130098149035,0.930416800819519,1.03570350349,1.16736750597208),
 .UNSPECIFIED.);
#821=B_SPLINE_CURVE_WITH_KNOTS('',3,(#21816,#21817,#21818,#21819,#21820,
#21821,#21822,#21823,#21824,#21825,#21826,#21827),.UNSPECIFIED.,.F.,.F.,
(4,2,2,2,2,4),(0.0789094028588958,0.210573405340968,0.315860108011452,0.421146810681937,
0.522142632548711,0.623138454415486),.UNSPECIFIED.);
#822=B_SPLINE_CURVE_WITH_KNOTS('',3,(#21829,#21830,#21831,#21832,#21833,
#21834,#21835,#21836,#21837,#21838,#21839,#21840),.UNSPECIFIED.,.F.,.F.,
(4,2,2,2,2,4),(0.623138454415486,0.72413427628226,0.825130098149035,0.930416800819519,
1.03570350349,1.16736750597208),.UNSPECIFIED.);
#823=B_SPLINE_CURVE_WITH_KNOTS('',3,(#21847,#21848,#21849,#21850,#21851,
#21852,#21853,#21854,#21855,#21856,#21857,#21858,#21859,#21860,#21861,#21862,
#21863,#21864,#21865,#21866,#21867,#21868),.UNSPECIFIED.,.F.,.F.,(4,2,2,
2,2,2,2,2,2,2,4),(0.0789094028588958,0.210573405340968,0.315860108011452,
0.421146810681936,0.522142632548711,0.623138454415486,0.72413427628226,
0.825130098149035,0.930416800819519,1.03570350349,1.16736750597208),
 .UNSPECIFIED.);
#824=B_SPLINE_CURVE_WITH_KNOTS('',3,(#21876,#21877,#21878,#21879,#21880,
#21881,#21882,#21883,#21884,#21885,#21886,#21887,#21888,#21889,#21890,#21891,
#21892,#21893,#21894,#21895,#21896,#21897),.UNSPECIFIED.,.F.,.F.,(4,2,2,
2,2,2,2,2,2,2,4),(0.0789094028588957,0.210573405340968,0.315860108011452,
0.421146810681936,0.522142632548711,0.623138454415485,0.72413427628226,
0.825130098149035,0.930416800819519,1.03570350349,1.16736750597207),
 .UNSPECIFIED.);
#825=B_SPLINE_CURVE_WITH_KNOTS('',3,(#21905,#21906,#21907,#21908,#21909,
#21910,#21911,#21912,#21913,#21914,#21915,#21916,#21917,#21918,#21919,#21920,
#21921,#21922,#21923,#21924,#21925,#21926),.UNSPECIFIED.,.F.,.F.,(4,2,2,
2,2,2,2,2,2,2,4),(0.0789094028588958,0.210573405340968,0.315860108011452,
0.421146810681936,0.522142632548711,0.623138454415486,0.72413427628226,
0.825130098149035,0.930416800819519,1.03570350349,1.16736750597208),
 .UNSPECIFIED.);
#826=B_SPLINE_CURVE_WITH_KNOTS('',3,(#21935,#21936,#21937,#21938,#21939,
#21940,#21941,#21942,#21943,#21944,#21945,#21946,#21947,#21948,#21949,#21950,
#21951,#21952,#21953,#21954,#21955,#21956),.UNSPECIFIED.,.F.,.F.,(4,2,2,
2,2,2,2,2,2,2,4),(0.0789094028588958,0.210573405340968,0.315860108011452,
0.421146810681936,0.522142632548711,0.623138454415485,0.72413427628226,
0.825130098149035,0.930416800819519,1.03570350349,1.16736750597208),
 .UNSPECIFIED.);
#827=B_SPLINE_CURVE_WITH_KNOTS('',3,(#22118,#22119,#22120,#22121,#22122,
#22123,#22124,#22125,#22126,#22127,#22128,#22129,#22130,#22131),
 .UNSPECIFIED.,.F.,.F.,(4,2,2,2,2,2,4),(0.598759573717655,0.624973342427791,
0.687463163426144,0.749952984424497,0.812442805422849,0.874932626421202,
0.901146395131338),.UNSPECIFIED.);
#828=B_SPLINE_CURVE_WITH_KNOTS('',3,(#22135,#22136,#22137,#22138,#22139,
#22140,#22141,#22142),.UNSPECIFIED.,.F.,.F.,(4,2,2,4),(0.249984328141499,
0.312474149139851,0.374963970138204,0.40117773884834),.UNSPECIFIED.);
#829=B_SPLINE_CURVE_WITH_KNOTS('',3,(#22144,#22145,#22146,#22147,#22148,
#22149),.UNSPECIFIED.,.F.,.F.,(4,2,4),(0.441257277248191,0.497904393396855,
0.554551509545519),.UNSPECIFIED.);
#830=B_SPLINE_CURVE_WITH_KNOTS('',3,(#22150,#22151,#22152,#22153,#22154,
#22155,#22156),.UNSPECIFIED.,.F.,.F.,(4,3,4),(-0.0566471161400152,0.,0.0566471161486645),
 .UNSPECIFIED.);
#831=B_SPLINE_CURVE_WITH_KNOTS('',3,(#22157,#22158,#22159,#22160,#22161,
#22162,#22163,#22164),.UNSPECIFIED.,.F.,.F.,(4,2,2,4),(0.0987909174346573,
0.125004686144794,0.187494507143146,0.249984328141499),.UNSPECIFIED.);
#832=B_SPLINE_CURVE_WITH_KNOTS('',3,(#33907,#33908,#33909,#33910,#33911,
#33912,#33913,#33914,#33915,#33916),.UNSPECIFIED.,.F.,.F.,(4,2,2,2,4),(0.,
0.0622753849594661,0.124550769918932,0.186824589898798,0.249098409878664),
 .UNSPECIFIED.);
#833=B_SPLINE_CURVE_WITH_KNOTS('',3,(#33917,#33918,#33919,#33920,#33921,
#33922,#33923,#33924,#33925,#33926,#33927,#33928,#33929,#33930,#33931,#33932,
#33933,#33934,#33935,#33936,#33937,#33938,#33939,#33940,#33941,#33942),
 .UNSPECIFIED.,.F.,.F.,(4,2,2,2,2,2,2,2,2,2,2,2,4),(0.249098409878664,0.31137222985853,
0.373646049838396,0.435921434797862,0.498196819757329,0.560472204716795,
0.622747589676261,0.685021409656127,0.747295229635993,0.809569049615859,
0.871842869595725,0.934118254555191,0.996393639514657),.UNSPECIFIED.);
#834=B_SPLINE_CURVE_WITH_KNOTS('',3,(#33946,#33947,#33948,#33949,#33950,
#33951,#33952,#33953,#33954,#33955,#33956,#33957,#33958,#33959,#33960,#33961,
#33962,#33963,#33964,#33965,#33966,#33967,#33968,#33969,#33970,#33971),
 .UNSPECIFIED.,.F.,.F.,(4,2,2,2,2,2,2,2,2,2,2,2,4),(0.,0.0622075173149515,
0.124415034629903,0.186622241324509,0.248829448019115,0.311036654713721,
0.373243861408327,0.435451378723279,0.49765889603823,0.559866413353181,
0.622073930668133,0.684281137362739,0.746488344057345),.UNSPECIFIED.);
#835=B_SPLINE_CURVE_WITH_KNOTS('',3,(#33972,#33973,#33974,#33975,#33976,
#33977,#33978,#33979,#33980,#33981),.UNSPECIFIED.,.F.,.F.,(4,2,2,2,4),(0.746488344057345,
0.808695550751951,0.870902757446557,0.933110274761508,0.99531779207646),
 .UNSPECIFIED.);
#836=B_SPLINE_CURVE_WITH_KNOTS('',3,(#40102,#40103,#40104,#40105,#40106,
#40107),.UNSPECIFIED.,.F.,.F.,(4,2,4),(0.,1.,2.),.UNSPECIFIED.);
#837=B_SPLINE_CURVE_WITH_KNOTS('',3,(#40321,#40322,#40323,#40324,#40325,
#40326),.UNSPECIFIED.,.F.,.F.,(4,2,4),(0.,1.,2.),.UNSPECIFIED.);
#838=B_SPLINE_CURVE_WITH_KNOTS('',3,(#40404,#40405,#40406,#40407,#40408,
#40409),.UNSPECIFIED.,.F.,.F.,(4,2,4),(0.,1.,2.),.UNSPECIFIED.);
#839=B_SPLINE_CURVE_WITH_KNOTS('',3,(#40763,#40764,#40765,#40766,#40767,
#40768),.UNSPECIFIED.,.F.,.F.,(4,2,4),(0.,1.,2.),.UNSPECIFIED.);
#840=B_SPLINE_CURVE_WITH_KNOTS('',3,(#40846,#40847,#40848,#40849,#40850,
#40851),.UNSPECIFIED.,.F.,.F.,(4,2,4),(0.,1.,2.),.UNSPECIFIED.);
#841=B_SPLINE_CURVE_WITH_KNOTS('',3,(#41205,#41206,#41207,#41208,#41209,
#41210),.UNSPECIFIED.,.F.,.F.,(4,2,4),(0.,1.,2.),.UNSPECIFIED.);
#842=B_SPLINE_CURVE_WITH_KNOTS('',3,(#41288,#41289,#41290,#41291,#41292,
#41293),.UNSPECIFIED.,.F.,.F.,(4,2,4),(0.,1.,2.),.UNSPECIFIED.);
#843=B_SPLINE_CURVE_WITH_KNOTS('',3,(#41647,#41648,#41649,#41650,#41651,
#41652),.UNSPECIFIED.,.F.,.F.,(4,2,4),(0.,1.,2.),.UNSPECIFIED.);
#844=B_SPLINE_CURVE_WITH_KNOTS('',3,(#41730,#41731,#41732,#41733,#41734,
#41735),.UNSPECIFIED.,.F.,.F.,(4,2,4),(0.,1.,2.),.UNSPECIFIED.);
#845=B_SPLINE_CURVE_WITH_KNOTS('',3,(#42089,#42090,#42091,#42092,#42093,
#42094),.UNSPECIFIED.,.F.,.F.,(4,2,4),(0.,1.,2.),.UNSPECIFIED.);
#846=B_SPLINE_CURVE_WITH_KNOTS('',3,(#42172,#42173,#42174,#42175,#42176,
#42177),.UNSPECIFIED.,.F.,.F.,(4,2,4),(0.,1.,2.),.UNSPECIFIED.);
#847=B_SPLINE_CURVE_WITH_KNOTS('',3,(#42531,#42532,#42533,#42534,#42535,
#42536),.UNSPECIFIED.,.F.,.F.,(4,2,4),(0.,1.,2.),.UNSPECIFIED.);
#848=B_SPLINE_CURVE_WITH_KNOTS('',3,(#42614,#42615,#42616,#42617,#42618,
#42619),.UNSPECIFIED.,.F.,.F.,(4,2,4),(0.,1.,2.),.UNSPECIFIED.);
#849=B_SPLINE_CURVE_WITH_KNOTS('',3,(#42973,#42974,#42975,#42976,#42977,
#42978),.UNSPECIFIED.,.F.,.F.,(4,2,4),(0.,1.,2.),.UNSPECIFIED.);
#850=B_SPLINE_CURVE_WITH_KNOTS('',3,(#43056,#43057,#43058,#43059,#43060,
#43061),.UNSPECIFIED.,.F.,.F.,(4,2,4),(0.,1.,2.),.UNSPECIFIED.);
#851=B_SPLINE_CURVE_WITH_KNOTS('',3,(#43415,#43416,#43417,#43418,#43419,
#43420),.UNSPECIFIED.,.F.,.F.,(4,2,4),(0.,1.,2.),.UNSPECIFIED.);
#852=B_SPLINE_CURVE_WITH_KNOTS('',3,(#43498,#43499,#43500,#43501,#43502,
#43503),.UNSPECIFIED.,.F.,.F.,(4,2,4),(0.,1.,2.),.UNSPECIFIED.);
#853=B_SPLINE_CURVE_WITH_KNOTS('',3,(#43857,#43858,#43859,#43860,#43861,
#43862),.UNSPECIFIED.,.F.,.F.,(4,2,4),(0.,1.,2.),.UNSPECIFIED.);
#854=B_SPLINE_CURVE_WITH_KNOTS('',3,(#43940,#43941,#43942,#43943,#43944,
#43945),.UNSPECIFIED.,.F.,.F.,(4,2,4),(0.,1.,2.),.UNSPECIFIED.);
#855=B_SPLINE_CURVE_WITH_KNOTS('',3,(#44299,#44300,#44301,#44302,#44303,
#44304),.UNSPECIFIED.,.F.,.F.,(4,2,4),(0.,1.,2.),.UNSPECIFIED.);
#856=B_SPLINE_CURVE_WITH_KNOTS('',3,(#44382,#44383,#44384,#44385,#44386,
#44387),.UNSPECIFIED.,.F.,.F.,(4,2,4),(0.,1.,2.),.UNSPECIFIED.);
#857=B_SPLINE_CURVE_WITH_KNOTS('',3,(#44741,#44742,#44743,#44744,#44745,
#44746),.UNSPECIFIED.,.F.,.F.,(4,2,4),(0.,1.,2.),.UNSPECIFIED.);
#858=B_SPLINE_CURVE_WITH_KNOTS('',3,(#44824,#44825,#44826,#44827,#44828,
#44829),.UNSPECIFIED.,.F.,.F.,(4,2,4),(0.,1.,2.),.UNSPECIFIED.);
#859=B_SPLINE_CURVE_WITH_KNOTS('',3,(#45183,#45184,#45185,#45186,#45187,
#45188),.UNSPECIFIED.,.F.,.F.,(4,2,4),(0.,1.,2.),.UNSPECIFIED.);
#860=B_SPLINE_CURVE_WITH_KNOTS('',3,(#45266,#45267,#45268,#45269,#45270,
#45271),.UNSPECIFIED.,.F.,.F.,(4,2,4),(0.,1.,2.),.UNSPECIFIED.);
#861=B_SPLINE_CURVE_WITH_KNOTS('',3,(#45625,#45626,#45627,#45628,#45629,
#45630),.UNSPECIFIED.,.F.,.F.,(4,2,4),(0.,1.,2.),.UNSPECIFIED.);
#862=B_SPLINE_CURVE_WITH_KNOTS('',3,(#45708,#45709,#45710,#45711,#45712,
#45713),.UNSPECIFIED.,.F.,.F.,(4,2,4),(0.,1.,2.),.UNSPECIFIED.);
#863=B_SPLINE_CURVE_WITH_KNOTS('',3,(#46067,#46068,#46069,#46070,#46071,
#46072),.UNSPECIFIED.,.F.,.F.,(4,2,4),(0.,1.,2.),.UNSPECIFIED.);
#864=B_SPLINE_CURVE_WITH_KNOTS('',3,(#46150,#46151,#46152,#46153,#46154,
#46155),.UNSPECIFIED.,.F.,.F.,(4,2,4),(0.,1.,2.),.UNSPECIFIED.);
#865=B_SPLINE_CURVE_WITH_KNOTS('',3,(#46509,#46510,#46511,#46512,#46513,
#46514),.UNSPECIFIED.,.F.,.F.,(4,2,4),(0.,1.,2.),.UNSPECIFIED.);
#866=B_SPLINE_CURVE_WITH_KNOTS('',3,(#46592,#46593,#46594,#46595,#46596,
#46597),.UNSPECIFIED.,.F.,.F.,(4,2,4),(0.,1.,2.),.UNSPECIFIED.);
#867=B_SPLINE_CURVE_WITH_KNOTS('',3,(#46951,#46952,#46953,#46954,#46955,
#46956),.UNSPECIFIED.,.F.,.F.,(4,2,4),(0.,1.,2.),.UNSPECIFIED.);
#868=B_SPLINE_CURVE_WITH_KNOTS('',3,(#47034,#47035,#47036,#47037,#47038,
#47039),.UNSPECIFIED.,.F.,.F.,(4,2,4),(0.,1.,2.),.UNSPECIFIED.);
#869=B_SPLINE_CURVE_WITH_KNOTS('',3,(#47393,#47394,#47395,#47396,#47397,
#47398),.UNSPECIFIED.,.F.,.F.,(4,2,4),(0.,1.,2.),.UNSPECIFIED.);
#870=B_SPLINE_CURVE_WITH_KNOTS('',3,(#47476,#47477,#47478,#47479,#47480,
#47481),.UNSPECIFIED.,.F.,.F.,(4,2,4),(0.,1.,2.),.UNSPECIFIED.);
#871=B_SPLINE_CURVE_WITH_KNOTS('',3,(#47835,#47836,#47837,#47838,#47839,
#47840),.UNSPECIFIED.,.F.,.F.,(4,2,4),(0.,1.,2.),.UNSPECIFIED.);
#872=B_SPLINE_CURVE_WITH_KNOTS('',3,(#47918,#47919,#47920,#47921,#47922,
#47923),.UNSPECIFIED.,.F.,.F.,(4,2,4),(0.,1.,2.),.UNSPECIFIED.);
#873=B_SPLINE_CURVE_WITH_KNOTS('',3,(#48277,#48278,#48279,#48280,#48281,
#48282),.UNSPECIFIED.,.F.,.F.,(4,2,4),(0.,1.,2.),.UNSPECIFIED.);
#874=B_SPLINE_CURVE_WITH_KNOTS('',3,(#48360,#48361,#48362,#48363,#48364,
#48365),.UNSPECIFIED.,.F.,.F.,(4,2,4),(0.,1.,2.),.UNSPECIFIED.);
#875=B_SPLINE_CURVE_WITH_KNOTS('',3,(#48719,#48720,#48721,#48722,#48723,
#48724),.UNSPECIFIED.,.F.,.F.,(4,2,4),(0.,1.,2.),.UNSPECIFIED.);
#876=B_SPLINE_CURVE_WITH_KNOTS('',3,(#48802,#48803,#48804,#48805,#48806,
#48807),.UNSPECIFIED.,.F.,.F.,(4,2,4),(0.,1.,2.),.UNSPECIFIED.);
#877=B_SPLINE_CURVE_WITH_KNOTS('',3,(#49161,#49162,#49163,#49164,#49165,
#49166),.UNSPECIFIED.,.F.,.F.,(4,2,4),(0.,1.,2.),.UNSPECIFIED.);
#878=B_SPLINE_CURVE_WITH_KNOTS('',3,(#49244,#49245,#49246,#49247,#49248,
#49249),.UNSPECIFIED.,.F.,.F.,(4,2,4),(0.,1.,2.),.UNSPECIFIED.);
#879=B_SPLINE_CURVE_WITH_KNOTS('',3,(#49603,#49604,#49605,#49606,#49607,
#49608),.UNSPECIFIED.,.F.,.F.,(4,2,4),(0.,1.,2.),.UNSPECIFIED.);
#880=B_SPLINE_CURVE_WITH_KNOTS('',3,(#49686,#49687,#49688,#49689,#49690,
#49691),.UNSPECIFIED.,.F.,.F.,(4,2,4),(0.,1.,2.),.UNSPECIFIED.);
#881=B_SPLINE_CURVE_WITH_KNOTS('',3,(#50045,#50046,#50047,#50048,#50049,
#50050),.UNSPECIFIED.,.F.,.F.,(4,2,4),(0.,1.,2.),.UNSPECIFIED.);
#882=B_SPLINE_CURVE_WITH_KNOTS('',3,(#50128,#50129,#50130,#50131,#50132,
#50133),.UNSPECIFIED.,.F.,.F.,(4,2,4),(0.,1.,2.),.UNSPECIFIED.);
#883=B_SPLINE_CURVE_WITH_KNOTS('',3,(#50487,#50488,#50489,#50490,#50491,
#50492),.UNSPECIFIED.,.F.,.F.,(4,2,4),(0.,1.,2.),.UNSPECIFIED.);
#884=B_SPLINE_CURVE_WITH_KNOTS('',3,(#50570,#50571,#50572,#50573,#50574,
#50575),.UNSPECIFIED.,.F.,.F.,(4,2,4),(0.,1.,2.),.UNSPECIFIED.);
#885=B_SPLINE_CURVE_WITH_KNOTS('',3,(#50929,#50930,#50931,#50932,#50933,
#50934),.UNSPECIFIED.,.F.,.F.,(4,2,4),(0.,1.,2.),.UNSPECIFIED.);
#886=B_SPLINE_CURVE_WITH_KNOTS('',3,(#51012,#51013,#51014,#51015,#51016,
#51017),.UNSPECIFIED.,.F.,.F.,(4,2,4),(0.,1.,2.),.UNSPECIFIED.);
#887=B_SPLINE_CURVE_WITH_KNOTS('',3,(#51371,#51372,#51373,#51374,#51375,
#51376),.UNSPECIFIED.,.F.,.F.,(4,2,4),(0.,1.,2.),.UNSPECIFIED.);
#888=B_SPLINE_CURVE_WITH_KNOTS('',3,(#51454,#51455,#51456,#51457,#51458,
#51459),.UNSPECIFIED.,.F.,.F.,(4,2,4),(0.,1.,2.),.UNSPECIFIED.);
#889=B_SPLINE_CURVE_WITH_KNOTS('',3,(#51813,#51814,#51815,#51816,#51817,
#51818),.UNSPECIFIED.,.F.,.F.,(4,2,4),(0.,1.,2.),.UNSPECIFIED.);
#890=B_SPLINE_CURVE_WITH_KNOTS('',3,(#51896,#51897,#51898,#51899,#51900,
#51901),.UNSPECIFIED.,.F.,.F.,(4,2,4),(0.,1.,2.),.UNSPECIFIED.);
#891=B_SPLINE_CURVE_WITH_KNOTS('',3,(#52255,#52256,#52257,#52258,#52259,
#52260),.UNSPECIFIED.,.F.,.F.,(4,2,4),(0.,1.,2.),.UNSPECIFIED.);
#892=B_SPLINE_CURVE_WITH_KNOTS('',3,(#52338,#52339,#52340,#52341,#52342,
#52343),.UNSPECIFIED.,.F.,.F.,(4,2,4),(0.,1.,2.),.UNSPECIFIED.);
#893=B_SPLINE_CURVE_WITH_KNOTS('',3,(#52697,#52698,#52699,#52700,#52701,
#52702),.UNSPECIFIED.,.F.,.F.,(4,2,4),(0.,1.,2.),.UNSPECIFIED.);
#894=B_SPLINE_CURVE_WITH_KNOTS('',3,(#52780,#52781,#52782,#52783,#52784,
#52785),.UNSPECIFIED.,.F.,.F.,(4,2,4),(0.,1.,2.),.UNSPECIFIED.);
#895=B_SPLINE_CURVE_WITH_KNOTS('',3,(#53139,#53140,#53141,#53142,#53143,
#53144),.UNSPECIFIED.,.F.,.F.,(4,2,4),(0.,1.,2.),.UNSPECIFIED.);
#896=B_SPLINE_CURVE_WITH_KNOTS('',3,(#53222,#53223,#53224,#53225,#53226,
#53227),.UNSPECIFIED.,.F.,.F.,(4,2,4),(0.,1.,2.),.UNSPECIFIED.);
#897=B_SPLINE_CURVE_WITH_KNOTS('',3,(#53581,#53582,#53583,#53584,#53585,
#53586),.UNSPECIFIED.,.F.,.F.,(4,2,4),(0.,1.,2.),.UNSPECIFIED.);
#898=B_SPLINE_CURVE_WITH_KNOTS('',3,(#53664,#53665,#53666,#53667,#53668,
#53669),.UNSPECIFIED.,.F.,.F.,(4,2,4),(0.,1.,2.),.UNSPECIFIED.);
#899=B_SPLINE_CURVE_WITH_KNOTS('',3,(#54023,#54024,#54025,#54026,#54027,
#54028),.UNSPECIFIED.,.F.,.F.,(4,2,4),(0.,1.,2.),.UNSPECIFIED.);
#900=B_SPLINE_CURVE_WITH_KNOTS('',3,(#54106,#54107,#54108,#54109,#54110,
#54111),.UNSPECIFIED.,.F.,.F.,(4,2,4),(0.,1.,2.),.UNSPECIFIED.);
#901=B_SPLINE_CURVE_WITH_KNOTS('',3,(#54465,#54466,#54467,#54468,#54469,
#54470),.UNSPECIFIED.,.F.,.F.,(4,2,4),(0.,1.,2.),.UNSPECIFIED.);
#902=B_SPLINE_CURVE_WITH_KNOTS('',3,(#54548,#54549,#54550,#54551,#54552,
#54553),.UNSPECIFIED.,.F.,.F.,(4,2,4),(0.,1.,2.),.UNSPECIFIED.);
#903=B_SPLINE_CURVE_WITH_KNOTS('',3,(#54907,#54908,#54909,#54910,#54911,
#54912),.UNSPECIFIED.,.F.,.F.,(4,2,4),(0.,1.,2.),.UNSPECIFIED.);
#904=B_SPLINE_CURVE_WITH_KNOTS('',3,(#54990,#54991,#54992,#54993,#54994,
#54995),.UNSPECIFIED.,.F.,.F.,(4,2,4),(0.,1.,2.),.UNSPECIFIED.);
#905=B_SPLINE_CURVE_WITH_KNOTS('',3,(#55349,#55350,#55351,#55352,#55353,
#55354),.UNSPECIFIED.,.F.,.F.,(4,2,4),(0.,1.,2.),.UNSPECIFIED.);
#906=B_SPLINE_CURVE_WITH_KNOTS('',3,(#55432,#55433,#55434,#55435,#55436,
#55437),.UNSPECIFIED.,.F.,.F.,(4,2,4),(0.,1.,2.),.UNSPECIFIED.);
#907=B_SPLINE_CURVE_WITH_KNOTS('',3,(#55791,#55792,#55793,#55794,#55795,
#55796),.UNSPECIFIED.,.F.,.F.,(4,2,4),(0.,1.,2.),.UNSPECIFIED.);
#908=B_SPLINE_CURVE_WITH_KNOTS('',3,(#55874,#55875,#55876,#55877,#55878,
#55879),.UNSPECIFIED.,.F.,.F.,(4,2,4),(0.,1.,2.),.UNSPECIFIED.);
#909=B_SPLINE_CURVE_WITH_KNOTS('',3,(#56233,#56234,#56235,#56236,#56237,
#56238),.UNSPECIFIED.,.F.,.F.,(4,2,4),(0.,1.,2.),.UNSPECIFIED.);
#910=B_SPLINE_CURVE_WITH_KNOTS('',3,(#56316,#56317,#56318,#56319,#56320,
#56321),.UNSPECIFIED.,.F.,.F.,(4,2,4),(0.,1.,2.),.UNSPECIFIED.);
#911=B_SPLINE_CURVE_WITH_KNOTS('',3,(#56675,#56676,#56677,#56678,#56679,
#56680),.UNSPECIFIED.,.F.,.F.,(4,2,4),(0.,1.,2.),.UNSPECIFIED.);
#912=B_SPLINE_CURVE_WITH_KNOTS('',3,(#56758,#56759,#56760,#56761,#56762,
#56763),.UNSPECIFIED.,.F.,.F.,(4,2,4),(0.,1.,2.),.UNSPECIFIED.);
#913=B_SPLINE_CURVE_WITH_KNOTS('',3,(#57121,#57122,#57123,#57124,#57125,
#57126),.UNSPECIFIED.,.F.,.F.,(4,2,4),(0.,1.,2.),.UNSPECIFIED.);
#914=B_SPLINE_CURVE_WITH_KNOTS('',3,(#57200,#57201,#57202,#57203,#57204,
#57205),.UNSPECIFIED.,.F.,.F.,(4,2,4),(0.,1.,2.),.UNSPECIFIED.);
#915=B_SPLINE_CURVE_WITH_KNOTS('',3,(#57347,#57348,#57349,#57350,#57351,
#57352),.UNSPECIFIED.,.F.,.F.,(4,2,4),(0.,1.,2.),.UNSPECIFIED.);
#916=SHAPE_REPRESENTATION_RELATIONSHIP('SRR','None',#58111,#966);
#917=SHAPE_REPRESENTATION_RELATIONSHIP('SRR','None',#58112,#967);
#918=SHAPE_REPRESENTATION_RELATIONSHIP('SRR','None',#58113,#968);
#919=SHAPE_REPRESENTATION_RELATIONSHIP('SRR','None',#58114,#969);
#920=SHAPE_REPRESENTATION_RELATIONSHIP('SRR','None',#58115,#970);
#921=SHAPE_REPRESENTATION_RELATIONSHIP('SRR','None',#58116,#971);
#922=SHAPE_REPRESENTATION_RELATIONSHIP('SRR','None',#58117,#972);
#923=SHAPE_REPRESENTATION_RELATIONSHIP('SRR','None',#58118,#973);
#924=SHAPE_REPRESENTATION_RELATIONSHIP('SRR','None',#58119,#974);
#925=SHAPE_REPRESENTATION_RELATIONSHIP('SRR','None',#58120,#975);
#926=SHAPE_REPRESENTATION_RELATIONSHIP('SRR','None',#58121,#976);
#927=SHAPE_REPRESENTATION_RELATIONSHIP('SRR','None',#58122,#977);
#928=SHAPE_REPRESENTATION_RELATIONSHIP('SRR','None',#58124,#978);
#929=SHAPE_REPRESENTATION_RELATIONSHIP('SRR','None',#58125,#979);
#930=SHAPE_REPRESENTATION_RELATIONSHIP('SRR','None',#58126,#980);
#931=SHAPE_REPRESENTATION_RELATIONSHIP('SRR','None',#58127,#981);
#932=SHAPE_REPRESENTATION_RELATIONSHIP('SRR','None',#58128,#982);
#933=SHAPE_REPRESENTATION_RELATIONSHIP('SRR','None',#58129,#983);
#934=SHAPE_REPRESENTATION_RELATIONSHIP('SRR','None',#58131,#984);
#935=SHAPE_REPRESENTATION_RELATIONSHIP('SRR','None',#58132,#985);
#936=SHAPE_REPRESENTATION_RELATIONSHIP('SRR','None',#58133,#986);
#937=SHAPE_REPRESENTATION_RELATIONSHIP('SRR','None',#58134,#987);
#938=SHAPE_REPRESENTATION_RELATIONSHIP('SRR','None',#58135,#988);
#939=SHAPE_REPRESENTATION_RELATIONSHIP('SRR','None',#58137,#989);
#940=SHAPE_REPRESENTATION_RELATIONSHIP('SRR','None',#58138,#990);
#941=SHAPE_REPRESENTATION_RELATIONSHIP('SRR','None',#58139,#991);
#942=SHAPE_REPRESENTATION_RELATIONSHIP('SRR','None',#58140,#992);
#943=SHAPE_REPRESENTATION_RELATIONSHIP('SRR','None',#58141,#993);
#944=SHAPE_REPRESENTATION_RELATIONSHIP('SRR','None',#58143,#994);
#945=SHAPE_REPRESENTATION_RELATIONSHIP('SRR','None',#58144,#995);
#946=SHAPE_REPRESENTATION_RELATIONSHIP('SRR','None',#58145,#996);
#947=SHAPE_REPRESENTATION_RELATIONSHIP('SRR','None',#58146,#997);
#948=SHAPE_REPRESENTATION_RELATIONSHIP('SRR','None',#58147,#998);
#949=SHAPE_REPRESENTATION_RELATIONSHIP('SRR','None',#58149,#999);
#950=SHAPE_REPRESENTATION_RELATIONSHIP('SRR','None',#58150,#1000);
#951=SHAPE_REPRESENTATION_RELATIONSHIP('SRR','None',#58151,#1001);
#952=SHAPE_REPRESENTATION_RELATIONSHIP('SRR','None',#58152,#1002);
#953=SHAPE_REPRESENTATION_RELATIONSHIP('SRR','None',#58153,#1003);
#954=SHAPE_REPRESENTATION_RELATIONSHIP('SRR','None',#58154,#1004);
#955=SHAPE_REPRESENTATION_RELATIONSHIP('SRR','None',#58155,#1005);
#956=SHAPE_REPRESENTATION_RELATIONSHIP('SRR','None',#58156,#1006);
#957=SHAPE_REPRESENTATION_RELATIONSHIP('SRR','None',#58158,#1007);
#958=SHAPE_REPRESENTATION_RELATIONSHIP('SRR','None',#58159,#1008);
#959=SHAPE_REPRESENTATION_RELATIONSHIP('SRR','None',#58160,#1009);
#960=SHAPE_REPRESENTATION_RELATIONSHIP('SRR','None',#58161,#1010);
#961=SHAPE_REPRESENTATION_RELATIONSHIP('SRR','None',#58162,#1011);
#962=SHAPE_REPRESENTATION_RELATIONSHIP('SRR','None',#58163,#1012);
#963=SHAPE_REPRESENTATION_RELATIONSHIP('SRR','None',#58164,#1013);
#964=SHAPE_REPRESENTATION_RELATIONSHIP('SRR','None',#58165,#1014);
#965=SHAPE_REPRESENTATION_RELATIONSHIP('SRR','None',#58166,#1015);
#966=ADVANCED_BREP_SHAPE_REPRESENTATION('',(#1081),#57844);
#967=ADVANCED_BREP_SHAPE_REPRESENTATION('',(#1082),#57845);
#968=ADVANCED_BREP_SHAPE_REPRESENTATION('',(#1083),#57846);
#969=ADVANCED_BREP_SHAPE_REPRESENTATION('',(#1084),#57847);
#970=ADVANCED_BREP_SHAPE_REPRESENTATION('',(#1085),#57848);
#971=ADVANCED_BREP_SHAPE_REPRESENTATION('',(#1086),#57849);
#972=ADVANCED_BREP_SHAPE_REPRESENTATION('',(#1087),#57850);
#973=ADVANCED_BREP_SHAPE_REPRESENTATION('',(#1088),#57851);
#974=ADVANCED_BREP_SHAPE_REPRESENTATION('',(#1089),#57852);
#975=ADVANCED_BREP_SHAPE_REPRESENTATION('',(#1090),#57853);
#976=ADVANCED_BREP_SHAPE_REPRESENTATION('',(#1091),#57854);
#977=ADVANCED_BREP_SHAPE_REPRESENTATION('',(#1092),#57855);
#978=ADVANCED_BREP_SHAPE_REPRESENTATION('',(#1093),#57857);
#979=ADVANCED_BREP_SHAPE_REPRESENTATION('',(#1094),#57858);
#980=ADVANCED_BREP_SHAPE_REPRESENTATION('',(#1095,#1096,#1097,#1098,#1099,
#1100,#1101),#57859);
#981=ADVANCED_BREP_SHAPE_REPRESENTATION('',(#1102),#57860);
#982=ADVANCED_BREP_SHAPE_REPRESENTATION('',(#1103,#1104),#57861);
#983=ADVANCED_BREP_SHAPE_REPRESENTATION('',(#374),#57862);
#984=ADVANCED_BREP_SHAPE_REPRESENTATION('',(#1105),#57864);
#985=ADVANCED_BREP_SHAPE_REPRESENTATION('',(#1106),#57865);
#986=ADVANCED_BREP_SHAPE_REPRESENTATION('',(#1107),#57866);
#987=ADVANCED_BREP_SHAPE_REPRESENTATION('',(#1108),#57867);
#988=ADVANCED_BREP_SHAPE_REPRESENTATION('',(#1109),#57868);
#989=ADVANCED_BREP_SHAPE_REPRESENTATION('',(#1110),#57870);
#990=ADVANCED_BREP_SHAPE_REPRESENTATION('',(#1111),#57871);
#991=ADVANCED_BREP_SHAPE_REPRESENTATION('',(#1112),#57872);
#992=ADVANCED_BREP_SHAPE_REPRESENTATION('',(#1113),#57873);
#993=ADVANCED_BREP_SHAPE_REPRESENTATION('',(#375),#57874);
#994=ADVANCED_BREP_SHAPE_REPRESENTATION('',(#1114),#57876);
#995=ADVANCED_BREP_SHAPE_REPRESENTATION('',(#1115),#57877);
#996=ADVANCED_BREP_SHAPE_REPRESENTATION('',(#1116,#1117,#1118,#1119,#1120,
#1121,#1122,#1123),#57878);
#997=ADVANCED_BREP_SHAPE_REPRESENTATION('',(#1124),#57879);
#998=ADVANCED_BREP_SHAPE_REPRESENTATION('',(#1125,#1126),#57880);
#999=ADVANCED_BREP_SHAPE_REPRESENTATION('',(#1127),#57882);
#1000=ADVANCED_BREP_SHAPE_REPRESENTATION('',(#1128),#57883);
#1001=ADVANCED_BREP_SHAPE_REPRESENTATION('',(#1129),#57884);
#1002=ADVANCED_BREP_SHAPE_REPRESENTATION('',(#1130),#57885);
#1003=ADVANCED_BREP_SHAPE_REPRESENTATION('',(#1131),#57886);
#1004=ADVANCED_BREP_SHAPE_REPRESENTATION('',(#1132),#57887);
#1005=ADVANCED_BREP_SHAPE_REPRESENTATION('',(#1133),#57888);
#1006=ADVANCED_BREP_SHAPE_REPRESENTATION('',(#1134),#57889);
#1007=ADVANCED_BREP_SHAPE_REPRESENTATION('',(#1135),#57891);
#1008=ADVANCED_BREP_SHAPE_REPRESENTATION('',(#1136),#57892);
#1009=ADVANCED_BREP_SHAPE_REPRESENTATION('',(#1137),#57893);
#1010=ADVANCED_BREP_SHAPE_REPRESENTATION('',(#1138),#57894);
#1011=ADVANCED_BREP_SHAPE_REPRESENTATION('',(#1139),#57895);
#1012=ADVANCED_BREP_SHAPE_REPRESENTATION('',(#1140),#57896);
#1013=ADVANCED_BREP_SHAPE_REPRESENTATION('',(#1141),#57897);
#1014=ADVANCED_BREP_SHAPE_REPRESENTATION('',(#1142),#57898);
#1015=ADVANCED_BREP_SHAPE_REPRESENTATION('',(#376),#57899);
#1016=STYLED_ITEM('',(#58444),#1081);
#1017=STYLED_ITEM('',(#58451),#1082);
#1018=STYLED_ITEM('',(#58451),#1083);
#1019=STYLED_ITEM('',(#58465),#1084);
#1020=STYLED_ITEM('',(#58465),#1085);
#1021=STYLED_ITEM('',(#58465),#1086);
#1022=STYLED_ITEM('',(#58458),#1087);
#1023=STYLED_ITEM('',(#58451),#1088);
#1024=STYLED_ITEM('',(#58444),#1089);
#1025=STYLED_ITEM('',(#58458),#1090);
#1026=STYLED_ITEM('',(#58458),#1091);
#1027=STYLED_ITEM('',(#58458),#1092);
#1028=STYLED_ITEM('',(#58465),#1093);
#1029=STYLED_ITEM('',(#58465),#1094);
#1030=STYLED_ITEM('',(#58465),#1095);
#1031=STYLED_ITEM('',(#58465),#1096);
#1032=STYLED_ITEM('',(#58465),#1097);
#1033=STYLED_ITEM('',(#58465),#1098);
#1034=STYLED_ITEM('',(#58465),#1099);
#1035=STYLED_ITEM('',(#58465),#1100);
#1036=STYLED_ITEM('',(#58465),#1101);
#1037=STYLED_ITEM('',(#58465),#1102);
#1038=STYLED_ITEM('',(#58465),#1103);
#1039=STYLED_ITEM('',(#58465),#1104);
#1040=STYLED_ITEM('',(#58472),#374);
#1041=STYLED_ITEM('',(#58451),#1105);
#1042=STYLED_ITEM('',(#58479),#1106);
#1043=STYLED_ITEM('',(#58465),#1107);
#1044=STYLED_ITEM('',(#58465),#1108);
#1045=STYLED_ITEM('',(#58465),#1109);
#1046=STYLED_ITEM('',(#58444),#1110);
#1047=STYLED_ITEM('',(#58458),#1111);
#1048=STYLED_ITEM('',(#58479),#1112);
#1049=STYLED_ITEM('',(#58472),#1113);
#1050=STYLED_ITEM('',(#58472),#375);
#1051=STYLED_ITEM('',(#58465),#1114);
#1052=STYLED_ITEM('',(#58465),#1115);
#1053=STYLED_ITEM('',(#58465),#1116);
#1054=STYLED_ITEM('',(#58465),#1117);
#1055=STYLED_ITEM('',(#58465),#1118);
#1056=STYLED_ITEM('',(#58465),#1119);
#1057=STYLED_ITEM('',(#58465),#1120);
#1058=STYLED_ITEM('',(#58465),#1121);
#1059=STYLED_ITEM('',(#58465),#1122);
#1060=STYLED_ITEM('',(#58465),#1123);
#1061=STYLED_ITEM('',(#58465),#1124);
#1062=STYLED_ITEM('',(#58465),#1125);
#1063=STYLED_ITEM('',(#58465),#1126);
#1064=STYLED_ITEM('',(#58451),#1127);
#1065=STYLED_ITEM('',(#58458),#1128);
#1066=STYLED_ITEM('',(#58458),#1129);
#1067=STYLED_ITEM('',(#58479),#1130);
#1068=STYLED_ITEM('',(#58479),#1131);
#1069=STYLED_ITEM('',(#58465),#1132);
#1070=STYLED_ITEM('',(#58479),#1133);
#1071=STYLED_ITEM('',(#58479),#1134);
#1072=STYLED_ITEM('',(#58479),#1135);
#1073=STYLED_ITEM('',(#58479),#1136);
#1074=STYLED_ITEM('',(#58451),#1137);
#1075=STYLED_ITEM('',(#58479),#1138);
#1076=STYLED_ITEM('',(#58465),#1139);
#1077=STYLED_ITEM('',(#58479),#1140);
#1078=STYLED_ITEM('',(#58472),#1141);
#1079=STYLED_ITEM('',(#58458),#1142);
#1080=STYLED_ITEM('',(#58472),#376);
#1081=MANIFOLD_SOLID_BREP('Body1',#13576);
#1082=MANIFOLD_SOLID_BREP('Body1',#13577);
#1083=MANIFOLD_SOLID_BREP('Body1',#13578);
#1084=MANIFOLD_SOLID_BREP('Body1',#13579);
#1085=MANIFOLD_SOLID_BREP('Body1',#13580);
#1086=MANIFOLD_SOLID_BREP('Body1',#13581);
#1087=MANIFOLD_SOLID_BREP('Body1',#13582);
#1088=MANIFOLD_SOLID_BREP('Body1',#13583);
#1089=MANIFOLD_SOLID_BREP('Body1',#13584);
#1090=MANIFOLD_SOLID_BREP('Body1',#13585);
#1091=MANIFOLD_SOLID_BREP('Body1',#13586);
#1092=MANIFOLD_SOLID_BREP('Body1',#13587);
#1093=MANIFOLD_SOLID_BREP('Body1',#13588);
#1094=MANIFOLD_SOLID_BREP('Body1',#13589);
#1095=MANIFOLD_SOLID_BREP('Body1',#13590);
#1096=MANIFOLD_SOLID_BREP('Body2',#13591);
#1097=MANIFOLD_SOLID_BREP('Body3',#13592);
#1098=MANIFOLD_SOLID_BREP('Body4',#13593);
#1099=MANIFOLD_SOLID_BREP('Body5',#13594);
#1100=MANIFOLD_SOLID_BREP('Body6',#13595);
#1101=MANIFOLD_SOLID_BREP('Body7',#13596);
#1102=MANIFOLD_SOLID_BREP('Continuous crown cage',#13597);
#1103=MANIFOLD_SOLID_BREP('Body1',#13598);
#1104=MANIFOLD_SOLID_BREP('Body2',#13599);
#1105=MANIFOLD_SOLID_BREP('Body1',#13602);
#1106=MANIFOLD_SOLID_BREP('Body1',#13603);
#1107=MANIFOLD_SOLID_BREP('Body1',#13604);
#1108=MANIFOLD_SOLID_BREP('Body1',#13605);
#1109=MANIFOLD_SOLID_BREP('Body1',#13606);
#1110=MANIFOLD_SOLID_BREP('Body1',#13607);
#1111=MANIFOLD_SOLID_BREP('Body1',#13608);
#1112=MANIFOLD_SOLID_BREP('Body1',#13609);
#1113=MANIFOLD_SOLID_BREP('Body1',#13610);
#1114=MANIFOLD_SOLID_BREP('Body1',#13613);
#1115=MANIFOLD_SOLID_BREP('Body1',#13614);
#1116=MANIFOLD_SOLID_BREP('Body1',#13615);
#1117=MANIFOLD_SOLID_BREP('Body2',#13616);
#1118=MANIFOLD_SOLID_BREP('Body3',#13617);
#1119=MANIFOLD_SOLID_BREP('Body4',#13618);
#1120=MANIFOLD_SOLID_BREP('Body5',#13619);
#1121=MANIFOLD_SOLID_BREP('Body6',#13620);
#1122=MANIFOLD_SOLID_BREP('Body7',#13621);
#1123=MANIFOLD_SOLID_BREP('Body8',#13622);
#1124=MANIFOLD_SOLID_BREP('Continuous crown cage',#13623);
#1125=MANIFOLD_SOLID_BREP('Body1',#13624);
#1126=MANIFOLD_SOLID_BREP('Body2',#13625);
#1127=MANIFOLD_SOLID_BREP('Body1',#13626);
#1128=MANIFOLD_SOLID_BREP('Body1',#13627);
#1129=MANIFOLD_SOLID_BREP('Body1',#13628);
#1130=MANIFOLD_SOLID_BREP('Body1',#13629);
#1131=MANIFOLD_SOLID_BREP('Body1',#13630);
#1132=MANIFOLD_SOLID_BREP('Body1',#13631);
#1133=MANIFOLD_SOLID_BREP('Body1',#13632);
#1134=MANIFOLD_SOLID_BREP('Body1',#13633);
#1135=MANIFOLD_SOLID_BREP('Body1',#13634);
#1136=MANIFOLD_SOLID_BREP('Body1',#13635);
#1137=MANIFOLD_SOLID_BREP('Body1',#13636);
#1138=MANIFOLD_SOLID_BREP('Body1',#13637);
#1139=MANIFOLD_SOLID_BREP('Body1',#13638);
#1140=MANIFOLD_SOLID_BREP('Body1',#13639);
#1141=MANIFOLD_SOLID_BREP('Body1',#13640);
#1142=MANIFOLD_SOLID_BREP('Body1',#13641);
#1143=FACE_BOUND('',#2476,.T.);
#1144=FACE_BOUND('',#2477,.T.);
#1145=FACE_BOUND('',#2478,.T.);
#1146=FACE_BOUND('',#2479,.T.);
#1147=FACE_BOUND('',#2480,.T.);
#1148=FACE_BOUND('',#2481,.T.);
#1149=FACE_BOUND('',#2482,.T.);
#1150=FACE_BOUND('',#2483,.T.);
#1151=FACE_BOUND('',#2484,.T.);
#1152=FACE_BOUND('',#2485,.T.);
#1153=FACE_BOUND('',#2486,.T.);
#1154=FACE_BOUND('',#2487,.T.);
#1155=FACE_BOUND('',#2489,.T.);
#1156=FACE_BOUND('',#2490,.T.);
#1157=FACE_BOUND('',#2491,.T.);
#1158=FACE_BOUND('',#2492,.T.);
#1159=FACE_BOUND('',#2493,.T.);
#1160=FACE_BOUND('',#2494,.T.);
#1161=FACE_BOUND('',#2495,.T.);
#1162=FACE_BOUND('',#2496,.T.);
#1163=FACE_BOUND('',#2497,.T.);
#1164=FACE_BOUND('',#2498,.T.);
#1165=FACE_BOUND('',#2499,.T.);
#1166=FACE_BOUND('',#2500,.T.);
#1167=FACE_BOUND('',#2531,.T.);
#1168=FACE_BOUND('',#2533,.T.);
#1169=FACE_BOUND('',#2534,.T.);
#1170=FACE_BOUND('',#2535,.T.);
#1171=FACE_BOUND('',#2536,.T.);
#1172=FACE_BOUND('',#2537,.T.);
#1173=FACE_BOUND('',#2544,.T.);
#1174=FACE_BOUND('',#2547,.T.);
#1175=FACE_BOUND('',#2549,.T.);
#1176=FACE_BOUND('',#2550,.T.);
#1177=FACE_BOUND('',#2551,.T.);
#1178=FACE_BOUND('',#2552,.T.);
#1179=FACE_BOUND('',#2553,.T.);
#1180=FACE_BOUND('',#2555,.T.);
#1181=FACE_BOUND('',#2556,.T.);
#1182=FACE_BOUND('',#2557,.T.);
#1183=FACE_BOUND('',#2558,.T.);
#1184=FACE_BOUND('',#2559,.T.);
#1185=FACE_BOUND('',#2563,.T.);
#1186=FACE_BOUND('',#2565,.T.);
#1187=FACE_BOUND('',#2571,.T.);
#1188=FACE_BOUND('',#2578,.T.);
#1189=FACE_BOUND('',#2581,.T.);
#1190=FACE_BOUND('',#2590,.T.);
#1191=FACE_BOUND('',#2591,.T.);
#1192=FACE_BOUND('',#2592,.T.);
#1193=FACE_BOUND('',#2593,.T.);
#1194=FACE_BOUND('',#2594,.T.);
#1195=FACE_BOUND('',#2596,.T.);
#1196=FACE_BOUND('',#2597,.T.);
#1197=FACE_BOUND('',#2598,.T.);
#1198=FACE_BOUND('',#2599,.T.);
#1199=FACE_BOUND('',#2617,.T.);
#1200=FACE_BOUND('',#2619,.T.);
#1201=FACE_BOUND('',#2625,.T.);
#1202=FACE_BOUND('',#2628,.T.);
#1203=FACE_BOUND('',#2632,.T.);
#1204=FACE_BOUND('',#2634,.T.);
#1205=FACE_BOUND('',#2643,.T.);
#1206=FACE_BOUND('',#2646,.T.);
#1207=FACE_BOUND('',#2649,.T.);
#1208=FACE_BOUND('',#2652,.T.);
#1209=FACE_BOUND('',#2662,.T.);
#1210=FACE_BOUND('',#2663,.T.);
#1211=FACE_BOUND('',#2664,.T.);
#1212=FACE_BOUND('',#2665,.T.);
#1213=FACE_BOUND('',#2672,.T.);
#1214=FACE_BOUND('',#2673,.T.);
#1215=FACE_BOUND('',#2674,.T.);
#1216=FACE_BOUND('',#2675,.T.);
#1217=FACE_BOUND('',#2684,.T.);
#1218=FACE_BOUND('',#2687,.T.);
#1219=FACE_BOUND('',#2692,.T.);
#1220=FACE_BOUND('',#2697,.T.);
#1221=FACE_BOUND('',#2722,.T.);
#1222=FACE_BOUND('',#2725,.T.);
#1223=FACE_BOUND('',#2728,.T.);
#1224=FACE_BOUND('',#2731,.T.);
#1225=FACE_BOUND('',#2734,.T.);
#1226=FACE_BOUND('',#2741,.T.);
#1227=FACE_BOUND('',#2760,.T.);
#1228=FACE_BOUND('',#2763,.T.);
#1229=FACE_BOUND('',#2772,.T.);
#1230=FACE_BOUND('',#2773,.T.);
#1231=FACE_BOUND('',#2774,.T.);
#1232=FACE_BOUND('',#2775,.T.);
#1233=FACE_BOUND('',#2776,.T.);
#1234=FACE_BOUND('',#2777,.T.);
#1235=FACE_BOUND('',#2778,.T.);
#1236=FACE_BOUND('',#2779,.T.);
#1237=FACE_BOUND('',#2786,.T.);
#1238=FACE_BOUND('',#2787,.T.);
#1239=FACE_BOUND('',#2788,.T.);
#1240=FACE_BOUND('',#2789,.T.);
#1241=FACE_BOUND('',#2790,.T.);
#1242=FACE_BOUND('',#2791,.T.);
#1243=FACE_BOUND('',#2792,.T.);
#1244=FACE_BOUND('',#2793,.T.);
#1245=FACE_BOUND('',#2794,.T.);
#1246=FACE_BOUND('',#2820,.T.);
#1247=FACE_BOUND('',#2821,.T.);
#1248=FACE_BOUND('',#2822,.T.);
#1249=FACE_BOUND('',#2823,.T.);
#1250=FACE_BOUND('',#2824,.T.);
#1251=FACE_BOUND('',#2829,.T.);
#1252=FACE_BOUND('',#2832,.T.);
#1253=FACE_BOUND('',#2835,.T.);
#1254=FACE_BOUND('',#2837,.T.);
#1255=FACE_BOUND('',#2838,.T.);
#1256=FACE_BOUND('',#2839,.T.);
#1257=FACE_BOUND('',#2840,.T.);
#1258=FACE_BOUND('',#2841,.T.);
#1259=FACE_BOUND('',#2843,.T.);
#1260=FACE_BOUND('',#2844,.T.);
#1261=FACE_BOUND('',#2845,.T.);
#1262=FACE_BOUND('',#2846,.T.);
#1263=FACE_BOUND('',#2847,.T.);
#1264=FACE_BOUND('',#2851,.T.);
#1265=FACE_BOUND('',#2853,.T.);
#1266=FACE_BOUND('',#2861,.T.);
#1267=FACE_BOUND('',#2862,.T.);
#1268=FACE_BOUND('',#2863,.T.);
#1269=FACE_BOUND('',#2864,.T.);
#1270=FACE_BOUND('',#2865,.T.);
#1271=FACE_BOUND('',#2867,.T.);
#1272=FACE_BOUND('',#2868,.T.);
#1273=FACE_BOUND('',#2869,.T.);
#1274=FACE_BOUND('',#2870,.T.);
#1275=FACE_BOUND('',#2871,.T.);
#1276=FACE_BOUND('',#2886,.T.);
#1277=FACE_BOUND('',#2887,.T.);
#1278=FACE_BOUND('',#2888,.T.);
#1279=FACE_BOUND('',#2889,.T.);
#1280=FACE_BOUND('',#2926,.T.);
#1281=FACE_BOUND('',#2945,.T.);
#1282=FACE_BOUND('',#2953,.T.);
#1283=FACE_BOUND('',#2956,.T.);
#1284=FACE_BOUND('',#2961,.T.);
#1285=FACE_BOUND('',#2966,.T.);
#1286=FACE_BOUND('',#2994,.T.);
#1287=FACE_BOUND('',#2997,.T.);
#1288=FACE_BOUND('',#3000,.T.);
#1289=FACE_BOUND('',#3003,.T.);
#1290=FACE_BOUND('',#3006,.T.);
#1291=FACE_BOUND('',#3016,.T.);
#1292=FACE_BOUND('',#3018,.T.);
#1293=FACE_BOUND('',#3022,.T.);
#1294=FACE_BOUND('',#3024,.T.);
#1295=FACE_BOUND('',#3029,.T.);
#1296=FACE_BOUND('',#3031,.T.);
#1297=FACE_BOUND('',#3035,.T.);
#1298=FACE_BOUND('',#3037,.T.);
#1299=FACE_BOUND('',#3041,.T.);
#1300=FACE_BOUND('',#3043,.T.);
#1301=FACE_BOUND('',#3049,.T.);
#1302=FACE_BOUND('',#3051,.T.);
#1303=FACE_BOUND('',#3052,.T.);
#1304=FACE_BOUND('',#3054,.T.);
#1305=FACE_BOUND('',#3056,.T.);
#1306=FACE_BOUND('',#3066,.T.);
#1307=FACE_BOUND('',#3068,.T.);
#1308=FACE_BOUND('',#3073,.T.);
#1309=FACE_BOUND('',#3077,.T.);
#1310=FACE_BOUND('',#3158,.T.);
#1311=FACE_BOUND('',#3168,.T.);
#1312=FACE_BOUND('',#3170,.T.);
#1313=FACE_BOUND('',#3174,.T.);
#1314=FACE_BOUND('',#3176,.T.);
#1315=FACE_BOUND('',#3181,.T.);
#1316=FACE_BOUND('',#3183,.T.);
#1317=FACE_BOUND('',#3187,.T.);
#1318=FACE_BOUND('',#3189,.T.);
#1319=FACE_BOUND('',#3192,.T.);
#1320=FACE_BOUND('',#3194,.T.);
#1321=FACE_BOUND('',#3196,.T.);
#1322=FACE_BOUND('',#3198,.T.);
#1323=FACE_BOUND('',#3208,.T.);
#1324=FACE_BOUND('',#3210,.T.);
#1325=FACE_BOUND('',#3220,.T.);
#1326=FACE_BOUND('',#3227,.T.);
#1327=FACE_BOUND('',#3231,.T.);
#1328=FACE_BOUND('',#3392,.T.);
#1329=FACE_BOUND('',#3408,.T.);
#1330=PLANE('',#14234);
#1331=PLANE('',#14235);
#1332=PLANE('',#14236);
#1333=PLANE('',#14237);
#1334=PLANE('',#14238);
#1335=PLANE('',#14239);
#1336=PLANE('',#14241);
#1337=PLANE('',#14242);
#1338=PLANE('',#14243);
#1339=PLANE('',#14244);
#1340=PLANE('',#14245);
#1341=PLANE('',#14246);
#1342=PLANE('',#14248);
#1343=PLANE('',#14249);
#1344=PLANE('',#14250);
#1345=PLANE('',#14251);
#1346=PLANE('',#14252);
#1347=PLANE('',#14253);
#1348=PLANE('',#14259);
#1349=PLANE('',#14263);
#1350=PLANE('',#14267);
#1351=PLANE('',#14271);
#1352=PLANE('',#14272);
#1353=PLANE('',#14280);
#1354=PLANE('',#14285);
#1355=PLANE('',#14290);
#1356=PLANE('',#14299);
#1357=PLANE('',#14316);
#1358=PLANE('',#14322);
#1359=PLANE('',#14323);
#1360=PLANE('',#14331);
#1361=PLANE('',#14332);
#1362=PLANE('',#14346);
#1363=PLANE('',#14362);
#1364=PLANE('',#14366);
#1365=PLANE('',#14383);
#1366=PLANE('',#14387);
#1367=PLANE('',#14388);
#1368=PLANE('',#14390);
#1369=PLANE('',#14395);
#1370=PLANE('',#14407);
#1371=PLANE('',#14409);
#1372=PLANE('',#14410);
#1373=PLANE('',#14411);
#1374=PLANE('',#14412);
#1375=PLANE('',#14413);
#1376=PLANE('',#14414);
#1377=PLANE('',#14415);
#1378=PLANE('',#14416);
#1379=PLANE('',#14417);
#1380=PLANE('',#14418);
#1381=PLANE('',#14419);
#1382=PLANE('',#14420);
#1383=PLANE('',#14426);
#1384=PLANE('',#14427);
#1385=PLANE('',#14428);
#1386=PLANE('',#14429);
#1387=PLANE('',#14430);
#1388=PLANE('',#14431);
#1389=PLANE('',#14439);
#1390=PLANE('',#14440);
#1391=PLANE('',#14445);
#1392=PLANE('',#14446);
#1393=PLANE('',#14451);
#1394=PLANE('',#14452);
#1395=PLANE('',#14457);
#1396=PLANE('',#14462);
#1397=PLANE('',#14467);
#1398=PLANE('',#14472);
#1399=PLANE('',#14482);
#1400=PLANE('',#14483);
#1401=PLANE('',#14484);
#1402=PLANE('',#14485);
#1403=PLANE('',#14486);
#1404=PLANE('',#14487);
#1405=PLANE('',#14488);
#1406=PLANE('',#14489);
#1407=PLANE('',#14490);
#1408=PLANE('',#14491);
#1409=PLANE('',#14492);
#1410=PLANE('',#14493);
#1411=PLANE('',#14494);
#1412=PLANE('',#14495);
#1413=PLANE('',#14511);
#1414=PLANE('',#14514);
#1415=PLANE('',#14526);
#1416=PLANE('',#14535);
#1417=PLANE('',#14566);
#1418=PLANE('',#14571);
#1419=PLANE('',#14576);
#1420=PLANE('',#14582);
#1421=PLANE('',#14587);
#1422=PLANE('',#14596);
#1423=PLANE('',#14600);
#1424=PLANE('',#14601);
#1425=PLANE('',#14603);
#1426=PLANE('',#14608);
#1427=PLANE('',#14611);
#1428=PLANE('',#14616);
#1429=PLANE('',#14625);
#1430=PLANE('',#14633);
#1431=PLANE('',#14641);
#1432=PLANE('',#14642);
#1433=PLANE('',#14643);
#1434=PLANE('',#14644);
#1435=PLANE('',#14645);
#1436=PLANE('',#14646);
#1437=PLANE('',#14647);
#1438=PLANE('',#14648);
#1439=PLANE('',#14649);
#1440=PLANE('',#14667);
#1441=PLANE('',#14668);
#1442=PLANE('',#14669);
#1443=PLANE('',#14670);
#1444=PLANE('',#14671);
#1445=PLANE('',#14687);
#1446=PLANE('',#14688);
#1447=PLANE('',#14689);
#1448=PLANE('',#14690);
#1449=PLANE('',#14691);
#1450=PLANE('',#14692);
#1451=PLANE('',#14693);
#1452=PLANE('',#14695);
#1453=PLANE('',#14696);
#1454=PLANE('',#14697);
#1455=PLANE('',#14698);
#1456=PLANE('',#14699);
#1457=PLANE('',#14700);
#1458=PLANE('',#14706);
#1459=PLANE('',#14710);
#1460=PLANE('',#14714);
#1461=PLANE('',#14718);
#1462=PLANE('',#14722);
#1463=PLANE('',#14727);
#1464=PLANE('',#14732);
#1465=PLANE('',#14737);
#1466=PLANE('',#14742);
#1467=PLANE('',#14763);
#1468=PLANE('',#14769);
#1469=PLANE('',#14770);
#1470=PLANE('',#14778);
#1471=PLANE('',#14779);
#1472=PLANE('',#14799);
#1473=PLANE('',#14800);
#1474=PLANE('',#14803);
#1475=PLANE('',#14809);
#1476=PLANE('',#14815);
#1477=PLANE('',#14821);
#1478=PLANE('',#14827);
#1479=PLANE('',#14828);
#1480=PLANE('',#14829);
#1481=PLANE('',#14830);
#1482=PLANE('',#14831);
#1483=PLANE('',#14832);
#1484=PLANE('',#14833);
#1485=PLANE('',#14834);
#1486=PLANE('',#14835);
#1487=PLANE('',#14836);
#1488=PLANE('',#14837);
#1489=PLANE('',#14838);
#1490=PLANE('',#14839);
#1491=PLANE('',#14840);
#1492=PLANE('',#14842);
#1493=PLANE('',#14843);
#1494=PLANE('',#14844);
#1495=PLANE('',#14845);
#1496=PLANE('',#14846);
#1497=PLANE('',#14847);
#1498=PLANE('',#14848);
#1499=PLANE('',#14849);
#1500=PLANE('',#14850);
#1501=PLANE('',#14851);
#1502=PLANE('',#14853);
#1503=PLANE('',#14854);
#1504=PLANE('',#14855);
#1505=PLANE('',#14856);
#1506=PLANE('',#14857);
#1507=PLANE('',#14858);
#1508=PLANE('',#14859);
#1509=PLANE('',#14860);
#1510=PLANE('',#14861);
#1511=PLANE('',#14862);
#1512=PLANE('',#14867);
#1513=PLANE('',#14868);
#1514=PLANE('',#14869);
#1515=PLANE('',#14870);
#1516=PLANE('',#14871);
#1517=PLANE('',#14872);
#1518=PLANE('',#14873);
#1519=PLANE('',#14874);
#1520=PLANE('',#14882);
#1521=PLANE('',#14884);
#1522=PLANE('',#14885);
#1523=PLANE('',#14886);
#1524=PLANE('',#14887);
#1525=PLANE('',#14888);
#1526=PLANE('',#14889);
#1527=PLANE('',#14890);
#1528=PLANE('',#14891);
#1529=PLANE('',#14892);
#1530=PLANE('',#14894);
#1531=PLANE('',#14902);
#1532=PLANE('',#14922);
#1533=PLANE('',#14925);
#1534=PLANE('',#14937);
#1535=PLANE('',#14946);
#1536=PLANE('',#14979);
#1537=PLANE('',#14984);
#1538=PLANE('',#14989);
#1539=PLANE('',#14994);
#1540=PLANE('',#14999);
#1541=PLANE('',#15004);
#1542=PLANE('',#15013);
#1543=PLANE('',#15017);
#1544=PLANE('',#15018);
#1545=PLANE('',#15020);
#1546=PLANE('',#15025);
#1547=PLANE('',#15028);
#1548=PLANE('',#15033);
#1549=PLANE('',#15046);
#1550=PLANE('',#15047);
#1551=PLANE('',#15048);
#1552=PLANE('',#15050);
#1553=PLANE('',#15051);
#1554=PLANE('',#15052);
#1555=PLANE('',#15054);
#1556=PLANE('',#15057);
#1557=PLANE('',#15065);
#1558=PLANE('',#15066);
#1559=PLANE('',#15074);
#1560=PLANE('',#15075);
#1561=PLANE('',#15083);
#1562=PLANE('',#15084);
#1563=PLANE('',#15092);
#1564=PLANE('',#15093);
#1565=PLANE('',#15095);
#1566=PLANE('',#15097);
#1567=PLANE('',#15103);
#1568=PLANE('',#15110);
#1569=PLANE('',#15111);
#1570=PLANE('',#15113);
#1571=PLANE('',#15114);
#1572=PLANE('',#15115);
#1573=PLANE('',#15116);
#1574=PLANE('',#15117);
#1575=PLANE('',#15118);
#1576=PLANE('',#15126);
#1577=PLANE('',#15127);
#1578=PLANE('',#15129);
#1579=PLANE('',#15130);
#1580=PLANE('',#15131);
#1581=PLANE('',#15132);
#1582=PLANE('',#15159);
#1583=PLANE('',#15160);
#1584=PLANE('',#15163);
#1585=PLANE('',#15166);
#1586=PLANE('',#15169);
#1587=PLANE('',#15172);
#1588=PLANE('',#15175);
#1589=PLANE('',#15178);
#1590=PLANE('',#15181);
#1591=PLANE('',#15184);
#1592=PLANE('',#15187);
#1593=PLANE('',#15190);
#1594=PLANE('',#15193);
#1595=PLANE('',#15196);
#1596=PLANE('',#15199);
#1597=PLANE('',#15202);
#1598=PLANE('',#15205);
#1599=PLANE('',#15208);
#1600=PLANE('',#15211);
#1601=PLANE('',#15214);
#1602=PLANE('',#15217);
#1603=PLANE('',#15218);
#1604=PLANE('',#15226);
#1605=PLANE('',#15227);
#1606=PLANE('',#15228);
#1607=PLANE('',#15230);
#1608=PLANE('',#15231);
#1609=PLANE('',#15232);
#1610=PLANE('',#15234);
#1611=PLANE('',#15237);
#1612=PLANE('',#15245);
#1613=PLANE('',#15246);
#1614=PLANE('',#15254);
#1615=PLANE('',#15255);
#1616=PLANE('',#15263);
#1617=PLANE('',#15264);
#1618=PLANE('',#15273);
#1619=PLANE('',#15274);
#1620=PLANE('',#15276);
#1621=PLANE('',#15277);
#1622=PLANE('',#15278);
#1623=PLANE('',#15279);
#1624=PLANE('',#15280);
#1625=PLANE('',#15281);
#1626=PLANE('',#15289);
#1627=PLANE('',#15290);
#1628=PLANE('',#15292);
#1629=PLANE('',#15294);
#1630=PLANE('',#15295);
#1631=PLANE('',#15296);
#1632=PLANE('',#15297);
#1633=PLANE('',#15298);
#1634=PLANE('',#15299);
#1635=PLANE('',#15300);
#1636=PLANE('',#15301);
#1637=PLANE('',#15307);
#1638=PLANE('',#15308);
#1639=PLANE('',#15309);
#1640=PLANE('',#15310);
#1641=PLANE('',#15357);
#1642=PLANE('',#15358);
#1643=PLANE('',#15361);
#1644=PLANE('',#15364);
#1645=PLANE('',#15367);
#1646=PLANE('',#15370);
#1647=PLANE('',#15373);
#1648=PLANE('',#15376);
#1649=PLANE('',#15379);
#1650=PLANE('',#15382);
#1651=PLANE('',#15385);
#1652=PLANE('',#15388);
#1653=PLANE('',#15391);
#1654=PLANE('',#15394);
#1655=PLANE('',#15397);
#1656=PLANE('',#15400);
#1657=PLANE('',#15403);
#1658=PLANE('',#15406);
#1659=PLANE('',#15409);
#1660=PLANE('',#15412);
#1661=PLANE('',#15415);
#1662=PLANE('',#15418);
#1663=PLANE('',#15421);
#1664=PLANE('',#15424);
#1665=PLANE('',#15427);
#1666=PLANE('',#15430);
#1667=PLANE('',#15433);
#1668=PLANE('',#15436);
#1669=PLANE('',#15439);
#1670=PLANE('',#15442);
#1671=PLANE('',#15445);
#1672=PLANE('',#15448);
#1673=PLANE('',#15451);
#1674=PLANE('',#15454);
#1675=PLANE('',#15457);
#1676=PLANE('',#15460);
#1677=PLANE('',#15463);
#1678=PLANE('',#15466);
#1679=PLANE('',#15469);
#1680=PLANE('',#15472);
#1681=PLANE('',#15475);
#1682=PLANE('',#15476);
#1683=PLANE('',#15480);
#1684=PLANE('',#15481);
#1685=PLANE('',#15482);
#1686=PLANE('',#15483);
#1687=PLANE('',#15484);
#1688=PLANE('',#15485);
#1689=PLANE('',#15486);
#1690=PLANE('',#15487);
#1691=PLANE('',#15488);
#1692=PLANE('',#15490);
#1693=PLANE('',#15498);
#1694=FACE_OUTER_BOUND('',#2459,.T.);
#1695=FACE_OUTER_BOUND('',#2460,.T.);
#1696=FACE_OUTER_BOUND('',#2461,.T.);
#1697=FACE_OUTER_BOUND('',#2462,.T.);
#1698=FACE_OUTER_BOUND('',#2463,.T.);
#1699=FACE_OUTER_BOUND('',#2464,.T.);
#1700=FACE_OUTER_BOUND('',#2465,.T.);
#1701=FACE_OUTER_BOUND('',#2466,.T.);
#1702=FACE_OUTER_BOUND('',#2467,.T.);
#1703=FACE_OUTER_BOUND('',#2468,.T.);
#1704=FACE_OUTER_BOUND('',#2469,.T.);
#1705=FACE_OUTER_BOUND('',#2470,.T.);
#1706=FACE_OUTER_BOUND('',#2471,.T.);
#1707=FACE_OUTER_BOUND('',#2472,.T.);
#1708=FACE_OUTER_BOUND('',#2473,.T.);
#1709=FACE_OUTER_BOUND('',#2474,.T.);
#1710=FACE_OUTER_BOUND('',#2475,.T.);
#1711=FACE_OUTER_BOUND('',#2488,.T.);
#1712=FACE_OUTER_BOUND('',#2501,.T.);
#1713=FACE_OUTER_BOUND('',#2502,.T.);
#1714=FACE_OUTER_BOUND('',#2503,.T.);
#1715=FACE_OUTER_BOUND('',#2504,.T.);
#1716=FACE_OUTER_BOUND('',#2505,.T.);
#1717=FACE_OUTER_BOUND('',#2506,.T.);
#1718=FACE_OUTER_BOUND('',#2507,.T.);
#1719=FACE_OUTER_BOUND('',#2508,.T.);
#1720=FACE_OUTER_BOUND('',#2509,.T.);
#1721=FACE_OUTER_BOUND('',#2510,.T.);
#1722=FACE_OUTER_BOUND('',#2511,.T.);
#1723=FACE_OUTER_BOUND('',#2512,.T.);
#1724=FACE_OUTER_BOUND('',#2513,.T.);
#1725=FACE_OUTER_BOUND('',#2514,.T.);
#1726=FACE_OUTER_BOUND('',#2515,.T.);
#1727=FACE_OUTER_BOUND('',#2516,.T.);
#1728=FACE_OUTER_BOUND('',#2517,.T.);
#1729=FACE_OUTER_BOUND('',#2518,.T.);
#1730=FACE_OUTER_BOUND('',#2519,.T.);
#1731=FACE_OUTER_BOUND('',#2520,.T.);
#1732=FACE_OUTER_BOUND('',#2521,.T.);
#1733=FACE_OUTER_BOUND('',#2522,.T.);
#1734=FACE_OUTER_BOUND('',#2523,.T.);
#1735=FACE_OUTER_BOUND('',#2524,.T.);
#1736=FACE_OUTER_BOUND('',#2525,.T.);
#1737=FACE_OUTER_BOUND('',#2526,.T.);
#1738=FACE_OUTER_BOUND('',#2527,.T.);
#1739=FACE_OUTER_BOUND('',#2528,.T.);
#1740=FACE_OUTER_BOUND('',#2529,.T.);
#1741=FACE_OUTER_BOUND('',#2530,.T.);
#1742=FACE_OUTER_BOUND('',#2532,.T.);
#1743=FACE_OUTER_BOUND('',#2538,.T.);
#1744=FACE_OUTER_BOUND('',#2539,.T.);
#1745=FACE_OUTER_BOUND('',#2540,.T.);
#1746=FACE_OUTER_BOUND('',#2541,.T.);
#1747=FACE_OUTER_BOUND('',#2542,.T.);
#1748=FACE_OUTER_BOUND('',#2543,.T.);
#1749=FACE_OUTER_BOUND('',#2545,.T.);
#1750=FACE_OUTER_BOUND('',#2546,.T.);
#1751=FACE_OUTER_BOUND('',#2548,.T.);
#1752=FACE_OUTER_BOUND('',#2554,.T.);
#1753=FACE_OUTER_BOUND('',#2560,.T.);
#1754=FACE_OUTER_BOUND('',#2561,.T.);
#1755=FACE_OUTER_BOUND('',#2562,.T.);
#1756=FACE_OUTER_BOUND('',#2564,.T.);
#1757=FACE_OUTER_BOUND('',#2566,.T.);
#1758=FACE_OUTER_BOUND('',#2567,.T.);
#1759=FACE_OUTER_BOUND('',#2568,.T.);
#1760=FACE_OUTER_BOUND('',#2569,.T.);
#1761=FACE_OUTER_BOUND('',#2570,.T.);
#1762=FACE_OUTER_BOUND('',#2572,.T.);
#1763=FACE_OUTER_BOUND('',#2573,.T.);
#1764=FACE_OUTER_BOUND('',#2574,.T.);
#1765=FACE_OUTER_BOUND('',#2575,.T.);
#1766=FACE_OUTER_BOUND('',#2576,.T.);
#1767=FACE_OUTER_BOUND('',#2577,.T.);
#1768=FACE_OUTER_BOUND('',#2579,.T.);
#1769=FACE_OUTER_BOUND('',#2580,.T.);
#1770=FACE_OUTER_BOUND('',#2582,.T.);
#1771=FACE_OUTER_BOUND('',#2583,.T.);
#1772=FACE_OUTER_BOUND('',#2584,.T.);
#1773=FACE_OUTER_BOUND('',#2585,.T.);
#1774=FACE_OUTER_BOUND('',#2586,.T.);
#1775=FACE_OUTER_BOUND('',#2587,.T.);
#1776=FACE_OUTER_BOUND('',#2588,.T.);
#1777=FACE_OUTER_BOUND('',#2589,.T.);
#1778=FACE_OUTER_BOUND('',#2595,.T.);
#1779=FACE_OUTER_BOUND('',#2600,.T.);
#1780=FACE_OUTER_BOUND('',#2601,.T.);
#1781=FACE_OUTER_BOUND('',#2602,.T.);
#1782=FACE_OUTER_BOUND('',#2603,.T.);
#1783=FACE_OUTER_BOUND('',#2604,.T.);
#1784=FACE_OUTER_BOUND('',#2605,.T.);
#1785=FACE_OUTER_BOUND('',#2606,.T.);
#1786=FACE_OUTER_BOUND('',#2607,.T.);
#1787=FACE_OUTER_BOUND('',#2608,.T.);
#1788=FACE_OUTER_BOUND('',#2609,.T.);
#1789=FACE_OUTER_BOUND('',#2610,.T.);
#1790=FACE_OUTER_BOUND('',#2611,.T.);
#1791=FACE_OUTER_BOUND('',#2612,.T.);
#1792=FACE_OUTER_BOUND('',#2613,.T.);
#1793=FACE_OUTER_BOUND('',#2614,.T.);
#1794=FACE_OUTER_BOUND('',#2615,.T.);
#1795=FACE_OUTER_BOUND('',#2616,.T.);
#1796=FACE_OUTER_BOUND('',#2618,.T.);
#1797=FACE_OUTER_BOUND('',#2620,.T.);
#1798=FACE_OUTER_BOUND('',#2621,.T.);
#1799=FACE_OUTER_BOUND('',#2622,.T.);
#1800=FACE_OUTER_BOUND('',#2623,.T.);
#1801=FACE_OUTER_BOUND('',#2624,.T.);
#1802=FACE_OUTER_BOUND('',#2626,.T.);
#1803=FACE_OUTER_BOUND('',#2627,.T.);
#1804=FACE_OUTER_BOUND('',#2629,.T.);
#1805=FACE_OUTER_BOUND('',#2630,.T.);
#1806=FACE_OUTER_BOUND('',#2631,.T.);
#1807=FACE_OUTER_BOUND('',#2633,.T.);
#1808=FACE_OUTER_BOUND('',#2635,.T.);
#1809=FACE_OUTER_BOUND('',#2636,.T.);
#1810=FACE_OUTER_BOUND('',#2637,.T.);
#1811=FACE_OUTER_BOUND('',#2638,.T.);
#1812=FACE_OUTER_BOUND('',#2639,.T.);
#1813=FACE_OUTER_BOUND('',#2640,.T.);
#1814=FACE_OUTER_BOUND('',#2641,.T.);
#1815=FACE_OUTER_BOUND('',#2642,.T.);
#1816=FACE_OUTER_BOUND('',#2644,.T.);
#1817=FACE_OUTER_BOUND('',#2645,.T.);
#1818=FACE_OUTER_BOUND('',#2647,.T.);
#1819=FACE_OUTER_BOUND('',#2648,.T.);
#1820=FACE_OUTER_BOUND('',#2650,.T.);
#1821=FACE_OUTER_BOUND('',#2651,.T.);
#1822=FACE_OUTER_BOUND('',#2653,.T.);
#1823=FACE_OUTER_BOUND('',#2654,.T.);
#1824=FACE_OUTER_BOUND('',#2655,.T.);
#1825=FACE_OUTER_BOUND('',#2656,.T.);
#1826=FACE_OUTER_BOUND('',#2657,.T.);
#1827=FACE_OUTER_BOUND('',#2658,.T.);
#1828=FACE_OUTER_BOUND('',#2659,.T.);
#1829=FACE_OUTER_BOUND('',#2660,.T.);
#1830=FACE_OUTER_BOUND('',#2661,.T.);
#1831=FACE_OUTER_BOUND('',#2666,.T.);
#1832=FACE_OUTER_BOUND('',#2667,.T.);
#1833=FACE_OUTER_BOUND('',#2668,.T.);
#1834=FACE_OUTER_BOUND('',#2669,.T.);
#1835=FACE_OUTER_BOUND('',#2670,.T.);
#1836=FACE_OUTER_BOUND('',#2671,.T.);
#1837=FACE_OUTER_BOUND('',#2676,.T.);
#1838=FACE_OUTER_BOUND('',#2677,.T.);
#1839=FACE_OUTER_BOUND('',#2678,.T.);
#1840=FACE_OUTER_BOUND('',#2679,.T.);
#1841=FACE_OUTER_BOUND('',#2680,.T.);
#1842=FACE_OUTER_BOUND('',#2681,.T.);
#1843=FACE_OUTER_BOUND('',#2682,.T.);
#1844=FACE_OUTER_BOUND('',#2683,.T.);
#1845=FACE_OUTER_BOUND('',#2685,.T.);
#1846=FACE_OUTER_BOUND('',#2686,.T.);
#1847=FACE_OUTER_BOUND('',#2688,.T.);
#1848=FACE_OUTER_BOUND('',#2689,.T.);
#1849=FACE_OUTER_BOUND('',#2690,.T.);
#1850=FACE_OUTER_BOUND('',#2691,.T.);
#1851=FACE_OUTER_BOUND('',#2693,.T.);
#1852=FACE_OUTER_BOUND('',#2694,.T.);
#1853=FACE_OUTER_BOUND('',#2695,.T.);
#1854=FACE_OUTER_BOUND('',#2696,.T.);
#1855=FACE_OUTER_BOUND('',#2698,.T.);
#1856=FACE_OUTER_BOUND('',#2699,.T.);
#1857=FACE_OUTER_BOUND('',#2700,.T.);
#1858=FACE_OUTER_BOUND('',#2701,.T.);
#1859=FACE_OUTER_BOUND('',#2702,.T.);
#1860=FACE_OUTER_BOUND('',#2703,.T.);
#1861=FACE_OUTER_BOUND('',#2704,.T.);
#1862=FACE_OUTER_BOUND('',#2705,.T.);
#1863=FACE_OUTER_BOUND('',#2706,.T.);
#1864=FACE_OUTER_BOUND('',#2707,.T.);
#1865=FACE_OUTER_BOUND('',#2708,.T.);
#1866=FACE_OUTER_BOUND('',#2709,.T.);
#1867=FACE_OUTER_BOUND('',#2710,.T.);
#1868=FACE_OUTER_BOUND('',#2711,.T.);
#1869=FACE_OUTER_BOUND('',#2712,.T.);
#1870=FACE_OUTER_BOUND('',#2713,.T.);
#1871=FACE_OUTER_BOUND('',#2714,.T.);
#1872=FACE_OUTER_BOUND('',#2715,.T.);
#1873=FACE_OUTER_BOUND('',#2716,.T.);
#1874=FACE_OUTER_BOUND('',#2717,.T.);
#1875=FACE_OUTER_BOUND('',#2718,.T.);
#1876=FACE_OUTER_BOUND('',#2719,.T.);
#1877=FACE_OUTER_BOUND('',#2720,.T.);
#1878=FACE_OUTER_BOUND('',#2721,.T.);
#1879=FACE_OUTER_BOUND('',#2723,.T.);
#1880=FACE_OUTER_BOUND('',#2724,.T.);
#1881=FACE_OUTER_BOUND('',#2726,.T.);
#1882=FACE_OUTER_BOUND('',#2727,.T.);
#1883=FACE_OUTER_BOUND('',#2729,.T.);
#1884=FACE_OUTER_BOUND('',#2730,.T.);
#1885=FACE_OUTER_BOUND('',#2732,.T.);
#1886=FACE_OUTER_BOUND('',#2733,.T.);
#1887=FACE_OUTER_BOUND('',#2735,.T.);
#1888=FACE_OUTER_BOUND('',#2736,.T.);
#1889=FACE_OUTER_BOUND('',#2737,.T.);
#1890=FACE_OUTER_BOUND('',#2738,.T.);
#1891=FACE_OUTER_BOUND('',#2739,.T.);
#1892=FACE_OUTER_BOUND('',#2740,.T.);
#1893=FACE_OUTER_BOUND('',#2742,.T.);
#1894=FACE_OUTER_BOUND('',#2743,.T.);
#1895=FACE_OUTER_BOUND('',#2744,.T.);
#1896=FACE_OUTER_BOUND('',#2745,.T.);
#1897=FACE_OUTER_BOUND('',#2746,.T.);
#1898=FACE_OUTER_BOUND('',#2747,.T.);
#1899=FACE_OUTER_BOUND('',#2748,.T.);
#1900=FACE_OUTER_BOUND('',#2749,.T.);
#1901=FACE_OUTER_BOUND('',#2750,.T.);
#1902=FACE_OUTER_BOUND('',#2751,.T.);
#1903=FACE_OUTER_BOUND('',#2752,.T.);
#1904=FACE_OUTER_BOUND('',#2753,.T.);
#1905=FACE_OUTER_BOUND('',#2754,.T.);
#1906=FACE_OUTER_BOUND('',#2755,.T.);
#1907=FACE_OUTER_BOUND('',#2756,.T.);
#1908=FACE_OUTER_BOUND('',#2757,.T.);
#1909=FACE_OUTER_BOUND('',#2758,.T.);
#1910=FACE_OUTER_BOUND('',#2759,.T.);
#1911=FACE_OUTER_BOUND('',#2761,.T.);
#1912=FACE_OUTER_BOUND('',#2762,.T.);
#1913=FACE_OUTER_BOUND('',#2764,.T.);
#1914=FACE_OUTER_BOUND('',#2765,.T.);
#1915=FACE_OUTER_BOUND('',#2766,.T.);
#1916=FACE_OUTER_BOUND('',#2767,.T.);
#1917=FACE_OUTER_BOUND('',#2768,.T.);
#1918=FACE_OUTER_BOUND('',#2769,.T.);
#1919=FACE_OUTER_BOUND('',#2770,.T.);
#1920=FACE_OUTER_BOUND('',#2771,.T.);
#1921=FACE_OUTER_BOUND('',#2780,.T.);
#1922=FACE_OUTER_BOUND('',#2781,.T.);
#1923=FACE_OUTER_BOUND('',#2782,.T.);
#1924=FACE_OUTER_BOUND('',#2783,.T.);
#1925=FACE_OUTER_BOUND('',#2784,.T.);
#1926=FACE_OUTER_BOUND('',#2785,.T.);
#1927=FACE_OUTER_BOUND('',#2795,.T.);
#1928=FACE_OUTER_BOUND('',#2796,.T.);
#1929=FACE_OUTER_BOUND('',#2797,.T.);
#1930=FACE_OUTER_BOUND('',#2798,.T.);
#1931=FACE_OUTER_BOUND('',#2799,.T.);
#1932=FACE_OUTER_BOUND('',#2800,.T.);
#1933=FACE_OUTER_BOUND('',#2801,.T.);
#1934=FACE_OUTER_BOUND('',#2802,.T.);
#1935=FACE_OUTER_BOUND('',#2803,.T.);
#1936=FACE_OUTER_BOUND('',#2804,.T.);
#1937=FACE_OUTER_BOUND('',#2805,.T.);
#1938=FACE_OUTER_BOUND('',#2806,.T.);
#1939=FACE_OUTER_BOUND('',#2807,.T.);
#1940=FACE_OUTER_BOUND('',#2808,.T.);
#1941=FACE_OUTER_BOUND('',#2809,.T.);
#1942=FACE_OUTER_BOUND('',#2810,.T.);
#1943=FACE_OUTER_BOUND('',#2811,.T.);
#1944=FACE_OUTER_BOUND('',#2812,.T.);
#1945=FACE_OUTER_BOUND('',#2813,.T.);
#1946=FACE_OUTER_BOUND('',#2814,.T.);
#1947=FACE_OUTER_BOUND('',#2815,.T.);
#1948=FACE_OUTER_BOUND('',#2816,.T.);
#1949=FACE_OUTER_BOUND('',#2817,.T.);
#1950=FACE_OUTER_BOUND('',#2818,.T.);
#1951=FACE_OUTER_BOUND('',#2819,.T.);
#1952=FACE_OUTER_BOUND('',#2825,.T.);
#1953=FACE_OUTER_BOUND('',#2826,.T.);
#1954=FACE_OUTER_BOUND('',#2827,.T.);
#1955=FACE_OUTER_BOUND('',#2828,.T.);
#1956=FACE_OUTER_BOUND('',#2830,.T.);
#1957=FACE_OUTER_BOUND('',#2831,.T.);
#1958=FACE_OUTER_BOUND('',#2833,.T.);
#1959=FACE_OUTER_BOUND('',#2834,.T.);
#1960=FACE_OUTER_BOUND('',#2836,.T.);
#1961=FACE_OUTER_BOUND('',#2842,.T.);
#1962=FACE_OUTER_BOUND('',#2848,.T.);
#1963=FACE_OUTER_BOUND('',#2849,.T.);
#1964=FACE_OUTER_BOUND('',#2850,.T.);
#1965=FACE_OUTER_BOUND('',#2852,.T.);
#1966=FACE_OUTER_BOUND('',#2854,.T.);
#1967=FACE_OUTER_BOUND('',#2855,.T.);
#1968=FACE_OUTER_BOUND('',#2856,.T.);
#1969=FACE_OUTER_BOUND('',#2857,.T.);
#1970=FACE_OUTER_BOUND('',#2858,.T.);
#1971=FACE_OUTER_BOUND('',#2859,.T.);
#1972=FACE_OUTER_BOUND('',#2860,.T.);
#1973=FACE_OUTER_BOUND('',#2866,.T.);
#1974=FACE_OUTER_BOUND('',#2872,.T.);
#1975=FACE_OUTER_BOUND('',#2873,.T.);
#1976=FACE_OUTER_BOUND('',#2874,.T.);
#1977=FACE_OUTER_BOUND('',#2875,.T.);
#1978=FACE_OUTER_BOUND('',#2876,.T.);
#1979=FACE_OUTER_BOUND('',#2877,.T.);
#1980=FACE_OUTER_BOUND('',#2878,.T.);
#1981=FACE_OUTER_BOUND('',#2879,.T.);
#1982=FACE_OUTER_BOUND('',#2880,.T.);
#1983=FACE_OUTER_BOUND('',#2881,.T.);
#1984=FACE_OUTER_BOUND('',#2882,.T.);
#1985=FACE_OUTER_BOUND('',#2883,.T.);
#1986=FACE_OUTER_BOUND('',#2884,.T.);
#1987=FACE_OUTER_BOUND('',#2885,.T.);
#1988=FACE_OUTER_BOUND('',#2890,.T.);
#1989=FACE_OUTER_BOUND('',#2891,.T.);
#1990=FACE_OUTER_BOUND('',#2892,.T.);
#1991=FACE_OUTER_BOUND('',#2893,.T.);
#1992=FACE_OUTER_BOUND('',#2894,.T.);
#1993=FACE_OUTER_BOUND('',#2895,.T.);
#1994=FACE_OUTER_BOUND('',#2896,.T.);
#1995=FACE_OUTER_BOUND('',#2897,.T.);
#1996=FACE_OUTER_BOUND('',#2898,.T.);
#1997=FACE_OUTER_BOUND('',#2899,.T.);
#1998=FACE_OUTER_BOUND('',#2900,.T.);
#1999=FACE_OUTER_BOUND('',#2901,.T.);
#2000=FACE_OUTER_BOUND('',#2902,.T.);
#2001=FACE_OUTER_BOUND('',#2903,.T.);
#2002=FACE_OUTER_BOUND('',#2904,.T.);
#2003=FACE_OUTER_BOUND('',#2905,.T.);
#2004=FACE_OUTER_BOUND('',#2906,.T.);
#2005=FACE_OUTER_BOUND('',#2907,.T.);
#2006=FACE_OUTER_BOUND('',#2908,.T.);
#2007=FACE_OUTER_BOUND('',#2909,.T.);
#2008=FACE_OUTER_BOUND('',#2910,.T.);
#2009=FACE_OUTER_BOUND('',#2911,.T.);
#2010=FACE_OUTER_BOUND('',#2912,.T.);
#2011=FACE_OUTER_BOUND('',#2913,.T.);
#2012=FACE_OUTER_BOUND('',#2914,.T.);
#2013=FACE_OUTER_BOUND('',#2915,.T.);
#2014=FACE_OUTER_BOUND('',#2916,.T.);
#2015=FACE_OUTER_BOUND('',#2917,.T.);
#2016=FACE_OUTER_BOUND('',#2918,.T.);
#2017=FACE_OUTER_BOUND('',#2919,.T.);
#2018=FACE_OUTER_BOUND('',#2920,.T.);
#2019=FACE_OUTER_BOUND('',#2921,.T.);
#2020=FACE_OUTER_BOUND('',#2922,.T.);
#2021=FACE_OUTER_BOUND('',#2923,.T.);
#2022=FACE_OUTER_BOUND('',#2924,.T.);
#2023=FACE_OUTER_BOUND('',#2925,.T.);
#2024=FACE_OUTER_BOUND('',#2927,.T.);
#2025=FACE_OUTER_BOUND('',#2928,.T.);
#2026=FACE_OUTER_BOUND('',#2929,.T.);
#2027=FACE_OUTER_BOUND('',#2930,.T.);
#2028=FACE_OUTER_BOUND('',#2931,.T.);
#2029=FACE_OUTER_BOUND('',#2932,.T.);
#2030=FACE_OUTER_BOUND('',#2933,.T.);
#2031=FACE_OUTER_BOUND('',#2934,.T.);
#2032=FACE_OUTER_BOUND('',#2935,.T.);
#2033=FACE_OUTER_BOUND('',#2936,.T.);
#2034=FACE_OUTER_BOUND('',#2937,.T.);
#2035=FACE_OUTER_BOUND('',#2938,.T.);
#2036=FACE_OUTER_BOUND('',#2939,.T.);
#2037=FACE_OUTER_BOUND('',#2940,.T.);
#2038=FACE_OUTER_BOUND('',#2941,.T.);
#2039=FACE_OUTER_BOUND('',#2942,.T.);
#2040=FACE_OUTER_BOUND('',#2943,.T.);
#2041=FACE_OUTER_BOUND('',#2944,.T.);
#2042=FACE_OUTER_BOUND('',#2946,.T.);
#2043=FACE_OUTER_BOUND('',#2947,.T.);
#2044=FACE_OUTER_BOUND('',#2948,.T.);
#2045=FACE_OUTER_BOUND('',#2949,.T.);
#2046=FACE_OUTER_BOUND('',#2950,.T.);
#2047=FACE_OUTER_BOUND('',#2951,.T.);
#2048=FACE_OUTER_BOUND('',#2952,.T.);
#2049=FACE_OUTER_BOUND('',#2954,.T.);
#2050=FACE_OUTER_BOUND('',#2955,.T.);
#2051=FACE_OUTER_BOUND('',#2957,.T.);
#2052=FACE_OUTER_BOUND('',#2958,.T.);
#2053=FACE_OUTER_BOUND('',#2959,.T.);
#2054=FACE_OUTER_BOUND('',#2960,.T.);
#2055=FACE_OUTER_BOUND('',#2962,.T.);
#2056=FACE_OUTER_BOUND('',#2963,.T.);
#2057=FACE_OUTER_BOUND('',#2964,.T.);
#2058=FACE_OUTER_BOUND('',#2965,.T.);
#2059=FACE_OUTER_BOUND('',#2967,.T.);
#2060=FACE_OUTER_BOUND('',#2968,.T.);
#2061=FACE_OUTER_BOUND('',#2969,.T.);
#2062=FACE_OUTER_BOUND('',#2970,.T.);
#2063=FACE_OUTER_BOUND('',#2971,.T.);
#2064=FACE_OUTER_BOUND('',#2972,.T.);
#2065=FACE_OUTER_BOUND('',#2973,.T.);
#2066=FACE_OUTER_BOUND('',#2974,.T.);
#2067=FACE_OUTER_BOUND('',#2975,.T.);
#2068=FACE_OUTER_BOUND('',#2976,.T.);
#2069=FACE_OUTER_BOUND('',#2977,.T.);
#2070=FACE_OUTER_BOUND('',#2978,.T.);
#2071=FACE_OUTER_BOUND('',#2979,.T.);
#2072=FACE_OUTER_BOUND('',#2980,.T.);
#2073=FACE_OUTER_BOUND('',#2981,.T.);
#2074=FACE_OUTER_BOUND('',#2982,.T.);
#2075=FACE_OUTER_BOUND('',#2983,.T.);
#2076=FACE_OUTER_BOUND('',#2984,.T.);
#2077=FACE_OUTER_BOUND('',#2985,.T.);
#2078=FACE_OUTER_BOUND('',#2986,.T.);
#2079=FACE_OUTER_BOUND('',#2987,.T.);
#2080=FACE_OUTER_BOUND('',#2988,.T.);
#2081=FACE_OUTER_BOUND('',#2989,.T.);
#2082=FACE_OUTER_BOUND('',#2990,.T.);
#2083=FACE_OUTER_BOUND('',#2991,.T.);
#2084=FACE_OUTER_BOUND('',#2992,.T.);
#2085=FACE_OUTER_BOUND('',#2993,.T.);
#2086=FACE_OUTER_BOUND('',#2995,.T.);
#2087=FACE_OUTER_BOUND('',#2996,.T.);
#2088=FACE_OUTER_BOUND('',#2998,.T.);
#2089=FACE_OUTER_BOUND('',#2999,.T.);
#2090=FACE_OUTER_BOUND('',#3001,.T.);
#2091=FACE_OUTER_BOUND('',#3002,.T.);
#2092=FACE_OUTER_BOUND('',#3004,.T.);
#2093=FACE_OUTER_BOUND('',#3005,.T.);
#2094=FACE_OUTER_BOUND('',#3007,.T.);
#2095=FACE_OUTER_BOUND('',#3008,.T.);
#2096=FACE_OUTER_BOUND('',#3009,.T.);
#2097=FACE_OUTER_BOUND('',#3010,.T.);
#2098=FACE_OUTER_BOUND('',#3011,.T.);
#2099=FACE_OUTER_BOUND('',#3012,.T.);
#2100=FACE_OUTER_BOUND('',#3013,.T.);
#2101=FACE_OUTER_BOUND('',#3014,.T.);
#2102=FACE_OUTER_BOUND('',#3015,.T.);
#2103=FACE_OUTER_BOUND('',#3017,.T.);
#2104=FACE_OUTER_BOUND('',#3019,.T.);
#2105=FACE_OUTER_BOUND('',#3020,.T.);
#2106=FACE_OUTER_BOUND('',#3021,.T.);
#2107=FACE_OUTER_BOUND('',#3023,.T.);
#2108=FACE_OUTER_BOUND('',#3025,.T.);
#2109=FACE_OUTER_BOUND('',#3026,.T.);
#2110=FACE_OUTER_BOUND('',#3027,.T.);
#2111=FACE_OUTER_BOUND('',#3028,.T.);
#2112=FACE_OUTER_BOUND('',#3030,.T.);
#2113=FACE_OUTER_BOUND('',#3032,.T.);
#2114=FACE_OUTER_BOUND('',#3033,.T.);
#2115=FACE_OUTER_BOUND('',#3034,.T.);
#2116=FACE_OUTER_BOUND('',#3036,.T.);
#2117=FACE_OUTER_BOUND('',#3038,.T.);
#2118=FACE_OUTER_BOUND('',#3039,.T.);
#2119=FACE_OUTER_BOUND('',#3040,.T.);
#2120=FACE_OUTER_BOUND('',#3042,.T.);
#2121=FACE_OUTER_BOUND('',#3044,.T.);
#2122=FACE_OUTER_BOUND('',#3045,.T.);
#2123=FACE_OUTER_BOUND('',#3046,.T.);
#2124=FACE_OUTER_BOUND('',#3047,.T.);
#2125=FACE_OUTER_BOUND('',#3048,.T.);
#2126=FACE_OUTER_BOUND('',#3050,.T.);
#2127=FACE_OUTER_BOUND('',#3053,.T.);
#2128=FACE_OUTER_BOUND('',#3055,.T.);
#2129=FACE_OUTER_BOUND('',#3057,.T.);
#2130=FACE_OUTER_BOUND('',#3058,.T.);
#2131=FACE_OUTER_BOUND('',#3059,.T.);
#2132=FACE_OUTER_BOUND('',#3060,.T.);
#2133=FACE_OUTER_BOUND('',#3061,.T.);
#2134=FACE_OUTER_BOUND('',#3062,.T.);
#2135=FACE_OUTER_BOUND('',#3063,.T.);
#2136=FACE_OUTER_BOUND('',#3064,.T.);
#2137=FACE_OUTER_BOUND('',#3065,.T.);
#2138=FACE_OUTER_BOUND('',#3067,.T.);
#2139=FACE_OUTER_BOUND('',#3069,.T.);
#2140=FACE_OUTER_BOUND('',#3070,.T.);
#2141=FACE_OUTER_BOUND('',#3071,.T.);
#2142=FACE_OUTER_BOUND('',#3072,.T.);
#2143=FACE_OUTER_BOUND('',#3074,.T.);
#2144=FACE_OUTER_BOUND('',#3075,.T.);
#2145=FACE_OUTER_BOUND('',#3076,.T.);
#2146=FACE_OUTER_BOUND('',#3078,.T.);
#2147=FACE_OUTER_BOUND('',#3079,.T.);
#2148=FACE_OUTER_BOUND('',#3080,.T.);
#2149=FACE_OUTER_BOUND('',#3081,.T.);
#2150=FACE_OUTER_BOUND('',#3082,.T.);
#2151=FACE_OUTER_BOUND('',#3083,.T.);
#2152=FACE_OUTER_BOUND('',#3084,.T.);
#2153=FACE_OUTER_BOUND('',#3085,.T.);
#2154=FACE_OUTER_BOUND('',#3086,.T.);
#2155=FACE_OUTER_BOUND('',#3087,.T.);
#2156=FACE_OUTER_BOUND('',#3088,.T.);
#2157=FACE_OUTER_BOUND('',#3089,.T.);
#2158=FACE_OUTER_BOUND('',#3090,.T.);
#2159=FACE_OUTER_BOUND('',#3091,.T.);
#2160=FACE_OUTER_BOUND('',#3092,.T.);
#2161=FACE_OUTER_BOUND('',#3093,.T.);
#2162=FACE_OUTER_BOUND('',#3094,.T.);
#2163=FACE_OUTER_BOUND('',#3095,.T.);
#2164=FACE_OUTER_BOUND('',#3096,.T.);
#2165=FACE_OUTER_BOUND('',#3097,.T.);
#2166=FACE_OUTER_BOUND('',#3098,.T.);
#2167=FACE_OUTER_BOUND('',#3099,.T.);
#2168=FACE_OUTER_BOUND('',#3100,.T.);
#2169=FACE_OUTER_BOUND('',#3101,.T.);
#2170=FACE_OUTER_BOUND('',#3102,.T.);
#2171=FACE_OUTER_BOUND('',#3103,.T.);
#2172=FACE_OUTER_BOUND('',#3104,.T.);
#2173=FACE_OUTER_BOUND('',#3105,.T.);
#2174=FACE_OUTER_BOUND('',#3106,.T.);
#2175=FACE_OUTER_BOUND('',#3107,.T.);
#2176=FACE_OUTER_BOUND('',#3108,.T.);
#2177=FACE_OUTER_BOUND('',#3109,.T.);
#2178=FACE_OUTER_BOUND('',#3110,.T.);
#2179=FACE_OUTER_BOUND('',#3111,.T.);
#2180=FACE_OUTER_BOUND('',#3112,.T.);
#2181=FACE_OUTER_BOUND('',#3113,.T.);
#2182=FACE_OUTER_BOUND('',#3114,.T.);
#2183=FACE_OUTER_BOUND('',#3115,.T.);
#2184=FACE_OUTER_BOUND('',#3116,.T.);
#2185=FACE_OUTER_BOUND('',#3117,.T.);
#2186=FACE_OUTER_BOUND('',#3118,.T.);
#2187=FACE_OUTER_BOUND('',#3119,.T.);
#2188=FACE_OUTER_BOUND('',#3120,.T.);
#2189=FACE_OUTER_BOUND('',#3121,.T.);
#2190=FACE_OUTER_BOUND('',#3122,.T.);
#2191=FACE_OUTER_BOUND('',#3123,.T.);
#2192=FACE_OUTER_BOUND('',#3124,.T.);
#2193=FACE_OUTER_BOUND('',#3125,.T.);
#2194=FACE_OUTER_BOUND('',#3126,.T.);
#2195=FACE_OUTER_BOUND('',#3127,.T.);
#2196=FACE_OUTER_BOUND('',#3128,.T.);
#2197=FACE_OUTER_BOUND('',#3129,.T.);
#2198=FACE_OUTER_BOUND('',#3130,.T.);
#2199=FACE_OUTER_BOUND('',#3131,.T.);
#2200=FACE_OUTER_BOUND('',#3132,.T.);
#2201=FACE_OUTER_BOUND('',#3133,.T.);
#2202=FACE_OUTER_BOUND('',#3134,.T.);
#2203=FACE_OUTER_BOUND('',#3135,.T.);
#2204=FACE_OUTER_BOUND('',#3136,.T.);
#2205=FACE_OUTER_BOUND('',#3137,.T.);
#2206=FACE_OUTER_BOUND('',#3138,.T.);
#2207=FACE_OUTER_BOUND('',#3139,.T.);
#2208=FACE_OUTER_BOUND('',#3140,.T.);
#2209=FACE_OUTER_BOUND('',#3141,.T.);
#2210=FACE_OUTER_BOUND('',#3142,.T.);
#2211=FACE_OUTER_BOUND('',#3143,.T.);
#2212=FACE_OUTER_BOUND('',#3144,.T.);
#2213=FACE_OUTER_BOUND('',#3145,.T.);
#2214=FACE_OUTER_BOUND('',#3146,.T.);
#2215=FACE_OUTER_BOUND('',#3147,.T.);
#2216=FACE_OUTER_BOUND('',#3148,.T.);
#2217=FACE_OUTER_BOUND('',#3149,.T.);
#2218=FACE_OUTER_BOUND('',#3150,.T.);
#2219=FACE_OUTER_BOUND('',#3151,.T.);
#2220=FACE_OUTER_BOUND('',#3152,.T.);
#2221=FACE_OUTER_BOUND('',#3153,.T.);
#2222=FACE_OUTER_BOUND('',#3154,.T.);
#2223=FACE_OUTER_BOUND('',#3155,.T.);
#2224=FACE_OUTER_BOUND('',#3156,.T.);
#2225=FACE_OUTER_BOUND('',#3157,.T.);
#2226=FACE_OUTER_BOUND('',#3159,.T.);
#2227=FACE_OUTER_BOUND('',#3160,.T.);
#2228=FACE_OUTER_BOUND('',#3161,.T.);
#2229=FACE_OUTER_BOUND('',#3162,.T.);
#2230=FACE_OUTER_BOUND('',#3163,.T.);
#2231=FACE_OUTER_BOUND('',#3164,.T.);
#2232=FACE_OUTER_BOUND('',#3165,.T.);
#2233=FACE_OUTER_BOUND('',#3166,.T.);
#2234=FACE_OUTER_BOUND('',#3167,.T.);
#2235=FACE_OUTER_BOUND('',#3169,.T.);
#2236=FACE_OUTER_BOUND('',#3171,.T.);
#2237=FACE_OUTER_BOUND('',#3172,.T.);
#2238=FACE_OUTER_BOUND('',#3173,.T.);
#2239=FACE_OUTER_BOUND('',#3175,.T.);
#2240=FACE_OUTER_BOUND('',#3177,.T.);
#2241=FACE_OUTER_BOUND('',#3178,.T.);
#2242=FACE_OUTER_BOUND('',#3179,.T.);
#2243=FACE_OUTER_BOUND('',#3180,.T.);
#2244=FACE_OUTER_BOUND('',#3182,.T.);
#2245=FACE_OUTER_BOUND('',#3184,.T.);
#2246=FACE_OUTER_BOUND('',#3185,.T.);
#2247=FACE_OUTER_BOUND('',#3186,.T.);
#2248=FACE_OUTER_BOUND('',#3188,.T.);
#2249=FACE_OUTER_BOUND('',#3190,.T.);
#2250=FACE_OUTER_BOUND('',#3191,.T.);
#2251=FACE_OUTER_BOUND('',#3193,.T.);
#2252=FACE_OUTER_BOUND('',#3195,.T.);
#2253=FACE_OUTER_BOUND('',#3197,.T.);
#2254=FACE_OUTER_BOUND('',#3199,.T.);
#2255=FACE_OUTER_BOUND('',#3200,.T.);
#2256=FACE_OUTER_BOUND('',#3201,.T.);
#2257=FACE_OUTER_BOUND('',#3202,.T.);
#2258=FACE_OUTER_BOUND('',#3203,.T.);
#2259=FACE_OUTER_BOUND('',#3204,.T.);
#2260=FACE_OUTER_BOUND('',#3205,.T.);
#2261=FACE_OUTER_BOUND('',#3206,.T.);
#2262=FACE_OUTER_BOUND('',#3207,.T.);
#2263=FACE_OUTER_BOUND('',#3209,.T.);
#2264=FACE_OUTER_BOUND('',#3211,.T.);
#2265=FACE_OUTER_BOUND('',#3212,.T.);
#2266=FACE_OUTER_BOUND('',#3213,.T.);
#2267=FACE_OUTER_BOUND('',#3214,.T.);
#2268=FACE_OUTER_BOUND('',#3215,.T.);
#2269=FACE_OUTER_BOUND('',#3216,.T.);
#2270=FACE_OUTER_BOUND('',#3217,.T.);
#2271=FACE_OUTER_BOUND('',#3218,.T.);
#2272=FACE_OUTER_BOUND('',#3219,.T.);
#2273=FACE_OUTER_BOUND('',#3221,.T.);
#2274=FACE_OUTER_BOUND('',#3222,.T.);
#2275=FACE_OUTER_BOUND('',#3223,.T.);
#2276=FACE_OUTER_BOUND('',#3224,.T.);
#2277=FACE_OUTER_BOUND('',#3225,.T.);
#2278=FACE_OUTER_BOUND('',#3226,.T.);
#2279=FACE_OUTER_BOUND('',#3228,.T.);
#2280=FACE_OUTER_BOUND('',#3229,.T.);
#2281=FACE_OUTER_BOUND('',#3230,.T.);
#2282=FACE_OUTER_BOUND('',#3232,.T.);
#2283=FACE_OUTER_BOUND('',#3233,.T.);
#2284=FACE_OUTER_BOUND('',#3234,.T.);
#2285=FACE_OUTER_BOUND('',#3235,.T.);
#2286=FACE_OUTER_BOUND('',#3236,.T.);
#2287=FACE_OUTER_BOUND('',#3237,.T.);
#2288=FACE_OUTER_BOUND('',#3238,.T.);
#2289=FACE_OUTER_BOUND('',#3239,.T.);
#2290=FACE_OUTER_BOUND('',#3240,.T.);
#2291=FACE_OUTER_BOUND('',#3241,.T.);
#2292=FACE_OUTER_BOUND('',#3242,.T.);
#2293=FACE_OUTER_BOUND('',#3243,.T.);
#2294=FACE_OUTER_BOUND('',#3244,.T.);
#2295=FACE_OUTER_BOUND('',#3245,.T.);
#2296=FACE_OUTER_BOUND('',#3246,.T.);
#2297=FACE_OUTER_BOUND('',#3247,.T.);
#2298=FACE_OUTER_BOUND('',#3248,.T.);
#2299=FACE_OUTER_BOUND('',#3249,.T.);
#2300=FACE_OUTER_BOUND('',#3250,.T.);
#2301=FACE_OUTER_BOUND('',#3251,.T.);
#2302=FACE_OUTER_BOUND('',#3252,.T.);
#2303=FACE_OUTER_BOUND('',#3253,.T.);
#2304=FACE_OUTER_BOUND('',#3254,.T.);
#2305=FACE_OUTER_BOUND('',#3255,.T.);
#2306=FACE_OUTER_BOUND('',#3256,.T.);
#2307=FACE_OUTER_BOUND('',#3257,.T.);
#2308=FACE_OUTER_BOUND('',#3258,.T.);
#2309=FACE_OUTER_BOUND('',#3259,.T.);
#2310=FACE_OUTER_BOUND('',#3260,.T.);
#2311=FACE_OUTER_BOUND('',#3261,.T.);
#2312=FACE_OUTER_BOUND('',#3262,.T.);
#2313=FACE_OUTER_BOUND('',#3263,.T.);
#2314=FACE_OUTER_BOUND('',#3264,.T.);
#2315=FACE_OUTER_BOUND('',#3265,.T.);
#2316=FACE_OUTER_BOUND('',#3266,.T.);
#2317=FACE_OUTER_BOUND('',#3267,.T.);
#2318=FACE_OUTER_BOUND('',#3268,.T.);
#2319=FACE_OUTER_BOUND('',#3269,.T.);
#2320=FACE_OUTER_BOUND('',#3270,.T.);
#2321=FACE_OUTER_BOUND('',#3271,.T.);
#2322=FACE_OUTER_BOUND('',#3272,.T.);
#2323=FACE_OUTER_BOUND('',#3273,.T.);
#2324=FACE_OUTER_BOUND('',#3274,.T.);
#2325=FACE_OUTER_BOUND('',#3275,.T.);
#2326=FACE_OUTER_BOUND('',#3276,.T.);
#2327=FACE_OUTER_BOUND('',#3277,.T.);
#2328=FACE_OUTER_BOUND('',#3278,.T.);
#2329=FACE_OUTER_BOUND('',#3279,.T.);
#2330=FACE_OUTER_BOUND('',#3280,.T.);
#2331=FACE_OUTER_BOUND('',#3281,.T.);
#2332=FACE_OUTER_BOUND('',#3282,.T.);
#2333=FACE_OUTER_BOUND('',#3283,.T.);
#2334=FACE_OUTER_BOUND('',#3284,.T.);
#2335=FACE_OUTER_BOUND('',#3285,.T.);
#2336=FACE_OUTER_BOUND('',#3286,.T.);
#2337=FACE_OUTER_BOUND('',#3287,.T.);
#2338=FACE_OUTER_BOUND('',#3288,.T.);
#2339=FACE_OUTER_BOUND('',#3289,.T.);
#2340=FACE_OUTER_BOUND('',#3290,.T.);
#2341=FACE_OUTER_BOUND('',#3291,.T.);
#2342=FACE_OUTER_BOUND('',#3292,.T.);
#2343=FACE_OUTER_BOUND('',#3293,.T.);
#2344=FACE_OUTER_BOUND('',#3294,.T.);
#2345=FACE_OUTER_BOUND('',#3295,.T.);
#2346=FACE_OUTER_BOUND('',#3296,.T.);
#2347=FACE_OUTER_BOUND('',#3297,.T.);
#2348=FACE_OUTER_BOUND('',#3298,.T.);
#2349=FACE_OUTER_BOUND('',#3299,.T.);
#2350=FACE_OUTER_BOUND('',#3300,.T.);
#2351=FACE_OUTER_BOUND('',#3301,.T.);
#2352=FACE_OUTER_BOUND('',#3302,.T.);
#2353=FACE_OUTER_BOUND('',#3303,.T.);
#2354=FACE_OUTER_BOUND('',#3304,.T.);
#2355=FACE_OUTER_BOUND('',#3305,.T.);
#2356=FACE_OUTER_BOUND('',#3306,.T.);
#2357=FACE_OUTER_BOUND('',#3307,.T.);
#2358=FACE_OUTER_BOUND('',#3308,.T.);
#2359=FACE_OUTER_BOUND('',#3309,.T.);
#2360=FACE_OUTER_BOUND('',#3310,.T.);
#2361=FACE_OUTER_BOUND('',#3311,.T.);
#2362=FACE_OUTER_BOUND('',#3312,.T.);
#2363=FACE_OUTER_BOUND('',#3313,.T.);
#2364=FACE_OUTER_BOUND('',#3314,.T.);
#2365=FACE_OUTER_BOUND('',#3315,.T.);
#2366=FACE_OUTER_BOUND('',#3316,.T.);
#2367=FACE_OUTER_BOUND('',#3317,.T.);
#2368=FACE_OUTER_BOUND('',#3318,.T.);
#2369=FACE_OUTER_BOUND('',#3319,.T.);
#2370=FACE_OUTER_BOUND('',#3320,.T.);
#2371=FACE_OUTER_BOUND('',#3321,.T.);
#2372=FACE_OUTER_BOUND('',#3322,.T.);
#2373=FACE_OUTER_BOUND('',#3323,.T.);
#2374=FACE_OUTER_BOUND('',#3324,.T.);
#2375=FACE_OUTER_BOUND('',#3325,.T.);
#2376=FACE_OUTER_BOUND('',#3326,.T.);
#2377=FACE_OUTER_BOUND('',#3327,.T.);
#2378=FACE_OUTER_BOUND('',#3328,.T.);
#2379=FACE_OUTER_BOUND('',#3329,.T.);
#2380=FACE_OUTER_BOUND('',#3330,.T.);
#2381=FACE_OUTER_BOUND('',#3331,.T.);
#2382=FACE_OUTER_BOUND('',#3332,.T.);
#2383=FACE_OUTER_BOUND('',#3333,.T.);
#2384=FACE_OUTER_BOUND('',#3334,.T.);
#2385=FACE_OUTER_BOUND('',#3335,.T.);
#2386=FACE_OUTER_BOUND('',#3336,.T.);
#2387=FACE_OUTER_BOUND('',#3337,.T.);
#2388=FACE_OUTER_BOUND('',#3338,.T.);
#2389=FACE_OUTER_BOUND('',#3339,.T.);
#2390=FACE_OUTER_BOUND('',#3340,.T.);
#2391=FACE_OUTER_BOUND('',#3341,.T.);
#2392=FACE_OUTER_BOUND('',#3342,.T.);
#2393=FACE_OUTER_BOUND('',#3343,.T.);
#2394=FACE_OUTER_BOUND('',#3344,.T.);
#2395=FACE_OUTER_BOUND('',#3345,.T.);
#2396=FACE_OUTER_BOUND('',#3346,.T.);
#2397=FACE_OUTER_BOUND('',#3347,.T.);
#2398=FACE_OUTER_BOUND('',#3348,.T.);
#2399=FACE_OUTER_BOUND('',#3349,.T.);
#2400=FACE_OUTER_BOUND('',#3350,.T.);
#2401=FACE_OUTER_BOUND('',#3351,.T.);
#2402=FACE_OUTER_BOUND('',#3352,.T.);
#2403=FACE_OUTER_BOUND('',#3353,.T.);
#2404=FACE_OUTER_BOUND('',#3354,.T.);
#2405=FACE_OUTER_BOUND('',#3355,.T.);
#2406=FACE_OUTER_BOUND('',#3356,.T.);
#2407=FACE_OUTER_BOUND('',#3357,.T.);
#2408=FACE_OUTER_BOUND('',#3358,.T.);
#2409=FACE_OUTER_BOUND('',#3359,.T.);
#2410=FACE_OUTER_BOUND('',#3360,.T.);
#2411=FACE_OUTER_BOUND('',#3361,.T.);
#2412=FACE_OUTER_BOUND('',#3362,.T.);
#2413=FACE_OUTER_BOUND('',#3363,.T.);
#2414=FACE_OUTER_BOUND('',#3364,.T.);
#2415=FACE_OUTER_BOUND('',#3365,.T.);
#2416=FACE_OUTER_BOUND('',#3366,.T.);
#2417=FACE_OUTER_BOUND('',#3367,.T.);
#2418=FACE_OUTER_BOUND('',#3368,.T.);
#2419=FACE_OUTER_BOUND('',#3369,.T.);
#2420=FACE_OUTER_BOUND('',#3370,.T.);
#2421=FACE_OUTER_BOUND('',#3371,.T.);
#2422=FACE_OUTER_BOUND('',#3372,.T.);
#2423=FACE_OUTER_BOUND('',#3373,.T.);
#2424=FACE_OUTER_BOUND('',#3374,.T.);
#2425=FACE_OUTER_BOUND('',#3375,.T.);
#2426=FACE_OUTER_BOUND('',#3376,.T.);
#2427=FACE_OUTER_BOUND('',#3377,.T.);
#2428=FACE_OUTER_BOUND('',#3378,.T.);
#2429=FACE_OUTER_BOUND('',#3379,.T.);
#2430=FACE_OUTER_BOUND('',#3380,.T.);
#2431=FACE_OUTER_BOUND('',#3381,.T.);
#2432=FACE_OUTER_BOUND('',#3382,.T.);
#2433=FACE_OUTER_BOUND('',#3383,.T.);
#2434=FACE_OUTER_BOUND('',#3384,.T.);
#2435=FACE_OUTER_BOUND('',#3385,.T.);
#2436=FACE_OUTER_BOUND('',#3386,.T.);
#2437=FACE_OUTER_BOUND('',#3387,.T.);
#2438=FACE_OUTER_BOUND('',#3388,.T.);
#2439=FACE_OUTER_BOUND('',#3389,.T.);
#2440=FACE_OUTER_BOUND('',#3390,.T.);
#2441=FACE_OUTER_BOUND('',#3391,.T.);
#2442=FACE_OUTER_BOUND('',#3393,.T.);
#2443=FACE_OUTER_BOUND('',#3394,.T.);
#2444=FACE_OUTER_BOUND('',#3395,.T.);
#2445=FACE_OUTER_BOUND('',#3396,.T.);
#2446=FACE_OUTER_BOUND('',#3397,.T.);
#2447=FACE_OUTER_BOUND('',#3398,.T.);
#2448=FACE_OUTER_BOUND('',#3399,.T.);
#2449=FACE_OUTER_BOUND('',#3400,.T.);
#2450=FACE_OUTER_BOUND('',#3401,.T.);
#2451=FACE_OUTER_BOUND('',#3402,.T.);
#2452=FACE_OUTER_BOUND('',#3403,.T.);
#2453=FACE_OUTER_BOUND('',#3404,.T.);
#2454=FACE_OUTER_BOUND('',#3405,.T.);
#2455=FACE_OUTER_BOUND('',#3406,.T.);
#2456=FACE_OUTER_BOUND('',#3407,.T.);
#2457=FACE_OUTER_BOUND('',#3409,.T.);
#2458=FACE_OUTER_BOUND('',#3410,.T.);
#2459=EDGE_LOOP('',(#8879,#8880,#8881,#8882));
#2460=EDGE_LOOP('',(#8883,#8884,#8885,#8886));
#2461=EDGE_LOOP('',(#8887,#8888,#8889,#8890));
#2462=EDGE_LOOP('',(#8891,#8892,#8893,#8894));
#2463=EDGE_LOOP('',(#8895,#8896,#8897,#8898));
#2464=EDGE_LOOP('',(#8899,#8900,#8901,#8902));
#2465=EDGE_LOOP('',(#8903,#8904,#8905,#8906));
#2466=EDGE_LOOP('',(#8907,#8908,#8909,#8910));
#2467=EDGE_LOOP('',(#8911,#8912,#8913,#8914));
#2468=EDGE_LOOP('',(#8915,#8916,#8917,#8918));
#2469=EDGE_LOOP('',(#8919,#8920,#8921,#8922));
#2470=EDGE_LOOP('',(#8923,#8924,#8925,#8926));
#2471=EDGE_LOOP('',(#8927,#8928,#8929,#8930));
#2472=EDGE_LOOP('',(#8931,#8932,#8933,#8934));
#2473=EDGE_LOOP('',(#8935,#8936,#8937,#8938));
#2474=EDGE_LOOP('',(#8939,#8940,#8941,#8942));
#2475=EDGE_LOOP('',(#8943,#8944,#8945,#8946));
#2476=EDGE_LOOP('',(#8947));
#2477=EDGE_LOOP('',(#8948));
#2478=EDGE_LOOP('',(#8949));
#2479=EDGE_LOOP('',(#8950));
#2480=EDGE_LOOP('',(#8951));
#2481=EDGE_LOOP('',(#8952));
#2482=EDGE_LOOP('',(#8953));
#2483=EDGE_LOOP('',(#8954));
#2484=EDGE_LOOP('',(#8955));
#2485=EDGE_LOOP('',(#8956));
#2486=EDGE_LOOP('',(#8957));
#2487=EDGE_LOOP('',(#8958));
#2488=EDGE_LOOP('',(#8959,#8960,#8961,#8962));
#2489=EDGE_LOOP('',(#8963));
#2490=EDGE_LOOP('',(#8964));
#2491=EDGE_LOOP('',(#8965));
#2492=EDGE_LOOP('',(#8966));
#2493=EDGE_LOOP('',(#8967));
#2494=EDGE_LOOP('',(#8968));
#2495=EDGE_LOOP('',(#8969));
#2496=EDGE_LOOP('',(#8970));
#2497=EDGE_LOOP('',(#8971));
#2498=EDGE_LOOP('',(#8972));
#2499=EDGE_LOOP('',(#8973));
#2500=EDGE_LOOP('',(#8974));
#2501=EDGE_LOOP('',(#8975,#8976,#8977,#8978));
#2502=EDGE_LOOP('',(#8979,#8980,#8981,#8982));
#2503=EDGE_LOOP('',(#8983,#8984,#8985,#8986));
#2504=EDGE_LOOP('',(#8987,#8988,#8989,#8990));
#2505=EDGE_LOOP('',(#8991,#8992,#8993,#8994));
#2506=EDGE_LOOP('',(#8995,#8996,#8997,#8998));
#2507=EDGE_LOOP('',(#8999,#9000,#9001,#9002));
#2508=EDGE_LOOP('',(#9003,#9004,#9005,#9006));
#2509=EDGE_LOOP('',(#9007,#9008,#9009,#9010));
#2510=EDGE_LOOP('',(#9011,#9012,#9013,#9014));
#2511=EDGE_LOOP('',(#9015,#9016,#9017,#9018));
#2512=EDGE_LOOP('',(#9019,#9020,#9021,#9022));
#2513=EDGE_LOOP('',(#9023,#9024,#9025,#9026,#9027,#9028));
#2514=EDGE_LOOP('',(#9029,#9030,#9031,#9032));
#2515=EDGE_LOOP('',(#9033));
#2516=EDGE_LOOP('',(#9034,#9035,#9036,#9037));
#2517=EDGE_LOOP('',(#9038));
#2518=EDGE_LOOP('',(#9039,#9040,#9041,#9042));
#2519=EDGE_LOOP('',(#9043));
#2520=EDGE_LOOP('',(#9044,#9045,#9046,#9047));
#2521=EDGE_LOOP('',(#9048));
#2522=EDGE_LOOP('',(#9049,#9050));
#2523=EDGE_LOOP('',(#9051,#9052,#9053,#9054));
#2524=EDGE_LOOP('',(#9055,#9056,#9057,#9058));
#2525=EDGE_LOOP('',(#9059,#9060));
#2526=EDGE_LOOP('',(#9061,#9062,#9063,#9064));
#2527=EDGE_LOOP('',(#9065,#9066));
#2528=EDGE_LOOP('',(#9067,#9068,#9069,#9070));
#2529=EDGE_LOOP('',(#9071,#9072));
#2530=EDGE_LOOP('',(#9073,#9074,#9075,#9076,#9077,#9078,#9079,#9080,#9081,
#9082,#9083,#9084,#9085,#9086,#9087,#9088,#9089,#9090,#9091,#9092));
#2531=EDGE_LOOP('',(#9093,#9094));
#2532=EDGE_LOOP('',(#9095));
#2533=EDGE_LOOP('',(#9096,#9097,#9098,#9099,#9100,#9101,#9102,#9103,#9104));
#2534=EDGE_LOOP('',(#9105));
#2535=EDGE_LOOP('',(#9106));
#2536=EDGE_LOOP('',(#9107));
#2537=EDGE_LOOP('',(#9108));
#2538=EDGE_LOOP('',(#9109,#9110,#9111,#9112));
#2539=EDGE_LOOP('',(#9113,#9114,#9115,#9116));
#2540=EDGE_LOOP('',(#9117,#9118,#9119,#9120));
#2541=EDGE_LOOP('',(#9121,#9122,#9123,#9124));
#2542=EDGE_LOOP('',(#9125,#9126,#9127,#9128));
#2543=EDGE_LOOP('',(#9129));
#2544=EDGE_LOOP('',(#9130));
#2545=EDGE_LOOP('',(#9131,#9132,#9133,#9134));
#2546=EDGE_LOOP('',(#9135,#9136,#9137,#9138));
#2547=EDGE_LOOP('',(#9139,#9140));
#2548=EDGE_LOOP('',(#9141));
#2549=EDGE_LOOP('',(#9142));
#2550=EDGE_LOOP('',(#9143));
#2551=EDGE_LOOP('',(#9144));
#2552=EDGE_LOOP('',(#9145));
#2553=EDGE_LOOP('',(#9146));
#2554=EDGE_LOOP('',(#9147));
#2555=EDGE_LOOP('',(#9148));
#2556=EDGE_LOOP('',(#9149));
#2557=EDGE_LOOP('',(#9150));
#2558=EDGE_LOOP('',(#9151));
#2559=EDGE_LOOP('',(#9152));
#2560=EDGE_LOOP('',(#9153,#9154,#9155,#9156));
#2561=EDGE_LOOP('',(#9157,#9158,#9159,#9160));
#2562=EDGE_LOOP('',(#9161));
#2563=EDGE_LOOP('',(#9162));
#2564=EDGE_LOOP('',(#9163));
#2565=EDGE_LOOP('',(#9164));
#2566=EDGE_LOOP('',(#9165,#9166,#9167,#9168));
#2567=EDGE_LOOP('',(#9169,#9170,#9171,#9172));
#2568=EDGE_LOOP('',(#9173,#9174,#9175,#9176));
#2569=EDGE_LOOP('',(#9177,#9178,#9179,#9180));
#2570=EDGE_LOOP('',(#9181,#9182,#9183,#9184,#9185,#9186,#9187,#9188));
#2571=EDGE_LOOP('',(#9189));
#2572=EDGE_LOOP('',(#9190,#9191,#9192,#9193));
#2573=EDGE_LOOP('',(#9194,#9195,#9196,#9197));
#2574=EDGE_LOOP('',(#9198,#9199,#9200,#9201));
#2575=EDGE_LOOP('',(#9202,#9203,#9204,#9205));
#2576=EDGE_LOOP('',(#9206,#9207,#9208,#9209));
#2577=EDGE_LOOP('',(#9210));
#2578=EDGE_LOOP('',(#9211));
#2579=EDGE_LOOP('',(#9212,#9213,#9214,#9215));
#2580=EDGE_LOOP('',(#9216,#9217,#9218,#9219,#9220,#9221,#9222,#9223));
#2581=EDGE_LOOP('',(#9224));
#2582=EDGE_LOOP('',(#9225,#9226,#9227,#9228));
#2583=EDGE_LOOP('',(#9229,#9230,#9231,#9232));
#2584=EDGE_LOOP('',(#9233,#9234,#9235,#9236));
#2585=EDGE_LOOP('',(#9237,#9238,#9239,#9240));
#2586=EDGE_LOOP('',(#9241,#9242,#9243,#9244));
#2587=EDGE_LOOP('',(#9245));
#2588=EDGE_LOOP('',(#9246,#9247,#9248,#9249));
#2589=EDGE_LOOP('',(#9250));
#2590=EDGE_LOOP('',(#9251));
#2591=EDGE_LOOP('',(#9252));
#2592=EDGE_LOOP('',(#9253));
#2593=EDGE_LOOP('',(#9254));
#2594=EDGE_LOOP('',(#9255));
#2595=EDGE_LOOP('',(#9256));
#2596=EDGE_LOOP('',(#9257));
#2597=EDGE_LOOP('',(#9258));
#2598=EDGE_LOOP('',(#9259));
#2599=EDGE_LOOP('',(#9260));
#2600=EDGE_LOOP('',(#9261,#9262));
#2601=EDGE_LOOP('',(#9263,#9264,#9265,#9266,#9267,#9268,#9269,#9270));
#2602=EDGE_LOOP('',(#9271,#9272));
#2603=EDGE_LOOP('',(#9273,#9274,#9275,#9276,#9277,#9278,#9279,#9280,#9281,
#9282,#9283,#9284,#9285,#9286,#9287,#9288,#9289,#9290,#9291,#9292,#9293,
#9294,#9295,#9296));
#2604=EDGE_LOOP('',(#9297,#9298,#9299,#9300,#9301,#9302,#9303,#9304,#9305));
#2605=EDGE_LOOP('',(#9306,#9307,#9308,#9309));
#2606=EDGE_LOOP('',(#9310,#9311,#9312));
#2607=EDGE_LOOP('',(#9313,#9314,#9315,#9316));
#2608=EDGE_LOOP('',(#9317,#9318,#9319,#9320));
#2609=EDGE_LOOP('',(#9321,#9322,#9323,#9324));
#2610=EDGE_LOOP('',(#9325,#9326,#9327,#9328));
#2611=EDGE_LOOP('',(#9329,#9330,#9331,#9332));
#2612=EDGE_LOOP('',(#9333,#9334,#9335,#9336));
#2613=EDGE_LOOP('',(#9337,#9338,#9339));
#2614=EDGE_LOOP('',(#9340,#9341,#9342));
#2615=EDGE_LOOP('',(#9343,#9344,#9345,#9346));
#2616=EDGE_LOOP('',(#9347,#9348,#9349,#9350,#9351,#9352,#9353,#9354));
#2617=EDGE_LOOP('',(#9355));
#2618=EDGE_LOOP('',(#9356,#9357,#9358,#9359));
#2619=EDGE_LOOP('',(#9360,#9361,#9362,#9363,#9364));
#2620=EDGE_LOOP('',(#9365,#9366,#9367,#9368));
#2621=EDGE_LOOP('',(#9369,#9370,#9371,#9372,#9373,#9374,#9375,#9376,#9377));
#2622=EDGE_LOOP('',(#9378,#9379,#9380,#9381));
#2623=EDGE_LOOP('',(#9382,#9383,#9384,#9385));
#2624=EDGE_LOOP('',(#9386,#9387,#9388,#9389));
#2625=EDGE_LOOP('',(#9390));
#2626=EDGE_LOOP('',(#9391,#9392,#9393));
#2627=EDGE_LOOP('',(#9394,#9395,#9396,#9397,#9398,#9399,#9400,#9401));
#2628=EDGE_LOOP('',(#9402));
#2629=EDGE_LOOP('',(#9403,#9404,#9405,#9406));
#2630=EDGE_LOOP('',(#9407,#9408,#9409,#9410));
#2631=EDGE_LOOP('',(#9411));
#2632=EDGE_LOOP('',(#9412));
#2633=EDGE_LOOP('',(#9413));
#2634=EDGE_LOOP('',(#9414));
#2635=EDGE_LOOP('',(#9415,#9416,#9417,#9418));
#2636=EDGE_LOOP('',(#9419));
#2637=EDGE_LOOP('',(#9420));
#2638=EDGE_LOOP('',(#9421,#9422,#9423,#9424));
#2639=EDGE_LOOP('',(#9425));
#2640=EDGE_LOOP('',(#9426));
#2641=EDGE_LOOP('',(#9427,#9428,#9429,#9430));
#2642=EDGE_LOOP('',(#9431));
#2643=EDGE_LOOP('',(#9432));
#2644=EDGE_LOOP('',(#9433,#9434,#9435,#9436));
#2645=EDGE_LOOP('',(#9437));
#2646=EDGE_LOOP('',(#9438));
#2647=EDGE_LOOP('',(#9439,#9440,#9441,#9442));
#2648=EDGE_LOOP('',(#9443));
#2649=EDGE_LOOP('',(#9444));
#2650=EDGE_LOOP('',(#9445,#9446,#9447,#9448));
#2651=EDGE_LOOP('',(#9449));
#2652=EDGE_LOOP('',(#9450));
#2653=EDGE_LOOP('',(#9451,#9452,#9453,#9454));
#2654=EDGE_LOOP('',(#9455,#9456,#9457,#9458));
#2655=EDGE_LOOP('',(#9459,#9460,#9461,#9462));
#2656=EDGE_LOOP('',(#9463,#9464,#9465,#9466));
#2657=EDGE_LOOP('',(#9467,#9468,#9469,#9470));
#2658=EDGE_LOOP('',(#9471,#9472,#9473,#9474));
#2659=EDGE_LOOP('',(#9475,#9476,#9477,#9478));
#2660=EDGE_LOOP('',(#9479,#9480,#9481,#9482));
#2661=EDGE_LOOP('',(#9483,#9484,#9485,#9486));
#2662=EDGE_LOOP('',(#9487));
#2663=EDGE_LOOP('',(#9488));
#2664=EDGE_LOOP('',(#9489));
#2665=EDGE_LOOP('',(#9490));
#2666=EDGE_LOOP('',(#9491,#9492,#9493,#9494));
#2667=EDGE_LOOP('',(#9495,#9496,#9497,#9498));
#2668=EDGE_LOOP('',(#9499,#9500,#9501,#9502));
#2669=EDGE_LOOP('',(#9503,#9504,#9505,#9506));
#2670=EDGE_LOOP('',(#9507,#9508,#9509,#9510));
#2671=EDGE_LOOP('',(#9511,#9512,#9513,#9514));
#2672=EDGE_LOOP('',(#9515));
#2673=EDGE_LOOP('',(#9516));
#2674=EDGE_LOOP('',(#9517));
#2675=EDGE_LOOP('',(#9518));
#2676=EDGE_LOOP('',(#9519,#9520,#9521,#9522));
#2677=EDGE_LOOP('',(#9523,#9524,#9525,#9526,#9527,#9528,#9529,#9530,#9531,
#9532,#9533,#9534));
#2678=EDGE_LOOP('',(#9535,#9536,#9537,#9538,#9539,#9540,#9541,#9542,#9543,
#9544,#9545,#9546));
#2679=EDGE_LOOP('',(#9547,#9548,#9549,#9550,#9551,#9552));
#2680=EDGE_LOOP('',(#9553,#9554,#9555,#9556,#9557));
#2681=EDGE_LOOP('',(#9558,#9559,#9560,#9561));
#2682=EDGE_LOOP('',(#9562,#9563,#9564,#9565));
#2683=EDGE_LOOP('',(#9566));
#2684=EDGE_LOOP('',(#9567));
#2685=EDGE_LOOP('',(#9568,#9569,#9570,#9571,#9572));
#2686=EDGE_LOOP('',(#9573));
#2687=EDGE_LOOP('',(#9574));
#2688=EDGE_LOOP('',(#9575,#9576,#9577,#9578));
#2689=EDGE_LOOP('',(#9579,#9580,#9581,#9582,#9583,#9584));
#2690=EDGE_LOOP('',(#9585,#9586,#9587,#9588,#9589));
#2691=EDGE_LOOP('',(#9590));
#2692=EDGE_LOOP('',(#9591));
#2693=EDGE_LOOP('',(#9592,#9593,#9594,#9595));
#2694=EDGE_LOOP('',(#9596,#9597,#9598,#9599));
#2695=EDGE_LOOP('',(#9600,#9601,#9602,#9603));
#2696=EDGE_LOOP('',(#9604));
#2697=EDGE_LOOP('',(#9605));
#2698=EDGE_LOOP('',(#9606,#9607,#9608,#9609,#9610));
#2699=EDGE_LOOP('',(#9611,#9612));
#2700=EDGE_LOOP('',(#9613,#9614));
#2701=EDGE_LOOP('',(#9615,#9616));
#2702=EDGE_LOOP('',(#9617,#9618));
#2703=EDGE_LOOP('',(#9619,#9620));
#2704=EDGE_LOOP('',(#9621,#9622));
#2705=EDGE_LOOP('',(#9623,#9624));
#2706=EDGE_LOOP('',(#9625,#9626,#9627,#9628));
#2707=EDGE_LOOP('',(#9629,#9630,#9631,#9632,#9633,#9634,#9635,#9636,#9637,
#9638,#9639,#9640,#9641,#9642,#9643,#9644,#9645,#9646));
#2708=EDGE_LOOP('',(#9647,#9648,#9649,#9650));
#2709=EDGE_LOOP('',(#9651,#9652,#9653,#9654));
#2710=EDGE_LOOP('',(#9655,#9656,#9657,#9658));
#2711=EDGE_LOOP('',(#9659,#9660,#9661,#9662));
#2712=EDGE_LOOP('',(#9663,#9664,#9665,#9666,#9667,#9668));
#2713=EDGE_LOOP('',(#9669,#9670,#9671,#9672));
#2714=EDGE_LOOP('',(#9673,#9674,#9675,#9676));
#2715=EDGE_LOOP('',(#9677,#9678,#9679,#9680));
#2716=EDGE_LOOP('',(#9681,#9682,#9683,#9684));
#2717=EDGE_LOOP('',(#9685,#9686,#9687,#9688));
#2718=EDGE_LOOP('',(#9689,#9690,#9691,#9692,#9693,#9694,#9695,#9696,#9697,
#9698,#9699,#9700,#9701,#9702,#9703,#9704,#9705,#9706));
#2719=EDGE_LOOP('',(#9707,#9708,#9709,#9710));
#2720=EDGE_LOOP('',(#9711,#9712,#9713,#9714));
#2721=EDGE_LOOP('',(#9715));
#2722=EDGE_LOOP('',(#9716));
#2723=EDGE_LOOP('',(#9717,#9718,#9719,#9720));
#2724=EDGE_LOOP('',(#9721));
#2725=EDGE_LOOP('',(#9722));
#2726=EDGE_LOOP('',(#9723,#9724,#9725,#9726));
#2727=EDGE_LOOP('',(#9727));
#2728=EDGE_LOOP('',(#9728));
#2729=EDGE_LOOP('',(#9729,#9730,#9731,#9732));
#2730=EDGE_LOOP('',(#9733));
#2731=EDGE_LOOP('',(#9734));
#2732=EDGE_LOOP('',(#9735,#9736,#9737,#9738));
#2733=EDGE_LOOP('',(#9739));
#2734=EDGE_LOOP('',(#9740));
#2735=EDGE_LOOP('',(#9741,#9742,#9743,#9744));
#2736=EDGE_LOOP('',(#9745));
#2737=EDGE_LOOP('',(#9746,#9747,#9748,#9749));
#2738=EDGE_LOOP('',(#9750,#9751,#9752,#9753));
#2739=EDGE_LOOP('',(#9754,#9755,#9756,#9757));
#2740=EDGE_LOOP('',(#9758));
#2741=EDGE_LOOP('',(#9759));
#2742=EDGE_LOOP('',(#9760,#9761,#9762,#9763));
#2743=EDGE_LOOP('',(#9764,#9765,#9766,#9767));
#2744=EDGE_LOOP('',(#9768,#9769,#9770,#9771));
#2745=EDGE_LOOP('',(#9772));
#2746=EDGE_LOOP('',(#9773,#9774,#9775,#9776));
#2747=EDGE_LOOP('',(#9777,#9778,#9779,#9780));
#2748=EDGE_LOOP('',(#9781,#9782,#9783,#9784));
#2749=EDGE_LOOP('',(#9785,#9786,#9787,#9788));
#2750=EDGE_LOOP('',(#9789,#9790,#9791,#9792));
#2751=EDGE_LOOP('',(#9793,#9794,#9795,#9796));
#2752=EDGE_LOOP('',(#9797,#9798,#9799,#9800,#9801,#9802));
#2753=EDGE_LOOP('',(#9803,#9804,#9805,#9806,#9807,#9808));
#2754=EDGE_LOOP('',(#9809,#9810,#9811,#9812));
#2755=EDGE_LOOP('',(#9813,#9814,#9815,#9816));
#2756=EDGE_LOOP('',(#9817,#9818,#9819,#9820));
#2757=EDGE_LOOP('',(#9821,#9822,#9823,#9824));
#2758=EDGE_LOOP('',(#9825,#9826,#9827,#9828));
#2759=EDGE_LOOP('',(#9829,#9830,#9831,#9832));
#2760=EDGE_LOOP('',(#9833));
#2761=EDGE_LOOP('',(#9834,#9835,#9836,#9837));
#2762=EDGE_LOOP('',(#9838,#9839,#9840,#9841));
#2763=EDGE_LOOP('',(#9842));
#2764=EDGE_LOOP('',(#9843,#9844,#9845,#9846));
#2765=EDGE_LOOP('',(#9847,#9848,#9849,#9850));
#2766=EDGE_LOOP('',(#9851,#9852,#9853,#9854));
#2767=EDGE_LOOP('',(#9855,#9856,#9857,#9858));
#2768=EDGE_LOOP('',(#9859,#9860,#9861,#9862));
#2769=EDGE_LOOP('',(#9863,#9864,#9865,#9866));
#2770=EDGE_LOOP('',(#9867,#9868,#9869,#9870));
#2771=EDGE_LOOP('',(#9871,#9872,#9873,#9874,#9875,#9876));
#2772=EDGE_LOOP('',(#9877));
#2773=EDGE_LOOP('',(#9878));
#2774=EDGE_LOOP('',(#9879));
#2775=EDGE_LOOP('',(#9880));
#2776=EDGE_LOOP('',(#9881));
#2777=EDGE_LOOP('',(#9882));
#2778=EDGE_LOOP('',(#9883));
#2779=EDGE_LOOP('',(#9884));
#2780=EDGE_LOOP('',(#9885,#9886,#9887,#9888));
#2781=EDGE_LOOP('',(#9889,#9890,#9891,#9892));
#2782=EDGE_LOOP('',(#9893,#9894,#9895,#9896));
#2783=EDGE_LOOP('',(#9897,#9898,#9899,#9900));
#2784=EDGE_LOOP('',(#9901,#9902,#9903,#9904));
#2785=EDGE_LOOP('',(#9905,#9906,#9907,#9908,#9909,#9910));
#2786=EDGE_LOOP('',(#9911));
#2787=EDGE_LOOP('',(#9912));
#2788=EDGE_LOOP('',(#9913));
#2789=EDGE_LOOP('',(#9914));
#2790=EDGE_LOOP('',(#9915,#9916,#9917,#9918));
#2791=EDGE_LOOP('',(#9919));
#2792=EDGE_LOOP('',(#9920));
#2793=EDGE_LOOP('',(#9921));
#2794=EDGE_LOOP('',(#9922));
#2795=EDGE_LOOP('',(#9923,#9924,#9925,#9926));
#2796=EDGE_LOOP('',(#9927,#9928,#9929,#9930));
#2797=EDGE_LOOP('',(#9931,#9932,#9933,#9934));
#2798=EDGE_LOOP('',(#9935,#9936,#9937,#9938));
#2799=EDGE_LOOP('',(#9939,#9940,#9941,#9942));
#2800=EDGE_LOOP('',(#9943,#9944,#9945,#9946));
#2801=EDGE_LOOP('',(#9947,#9948,#9949,#9950,#9951,#9952));
#2802=EDGE_LOOP('',(#9953,#9954,#9955,#9956));
#2803=EDGE_LOOP('',(#9957));
#2804=EDGE_LOOP('',(#9958,#9959,#9960,#9961));
#2805=EDGE_LOOP('',(#9962));
#2806=EDGE_LOOP('',(#9963,#9964,#9965,#9966));
#2807=EDGE_LOOP('',(#9967));
#2808=EDGE_LOOP('',(#9968,#9969,#9970,#9971));
#2809=EDGE_LOOP('',(#9972));
#2810=EDGE_LOOP('',(#9973,#9974,#9975,#9976));
#2811=EDGE_LOOP('',(#9977,#9978));
#2812=EDGE_LOOP('',(#9979,#9980,#9981,#9982));
#2813=EDGE_LOOP('',(#9983,#9984));
#2814=EDGE_LOOP('',(#9985,#9986,#9987,#9988));
#2815=EDGE_LOOP('',(#9989,#9990));
#2816=EDGE_LOOP('',(#9991,#9992,#9993,#9994));
#2817=EDGE_LOOP('',(#9995,#9996));
#2818=EDGE_LOOP('',(#9997,#9998,#9999,#10000));
#2819=EDGE_LOOP('',(#10001));
#2820=EDGE_LOOP('',(#10002,#10003,#10004,#10005,#10006,#10007,#10008,#10009,
#10010));
#2821=EDGE_LOOP('',(#10011));
#2822=EDGE_LOOP('',(#10012));
#2823=EDGE_LOOP('',(#10013));
#2824=EDGE_LOOP('',(#10014));
#2825=EDGE_LOOP('',(#10015,#10016,#10017,#10018));
#2826=EDGE_LOOP('',(#10019,#10020,#10021,#10022));
#2827=EDGE_LOOP('',(#10023,#10024,#10025,#10026));
#2828=EDGE_LOOP('',(#10027,#10028,#10029,#10030,#10031,#10032,#10033,#10034,
#10035,#10036,#10037,#10038,#10039,#10040,#10041,#10042,#10043,#10044,#10045,
#10046));
#2829=EDGE_LOOP('',(#10047,#10048));
#2830=EDGE_LOOP('',(#10049,#10050,#10051,#10052));
#2831=EDGE_LOOP('',(#10053));
#2832=EDGE_LOOP('',(#10054));
#2833=EDGE_LOOP('',(#10055,#10056,#10057,#10058));
#2834=EDGE_LOOP('',(#10059,#10060,#10061,#10062));
#2835=EDGE_LOOP('',(#10063,#10064));
#2836=EDGE_LOOP('',(#10065));
#2837=EDGE_LOOP('',(#10066));
#2838=EDGE_LOOP('',(#10067));
#2839=EDGE_LOOP('',(#10068));
#2840=EDGE_LOOP('',(#10069));
#2841=EDGE_LOOP('',(#10070));
#2842=EDGE_LOOP('',(#10071));
#2843=EDGE_LOOP('',(#10072));
#2844=EDGE_LOOP('',(#10073));
#2845=EDGE_LOOP('',(#10074));
#2846=EDGE_LOOP('',(#10075));
#2847=EDGE_LOOP('',(#10076));
#2848=EDGE_LOOP('',(#10077,#10078,#10079,#10080));
#2849=EDGE_LOOP('',(#10081,#10082,#10083,#10084));
#2850=EDGE_LOOP('',(#10085));
#2851=EDGE_LOOP('',(#10086));
#2852=EDGE_LOOP('',(#10087));
#2853=EDGE_LOOP('',(#10088));
#2854=EDGE_LOOP('',(#10089,#10090,#10091,#10092));
#2855=EDGE_LOOP('',(#10093,#10094,#10095,#10096));
#2856=EDGE_LOOP('',(#10097,#10098,#10099,#10100));
#2857=EDGE_LOOP('',(#10101,#10102,#10103,#10104));
#2858=EDGE_LOOP('',(#10105,#10106,#10107,#10108));
#2859=EDGE_LOOP('',(#10109,#10110,#10111,#10112));
#2860=EDGE_LOOP('',(#10113));
#2861=EDGE_LOOP('',(#10114));
#2862=EDGE_LOOP('',(#10115));
#2863=EDGE_LOOP('',(#10116));
#2864=EDGE_LOOP('',(#10117));
#2865=EDGE_LOOP('',(#10118));
#2866=EDGE_LOOP('',(#10119));
#2867=EDGE_LOOP('',(#10120));
#2868=EDGE_LOOP('',(#10121));
#2869=EDGE_LOOP('',(#10122));
#2870=EDGE_LOOP('',(#10123));
#2871=EDGE_LOOP('',(#10124));
#2872=EDGE_LOOP('',(#10125,#10126));
#2873=EDGE_LOOP('',(#10127,#10128,#10129,#10130,#10131,#10132,#10133,#10134));
#2874=EDGE_LOOP('',(#10135,#10136));
#2875=EDGE_LOOP('',(#10137,#10138,#10139,#10140,#10141,#10142,#10143,#10144));
#2876=EDGE_LOOP('',(#10145,#10146));
#2877=EDGE_LOOP('',(#10147,#10148,#10149,#10150,#10151,#10152,#10153,#10154));
#2878=EDGE_LOOP('',(#10155,#10156));
#2879=EDGE_LOOP('',(#10157,#10158,#10159,#10160,#10161,#10162,#10163,#10164));
#2880=EDGE_LOOP('',(#10165,#10166,#10167,#10168,#10169,#10170,#10171,#10172,
#10173,#10174,#10175,#10176));
#2881=EDGE_LOOP('',(#10177,#10178,#10179,#10180,#10181,#10182,#10183,#10184,
#10185,#10186,#10187,#10188));
#2882=EDGE_LOOP('',(#10189,#10190,#10191,#10192,#10193,#10194,#10195,#10196,
#10197,#10198,#10199,#10200));
#2883=EDGE_LOOP('',(#10201,#10202,#10203,#10204,#10205,#10206,#10207,#10208,
#10209,#10210));
#2884=EDGE_LOOP('',(#10211,#10212,#10213,#10214));
#2885=EDGE_LOOP('',(#10215,#10216,#10217,#10218));
#2886=EDGE_LOOP('',(#10219));
#2887=EDGE_LOOP('',(#10220));
#2888=EDGE_LOOP('',(#10221));
#2889=EDGE_LOOP('',(#10222));
#2890=EDGE_LOOP('',(#10223,#10224,#10225,#10226));
#2891=EDGE_LOOP('',(#10227,#10228,#10229,#10230,#10231,#10232,#10233,#10234,
#10235,#10236));
#2892=EDGE_LOOP('',(#10237,#10238,#10239,#10240));
#2893=EDGE_LOOP('',(#10241,#10242,#10243,#10244));
#2894=EDGE_LOOP('',(#10245,#10246,#10247,#10248));
#2895=EDGE_LOOP('',(#10249,#10250,#10251,#10252));
#2896=EDGE_LOOP('',(#10253,#10254,#10255,#10256));
#2897=EDGE_LOOP('',(#10257,#10258,#10259,#10260,#10261,#10262,#10263,#10264,
#10265,#10266,#10267,#10268));
#2898=EDGE_LOOP('',(#10269,#10270,#10271,#10272));
#2899=EDGE_LOOP('',(#10273,#10274,#10275,#10276));
#2900=EDGE_LOOP('',(#10277,#10278,#10279,#10280));
#2901=EDGE_LOOP('',(#10281,#10282,#10283,#10284));
#2902=EDGE_LOOP('',(#10285,#10286,#10287,#10288));
#2903=EDGE_LOOP('',(#10289,#10290,#10291,#10292));
#2904=EDGE_LOOP('',(#10293,#10294,#10295,#10296));
#2905=EDGE_LOOP('',(#10297,#10298,#10299,#10300));
#2906=EDGE_LOOP('',(#10301,#10302,#10303,#10304,#10305,#10306,#10307,#10308));
#2907=EDGE_LOOP('',(#10309,#10310,#10311,#10312,#10313,#10314,#10315,#10316));
#2908=EDGE_LOOP('',(#10317,#10318,#10319,#10320));
#2909=EDGE_LOOP('',(#10321,#10322,#10323,#10324));
#2910=EDGE_LOOP('',(#10325,#10326,#10327,#10328));
#2911=EDGE_LOOP('',(#10329,#10330,#10331,#10332));
#2912=EDGE_LOOP('',(#10333,#10334,#10335,#10336));
#2913=EDGE_LOOP('',(#10337,#10338,#10339,#10340));
#2914=EDGE_LOOP('',(#10341,#10342,#10343,#10344));
#2915=EDGE_LOOP('',(#10345,#10346,#10347,#10348));
#2916=EDGE_LOOP('',(#10349,#10350,#10351,#10352,#10353,#10354,#10355,#10356));
#2917=EDGE_LOOP('',(#10357,#10358,#10359,#10360,#10361,#10362,#10363,#10364));
#2918=EDGE_LOOP('',(#10365,#10366,#10367,#10368));
#2919=EDGE_LOOP('',(#10369,#10370,#10371,#10372));
#2920=EDGE_LOOP('',(#10373,#10374,#10375,#10376));
#2921=EDGE_LOOP('',(#10377,#10378,#10379,#10380));
#2922=EDGE_LOOP('',(#10381,#10382,#10383,#10384));
#2923=EDGE_LOOP('',(#10385,#10386,#10387,#10388));
#2924=EDGE_LOOP('',(#10389,#10390,#10391,#10392,#10393,#10394));
#2925=EDGE_LOOP('',(#10395));
#2926=EDGE_LOOP('',(#10396,#10397,#10398,#10399,#10400,#10401));
#2927=EDGE_LOOP('',(#10402,#10403,#10404,#10405));
#2928=EDGE_LOOP('',(#10406,#10407,#10408,#10409));
#2929=EDGE_LOOP('',(#10410,#10411,#10412,#10413));
#2930=EDGE_LOOP('',(#10414));
#2931=EDGE_LOOP('',(#10415,#10416,#10417,#10418));
#2932=EDGE_LOOP('',(#10419,#10420,#10421,#10422));
#2933=EDGE_LOOP('',(#10423,#10424,#10425,#10426));
#2934=EDGE_LOOP('',(#10427,#10428,#10429,#10430));
#2935=EDGE_LOOP('',(#10431,#10432,#10433,#10434));
#2936=EDGE_LOOP('',(#10435,#10436,#10437,#10438));
#2937=EDGE_LOOP('',(#10439,#10440,#10441,#10442,#10443,#10444));
#2938=EDGE_LOOP('',(#10445,#10446,#10447,#10448,#10449,#10450));
#2939=EDGE_LOOP('',(#10451));
#2940=EDGE_LOOP('',(#10452));
#2941=EDGE_LOOP('',(#10453,#10454,#10455,#10456));
#2942=EDGE_LOOP('',(#10457,#10458,#10459,#10460));
#2943=EDGE_LOOP('',(#10461,#10462,#10463,#10464));
#2944=EDGE_LOOP('',(#10465));
#2945=EDGE_LOOP('',(#10466));
#2946=EDGE_LOOP('',(#10467,#10468,#10469,#10470));
#2947=EDGE_LOOP('',(#10471,#10472,#10473,#10474));
#2948=EDGE_LOOP('',(#10475,#10476,#10477,#10478,#10479,#10480));
#2949=EDGE_LOOP('',(#10481,#10482,#10483,#10484,#10485));
#2950=EDGE_LOOP('',(#10486,#10487,#10488,#10489));
#2951=EDGE_LOOP('',(#10490,#10491,#10492,#10493));
#2952=EDGE_LOOP('',(#10494));
#2953=EDGE_LOOP('',(#10495));
#2954=EDGE_LOOP('',(#10496,#10497,#10498,#10499,#10500));
#2955=EDGE_LOOP('',(#10501));
#2956=EDGE_LOOP('',(#10502));
#2957=EDGE_LOOP('',(#10503,#10504,#10505,#10506));
#2958=EDGE_LOOP('',(#10507,#10508,#10509,#10510,#10511,#10512));
#2959=EDGE_LOOP('',(#10513,#10514,#10515,#10516,#10517));
#2960=EDGE_LOOP('',(#10518));
#2961=EDGE_LOOP('',(#10519));
#2962=EDGE_LOOP('',(#10520,#10521,#10522,#10523));
#2963=EDGE_LOOP('',(#10524,#10525,#10526,#10527));
#2964=EDGE_LOOP('',(#10528,#10529,#10530,#10531));
#2965=EDGE_LOOP('',(#10532));
#2966=EDGE_LOOP('',(#10533));
#2967=EDGE_LOOP('',(#10534,#10535,#10536,#10537,#10538));
#2968=EDGE_LOOP('',(#10539,#10540));
#2969=EDGE_LOOP('',(#10541,#10542));
#2970=EDGE_LOOP('',(#10543,#10544));
#2971=EDGE_LOOP('',(#10545,#10546));
#2972=EDGE_LOOP('',(#10547,#10548));
#2973=EDGE_LOOP('',(#10549,#10550));
#2974=EDGE_LOOP('',(#10551,#10552));
#2975=EDGE_LOOP('',(#10553,#10554));
#2976=EDGE_LOOP('',(#10555,#10556,#10557,#10558));
#2977=EDGE_LOOP('',(#10559,#10560,#10561,#10562,#10563,#10564,#10565,#10566,
#10567,#10568,#10569,#10570,#10571,#10572,#10573,#10574,#10575,#10576,#10577,
#10578));
#2978=EDGE_LOOP('',(#10579,#10580,#10581,#10582));
#2979=EDGE_LOOP('',(#10583,#10584,#10585,#10586));
#2980=EDGE_LOOP('',(#10587,#10588,#10589,#10590));
#2981=EDGE_LOOP('',(#10591,#10592,#10593,#10594));
#2982=EDGE_LOOP('',(#10595,#10596,#10597,#10598));
#2983=EDGE_LOOP('',(#10599,#10600,#10601,#10602,#10603,#10604));
#2984=EDGE_LOOP('',(#10605,#10606,#10607,#10608));
#2985=EDGE_LOOP('',(#10609,#10610,#10611,#10612));
#2986=EDGE_LOOP('',(#10613,#10614,#10615,#10616));
#2987=EDGE_LOOP('',(#10617,#10618,#10619,#10620));
#2988=EDGE_LOOP('',(#10621,#10622,#10623,#10624));
#2989=EDGE_LOOP('',(#10625,#10626,#10627,#10628));
#2990=EDGE_LOOP('',(#10629,#10630,#10631,#10632,#10633,#10634,#10635,#10636,
#10637,#10638,#10639,#10640,#10641,#10642,#10643,#10644,#10645,#10646,#10647,
#10648));
#2991=EDGE_LOOP('',(#10649,#10650,#10651,#10652));
#2992=EDGE_LOOP('',(#10653,#10654,#10655,#10656));
#2993=EDGE_LOOP('',(#10657));
#2994=EDGE_LOOP('',(#10658));
#2995=EDGE_LOOP('',(#10659,#10660,#10661,#10662));
#2996=EDGE_LOOP('',(#10663));
#2997=EDGE_LOOP('',(#10664));
#2998=EDGE_LOOP('',(#10665,#10666,#10667,#10668));
#2999=EDGE_LOOP('',(#10669));
#3000=EDGE_LOOP('',(#10670));
#3001=EDGE_LOOP('',(#10671,#10672,#10673,#10674));
#3002=EDGE_LOOP('',(#10675));
#3003=EDGE_LOOP('',(#10676));
#3004=EDGE_LOOP('',(#10677,#10678,#10679,#10680));
#3005=EDGE_LOOP('',(#10681));
#3006=EDGE_LOOP('',(#10682));
#3007=EDGE_LOOP('',(#10683,#10684,#10685,#10686));
#3008=EDGE_LOOP('',(#10687,#10688,#10689,#10690));
#3009=EDGE_LOOP('',(#10691));
#3010=EDGE_LOOP('',(#10692,#10693,#10694,#10695));
#3011=EDGE_LOOP('',(#10696,#10697,#10698,#10699));
#3012=EDGE_LOOP('',(#10700,#10701,#10702,#10703));
#3013=EDGE_LOOP('',(#10704,#10705,#10706,#10707));
#3014=EDGE_LOOP('',(#10708,#10709,#10710,#10711));
#3015=EDGE_LOOP('',(#10712));
#3016=EDGE_LOOP('',(#10713));
#3017=EDGE_LOOP('',(#10714));
#3018=EDGE_LOOP('',(#10715));
#3019=EDGE_LOOP('',(#10716,#10717,#10718,#10719));
#3020=EDGE_LOOP('',(#10720,#10721,#10722,#10723));
#3021=EDGE_LOOP('',(#10724,#10725,#10726,#10727));
#3022=EDGE_LOOP('',(#10728,#10729,#10730,#10731));
#3023=EDGE_LOOP('',(#10732));
#3024=EDGE_LOOP('',(#10733));
#3025=EDGE_LOOP('',(#10734));
#3026=EDGE_LOOP('',(#10735,#10736,#10737,#10738));
#3027=EDGE_LOOP('',(#10739,#10740,#10741,#10742));
#3028=EDGE_LOOP('',(#10743));
#3029=EDGE_LOOP('',(#10744));
#3030=EDGE_LOOP('',(#10745));
#3031=EDGE_LOOP('',(#10746));
#3032=EDGE_LOOP('',(#10747,#10748,#10749,#10750));
#3033=EDGE_LOOP('',(#10751,#10752,#10753,#10754));
#3034=EDGE_LOOP('',(#10755));
#3035=EDGE_LOOP('',(#10756));
#3036=EDGE_LOOP('',(#10757));
#3037=EDGE_LOOP('',(#10758));
#3038=EDGE_LOOP('',(#10759,#10760,#10761,#10762));
#3039=EDGE_LOOP('',(#10763,#10764,#10765,#10766));
#3040=EDGE_LOOP('',(#10767));
#3041=EDGE_LOOP('',(#10768));
#3042=EDGE_LOOP('',(#10769));
#3043=EDGE_LOOP('',(#10770));
#3044=EDGE_LOOP('',(#10771,#10772));
#3045=EDGE_LOOP('',(#10773,#10774,#10775,#10776,#10777));
#3046=EDGE_LOOP('',(#10778,#10779,#10780,#10781,#10782,#10783,#10784,#10785,
#10786,#10787,#10788,#10789));
#3047=EDGE_LOOP('',(#10790,#10791));
#3048=EDGE_LOOP('',(#10792,#10793,#10794,#10795));
#3049=EDGE_LOOP('',(#10796,#10797,#10798,#10799,#10800));
#3050=EDGE_LOOP('',(#10801,#10802,#10803,#10804));
#3051=EDGE_LOOP('',(#10805,#10806));
#3052=EDGE_LOOP('',(#10807,#10808));
#3053=EDGE_LOOP('',(#10809));
#3054=EDGE_LOOP('',(#10810));
#3055=EDGE_LOOP('',(#10811));
#3056=EDGE_LOOP('',(#10812));
#3057=EDGE_LOOP('',(#10813,#10814,#10815,#10816));
#3058=EDGE_LOOP('',(#10817,#10818,#10819,#10820));
#3059=EDGE_LOOP('',(#10821,#10822,#10823,#10824));
#3060=EDGE_LOOP('',(#10825,#10826,#10827,#10828));
#3061=EDGE_LOOP('',(#10829,#10830,#10831,#10832));
#3062=EDGE_LOOP('',(#10833,#10834,#10835,#10836));
#3063=EDGE_LOOP('',(#10837,#10838,#10839,#10840));
#3064=EDGE_LOOP('',(#10841,#10842,#10843,#10844));
#3065=EDGE_LOOP('',(#10845));
#3066=EDGE_LOOP('',(#10846));
#3067=EDGE_LOOP('',(#10847));
#3068=EDGE_LOOP('',(#10848));
#3069=EDGE_LOOP('',(#10849,#10850,#10851,#10852));
#3070=EDGE_LOOP('',(#10853,#10854,#10855,#10856));
#3071=EDGE_LOOP('',(#10857,#10858,#10859,#10860));
#3072=EDGE_LOOP('',(#10861,#10862,#10863,#10864,#10865,#10866,#10867,#10868,
#10869,#10870,#10871,#10872,#10873,#10874,#10875,#10876,#10877,#10878,#10879,
#10880,#10881,#10882,#10883,#10884,#10885,#10886,#10887,#10888,#10889,#10890,
#10891,#10892,#10893,#10894,#10895,#10896,#10897,#10898,#10899,#10900,#10901,
#10902,#10903,#10904,#10905,#10906,#10907,#10908,#10909,#10910,#10911,#10912,
#10913,#10914,#10915,#10916,#10917,#10918,#10919,#10920,#10921,#10922,#10923,
#10924,#10925,#10926,#10927,#10928,#10929,#10930,#10931,#10932,#10933,#10934,
#10935,#10936,#10937,#10938,#10939,#10940));
#3073=EDGE_LOOP('',(#10941,#10942,#10943,#10944));
#3074=EDGE_LOOP('',(#10945,#10946,#10947,#10948));
#3075=EDGE_LOOP('',(#10949,#10950,#10951,#10952));
#3076=EDGE_LOOP('',(#10953));
#3077=EDGE_LOOP('',(#10954,#10955,#10956,#10957));
#3078=EDGE_LOOP('',(#10958,#10959,#10960,#10961));
#3079=EDGE_LOOP('',(#10962,#10963,#10964,#10965));
#3080=EDGE_LOOP('',(#10966,#10967,#10968,#10969));
#3081=EDGE_LOOP('',(#10970,#10971,#10972,#10973));
#3082=EDGE_LOOP('',(#10974,#10975,#10976,#10977));
#3083=EDGE_LOOP('',(#10978,#10979,#10980,#10981));
#3084=EDGE_LOOP('',(#10982,#10983,#10984,#10985));
#3085=EDGE_LOOP('',(#10986,#10987,#10988,#10989));
#3086=EDGE_LOOP('',(#10990,#10991,#10992,#10993));
#3087=EDGE_LOOP('',(#10994,#10995,#10996,#10997));
#3088=EDGE_LOOP('',(#10998,#10999,#11000,#11001));
#3089=EDGE_LOOP('',(#11002,#11003,#11004,#11005));
#3090=EDGE_LOOP('',(#11006,#11007,#11008,#11009));
#3091=EDGE_LOOP('',(#11010,#11011,#11012,#11013));
#3092=EDGE_LOOP('',(#11014,#11015,#11016,#11017));
#3093=EDGE_LOOP('',(#11018,#11019,#11020,#11021));
#3094=EDGE_LOOP('',(#11022,#11023,#11024,#11025));
#3095=EDGE_LOOP('',(#11026,#11027,#11028,#11029));
#3096=EDGE_LOOP('',(#11030,#11031,#11032,#11033));
#3097=EDGE_LOOP('',(#11034,#11035,#11036,#11037));
#3098=EDGE_LOOP('',(#11038,#11039,#11040,#11041));
#3099=EDGE_LOOP('',(#11042,#11043,#11044,#11045));
#3100=EDGE_LOOP('',(#11046,#11047,#11048,#11049));
#3101=EDGE_LOOP('',(#11050,#11051,#11052,#11053));
#3102=EDGE_LOOP('',(#11054,#11055,#11056,#11057));
#3103=EDGE_LOOP('',(#11058,#11059,#11060,#11061));
#3104=EDGE_LOOP('',(#11062,#11063,#11064,#11065));
#3105=EDGE_LOOP('',(#11066,#11067,#11068,#11069));
#3106=EDGE_LOOP('',(#11070,#11071,#11072,#11073));
#3107=EDGE_LOOP('',(#11074,#11075,#11076,#11077));
#3108=EDGE_LOOP('',(#11078,#11079,#11080,#11081));
#3109=EDGE_LOOP('',(#11082,#11083,#11084,#11085));
#3110=EDGE_LOOP('',(#11086,#11087,#11088,#11089));
#3111=EDGE_LOOP('',(#11090,#11091,#11092,#11093));
#3112=EDGE_LOOP('',(#11094,#11095,#11096,#11097));
#3113=EDGE_LOOP('',(#11098,#11099,#11100,#11101));
#3114=EDGE_LOOP('',(#11102,#11103,#11104,#11105));
#3115=EDGE_LOOP('',(#11106,#11107,#11108,#11109));
#3116=EDGE_LOOP('',(#11110,#11111,#11112,#11113));
#3117=EDGE_LOOP('',(#11114,#11115,#11116,#11117));
#3118=EDGE_LOOP('',(#11118,#11119,#11120,#11121));
#3119=EDGE_LOOP('',(#11122,#11123,#11124,#11125));
#3120=EDGE_LOOP('',(#11126,#11127,#11128,#11129));
#3121=EDGE_LOOP('',(#11130,#11131,#11132,#11133));
#3122=EDGE_LOOP('',(#11134,#11135,#11136,#11137));
#3123=EDGE_LOOP('',(#11138,#11139,#11140,#11141));
#3124=EDGE_LOOP('',(#11142,#11143,#11144,#11145));
#3125=EDGE_LOOP('',(#11146,#11147,#11148,#11149));
#3126=EDGE_LOOP('',(#11150,#11151,#11152,#11153));
#3127=EDGE_LOOP('',(#11154,#11155,#11156,#11157));
#3128=EDGE_LOOP('',(#11158,#11159,#11160,#11161));
#3129=EDGE_LOOP('',(#11162,#11163,#11164,#11165));
#3130=EDGE_LOOP('',(#11166,#11167,#11168,#11169));
#3131=EDGE_LOOP('',(#11170,#11171,#11172,#11173));
#3132=EDGE_LOOP('',(#11174,#11175,#11176,#11177));
#3133=EDGE_LOOP('',(#11178,#11179,#11180,#11181));
#3134=EDGE_LOOP('',(#11182,#11183,#11184,#11185));
#3135=EDGE_LOOP('',(#11186,#11187,#11188,#11189));
#3136=EDGE_LOOP('',(#11190,#11191,#11192,#11193));
#3137=EDGE_LOOP('',(#11194,#11195,#11196,#11197));
#3138=EDGE_LOOP('',(#11198,#11199,#11200,#11201));
#3139=EDGE_LOOP('',(#11202,#11203,#11204,#11205));
#3140=EDGE_LOOP('',(#11206,#11207,#11208,#11209));
#3141=EDGE_LOOP('',(#11210,#11211,#11212,#11213));
#3142=EDGE_LOOP('',(#11214,#11215,#11216,#11217));
#3143=EDGE_LOOP('',(#11218,#11219,#11220,#11221));
#3144=EDGE_LOOP('',(#11222,#11223,#11224,#11225));
#3145=EDGE_LOOP('',(#11226,#11227,#11228,#11229));
#3146=EDGE_LOOP('',(#11230,#11231,#11232,#11233));
#3147=EDGE_LOOP('',(#11234,#11235,#11236,#11237));
#3148=EDGE_LOOP('',(#11238,#11239,#11240,#11241));
#3149=EDGE_LOOP('',(#11242,#11243,#11244,#11245));
#3150=EDGE_LOOP('',(#11246,#11247,#11248,#11249));
#3151=EDGE_LOOP('',(#11250,#11251,#11252,#11253));
#3152=EDGE_LOOP('',(#11254,#11255,#11256,#11257));
#3153=EDGE_LOOP('',(#11258,#11259,#11260,#11261));
#3154=EDGE_LOOP('',(#11262,#11263,#11264,#11265));
#3155=EDGE_LOOP('',(#11266,#11267,#11268,#11269));
#3156=EDGE_LOOP('',(#11270,#11271,#11272,#11273));
#3157=EDGE_LOOP('',(#11274,#11275,#11276,#11277,#11278,#11279,#11280,#11281,
#11282,#11283,#11284,#11285,#11286,#11287,#11288,#11289,#11290,#11291,#11292,
#11293,#11294,#11295,#11296,#11297,#11298,#11299,#11300,#11301,#11302,#11303,
#11304,#11305,#11306,#11307,#11308,#11309,#11310,#11311,#11312,#11313,#11314,
#11315,#11316,#11317,#11318,#11319,#11320,#11321,#11322,#11323,#11324,#11325,
#11326,#11327,#11328,#11329,#11330,#11331,#11332,#11333,#11334,#11335,#11336,
#11337,#11338,#11339,#11340,#11341,#11342,#11343,#11344,#11345,#11346,#11347,
#11348,#11349,#11350,#11351,#11352,#11353));
#3158=EDGE_LOOP('',(#11354));
#3159=EDGE_LOOP('',(#11355,#11356,#11357,#11358));
#3160=EDGE_LOOP('',(#11359,#11360,#11361,#11362));
#3161=EDGE_LOOP('',(#11363));
#3162=EDGE_LOOP('',(#11364,#11365,#11366,#11367));
#3163=EDGE_LOOP('',(#11368,#11369,#11370,#11371));
#3164=EDGE_LOOP('',(#11372,#11373,#11374,#11375));
#3165=EDGE_LOOP('',(#11376,#11377,#11378,#11379));
#3166=EDGE_LOOP('',(#11380,#11381,#11382,#11383));
#3167=EDGE_LOOP('',(#11384));
#3168=EDGE_LOOP('',(#11385));
#3169=EDGE_LOOP('',(#11386));
#3170=EDGE_LOOP('',(#11387));
#3171=EDGE_LOOP('',(#11388,#11389,#11390,#11391));
#3172=EDGE_LOOP('',(#11392,#11393,#11394,#11395));
#3173=EDGE_LOOP('',(#11396,#11397,#11398,#11399));
#3174=EDGE_LOOP('',(#11400,#11401,#11402,#11403));
#3175=EDGE_LOOP('',(#11404));
#3176=EDGE_LOOP('',(#11405));
#3177=EDGE_LOOP('',(#11406));
#3178=EDGE_LOOP('',(#11407,#11408,#11409,#11410));
#3179=EDGE_LOOP('',(#11411,#11412,#11413,#11414));
#3180=EDGE_LOOP('',(#11415));
#3181=EDGE_LOOP('',(#11416));
#3182=EDGE_LOOP('',(#11417));
#3183=EDGE_LOOP('',(#11418));
#3184=EDGE_LOOP('',(#11419,#11420,#11421,#11422));
#3185=EDGE_LOOP('',(#11423,#11424,#11425,#11426));
#3186=EDGE_LOOP('',(#11427));
#3187=EDGE_LOOP('',(#11428));
#3188=EDGE_LOOP('',(#11429));
#3189=EDGE_LOOP('',(#11430));
#3190=EDGE_LOOP('',(#11431,#11432,#11433,#11434,#11435,#11436));
#3191=EDGE_LOOP('',(#11437,#11438,#11439,#11440));
#3192=EDGE_LOOP('',(#11441,#11442));
#3193=EDGE_LOOP('',(#11443,#11444,#11445,#11446));
#3194=EDGE_LOOP('',(#11447,#11448));
#3195=EDGE_LOOP('',(#11449));
#3196=EDGE_LOOP('',(#11450));
#3197=EDGE_LOOP('',(#11451));
#3198=EDGE_LOOP('',(#11452));
#3199=EDGE_LOOP('',(#11453,#11454,#11455,#11456));
#3200=EDGE_LOOP('',(#11457,#11458,#11459,#11460));
#3201=EDGE_LOOP('',(#11461,#11462,#11463,#11464));
#3202=EDGE_LOOP('',(#11465,#11466,#11467,#11468));
#3203=EDGE_LOOP('',(#11469,#11470,#11471,#11472));
#3204=EDGE_LOOP('',(#11473,#11474,#11475,#11476));
#3205=EDGE_LOOP('',(#11477,#11478,#11479,#11480));
#3206=EDGE_LOOP('',(#11481,#11482,#11483,#11484));
#3207=EDGE_LOOP('',(#11485));
#3208=EDGE_LOOP('',(#11486));
#3209=EDGE_LOOP('',(#11487));
#3210=EDGE_LOOP('',(#11488));
#3211=EDGE_LOOP('',(#11489));
#3212=EDGE_LOOP('',(#11490,#11491,#11492,#11493));
#3213=EDGE_LOOP('',(#11494,#11495,#11496,#11497));
#3214=EDGE_LOOP('',(#11498,#11499,#11500,#11501));
#3215=EDGE_LOOP('',(#11502,#11503,#11504,#11505));
#3216=EDGE_LOOP('',(#11506,#11507,#11508,#11509));
#3217=EDGE_LOOP('',(#11510,#11511,#11512,#11513));
#3218=EDGE_LOOP('',(#11514,#11515,#11516,#11517,#11518,#11519));
#3219=EDGE_LOOP('',(#11520));
#3220=EDGE_LOOP('',(#11521,#11522,#11523,#11524,#11525,#11526));
#3221=EDGE_LOOP('',(#11527,#11528,#11529,#11530));
#3222=EDGE_LOOP('',(#11531,#11532,#11533,#11534));
#3223=EDGE_LOOP('',(#11535,#11536,#11537,#11538));
#3224=EDGE_LOOP('',(#11539,#11540,#11541,#11542));
#3225=EDGE_LOOP('',(#11543,#11544,#11545,#11546));
#3226=EDGE_LOOP('',(#11547,#11548,#11549,#11550,#11551,#11552,#11553,#11554,
#11555,#11556,#11557,#11558,#11559,#11560,#11561,#11562,#11563,#11564,#11565,
#11566,#11567,#11568,#11569,#11570,#11571,#11572,#11573,#11574,#11575,#11576,
#11577,#11578,#11579,#11580,#11581,#11582,#11583,#11584,#11585,#11586,#11587,
#11588,#11589,#11590,#11591,#11592,#11593,#11594,#11595,#11596,#11597,#11598,
#11599,#11600,#11601,#11602,#11603,#11604,#11605,#11606,#11607,#11608,#11609,
#11610,#11611,#11612,#11613,#11614,#11615,#11616,#11617,#11618,#11619,#11620,
#11621,#11622,#11623,#11624,#11625,#11626,#11627,#11628,#11629,#11630,#11631,
#11632,#11633,#11634,#11635,#11636,#11637,#11638,#11639,#11640,#11641,#11642,
#11643,#11644,#11645,#11646,#11647,#11648,#11649,#11650,#11651,#11652,#11653,
#11654,#11655,#11656,#11657,#11658,#11659,#11660,#11661,#11662,#11663,#11664,
#11665,#11666,#11667,#11668,#11669,#11670,#11671,#11672,#11673,#11674,#11675,
#11676,#11677,#11678,#11679,#11680,#11681,#11682,#11683,#11684,#11685,#11686,
#11687,#11688,#11689,#11690,#11691,#11692,#11693,#11694,#11695,#11696,#11697,
#11698,#11699,#11700,#11701,#11702,#11703,#11704,#11705,#11706));
#3227=EDGE_LOOP('',(#11707,#11708,#11709,#11710));
#3228=EDGE_LOOP('',(#11711,#11712,#11713,#11714));
#3229=EDGE_LOOP('',(#11715,#11716,#11717,#11718));
#3230=EDGE_LOOP('',(#11719));
#3231=EDGE_LOOP('',(#11720,#11721,#11722,#11723));
#3232=EDGE_LOOP('',(#11724,#11725,#11726,#11727));
#3233=EDGE_LOOP('',(#11728,#11729,#11730,#11731));
#3234=EDGE_LOOP('',(#11732,#11733,#11734,#11735));
#3235=EDGE_LOOP('',(#11736,#11737,#11738,#11739));
#3236=EDGE_LOOP('',(#11740,#11741,#11742,#11743));
#3237=EDGE_LOOP('',(#11744,#11745,#11746,#11747));
#3238=EDGE_LOOP('',(#11748,#11749,#11750,#11751));
#3239=EDGE_LOOP('',(#11752,#11753,#11754,#11755));
#3240=EDGE_LOOP('',(#11756,#11757,#11758,#11759));
#3241=EDGE_LOOP('',(#11760,#11761,#11762,#11763));
#3242=EDGE_LOOP('',(#11764,#11765,#11766,#11767));
#3243=EDGE_LOOP('',(#11768,#11769,#11770,#11771));
#3244=EDGE_LOOP('',(#11772,#11773,#11774,#11775));
#3245=EDGE_LOOP('',(#11776,#11777,#11778,#11779));
#3246=EDGE_LOOP('',(#11780,#11781,#11782,#11783));
#3247=EDGE_LOOP('',(#11784,#11785,#11786,#11787));
#3248=EDGE_LOOP('',(#11788,#11789,#11790,#11791));
#3249=EDGE_LOOP('',(#11792,#11793,#11794,#11795));
#3250=EDGE_LOOP('',(#11796,#11797,#11798,#11799));
#3251=EDGE_LOOP('',(#11800,#11801,#11802,#11803));
#3252=EDGE_LOOP('',(#11804,#11805,#11806,#11807));
#3253=EDGE_LOOP('',(#11808,#11809,#11810,#11811));
#3254=EDGE_LOOP('',(#11812,#11813,#11814,#11815));
#3255=EDGE_LOOP('',(#11816,#11817,#11818,#11819));
#3256=EDGE_LOOP('',(#11820,#11821,#11822,#11823));
#3257=EDGE_LOOP('',(#11824,#11825,#11826,#11827));
#3258=EDGE_LOOP('',(#11828,#11829,#11830,#11831));
#3259=EDGE_LOOP('',(#11832,#11833,#11834,#11835));
#3260=EDGE_LOOP('',(#11836,#11837,#11838,#11839));
#3261=EDGE_LOOP('',(#11840,#11841,#11842,#11843));
#3262=EDGE_LOOP('',(#11844,#11845,#11846,#11847));
#3263=EDGE_LOOP('',(#11848,#11849,#11850,#11851));
#3264=EDGE_LOOP('',(#11852,#11853,#11854,#11855));
#3265=EDGE_LOOP('',(#11856,#11857,#11858,#11859));
#3266=EDGE_LOOP('',(#11860,#11861,#11862,#11863));
#3267=EDGE_LOOP('',(#11864,#11865,#11866,#11867));
#3268=EDGE_LOOP('',(#11868,#11869,#11870,#11871));
#3269=EDGE_LOOP('',(#11872,#11873,#11874,#11875));
#3270=EDGE_LOOP('',(#11876,#11877,#11878,#11879));
#3271=EDGE_LOOP('',(#11880,#11881,#11882,#11883));
#3272=EDGE_LOOP('',(#11884,#11885,#11886,#11887));
#3273=EDGE_LOOP('',(#11888,#11889,#11890,#11891));
#3274=EDGE_LOOP('',(#11892,#11893,#11894,#11895));
#3275=EDGE_LOOP('',(#11896,#11897,#11898,#11899));
#3276=EDGE_LOOP('',(#11900,#11901,#11902,#11903));
#3277=EDGE_LOOP('',(#11904,#11905,#11906,#11907));
#3278=EDGE_LOOP('',(#11908,#11909,#11910,#11911));
#3279=EDGE_LOOP('',(#11912,#11913,#11914,#11915));
#3280=EDGE_LOOP('',(#11916,#11917,#11918,#11919));
#3281=EDGE_LOOP('',(#11920,#11921,#11922,#11923));
#3282=EDGE_LOOP('',(#11924,#11925,#11926,#11927));
#3283=EDGE_LOOP('',(#11928,#11929,#11930,#11931));
#3284=EDGE_LOOP('',(#11932,#11933,#11934,#11935));
#3285=EDGE_LOOP('',(#11936,#11937,#11938,#11939));
#3286=EDGE_LOOP('',(#11940,#11941,#11942,#11943));
#3287=EDGE_LOOP('',(#11944,#11945,#11946,#11947));
#3288=EDGE_LOOP('',(#11948,#11949,#11950,#11951));
#3289=EDGE_LOOP('',(#11952,#11953,#11954,#11955));
#3290=EDGE_LOOP('',(#11956,#11957,#11958,#11959));
#3291=EDGE_LOOP('',(#11960,#11961,#11962,#11963));
#3292=EDGE_LOOP('',(#11964,#11965,#11966,#11967));
#3293=EDGE_LOOP('',(#11968,#11969,#11970,#11971));
#3294=EDGE_LOOP('',(#11972,#11973,#11974,#11975));
#3295=EDGE_LOOP('',(#11976,#11977,#11978,#11979));
#3296=EDGE_LOOP('',(#11980,#11981,#11982,#11983));
#3297=EDGE_LOOP('',(#11984,#11985,#11986,#11987));
#3298=EDGE_LOOP('',(#11988,#11989,#11990,#11991));
#3299=EDGE_LOOP('',(#11992,#11993,#11994,#11995));
#3300=EDGE_LOOP('',(#11996,#11997,#11998,#11999));
#3301=EDGE_LOOP('',(#12000,#12001,#12002,#12003));
#3302=EDGE_LOOP('',(#12004,#12005,#12006,#12007));
#3303=EDGE_LOOP('',(#12008,#12009,#12010,#12011));
#3304=EDGE_LOOP('',(#12012,#12013,#12014,#12015));
#3305=EDGE_LOOP('',(#12016,#12017,#12018,#12019));
#3306=EDGE_LOOP('',(#12020,#12021,#12022,#12023));
#3307=EDGE_LOOP('',(#12024,#12025,#12026,#12027));
#3308=EDGE_LOOP('',(#12028,#12029,#12030,#12031));
#3309=EDGE_LOOP('',(#12032,#12033,#12034,#12035));
#3310=EDGE_LOOP('',(#12036,#12037,#12038,#12039));
#3311=EDGE_LOOP('',(#12040,#12041,#12042,#12043));
#3312=EDGE_LOOP('',(#12044,#12045,#12046,#12047));
#3313=EDGE_LOOP('',(#12048,#12049,#12050,#12051));
#3314=EDGE_LOOP('',(#12052,#12053,#12054,#12055));
#3315=EDGE_LOOP('',(#12056,#12057,#12058,#12059));
#3316=EDGE_LOOP('',(#12060,#12061,#12062,#12063));
#3317=EDGE_LOOP('',(#12064,#12065,#12066,#12067));
#3318=EDGE_LOOP('',(#12068,#12069,#12070,#12071));
#3319=EDGE_LOOP('',(#12072,#12073,#12074,#12075));
#3320=EDGE_LOOP('',(#12076,#12077,#12078,#12079));
#3321=EDGE_LOOP('',(#12080,#12081,#12082,#12083));
#3322=EDGE_LOOP('',(#12084,#12085,#12086,#12087));
#3323=EDGE_LOOP('',(#12088,#12089,#12090,#12091));
#3324=EDGE_LOOP('',(#12092,#12093,#12094,#12095));
#3325=EDGE_LOOP('',(#12096,#12097,#12098,#12099));
#3326=EDGE_LOOP('',(#12100,#12101,#12102,#12103));
#3327=EDGE_LOOP('',(#12104,#12105,#12106,#12107));
#3328=EDGE_LOOP('',(#12108,#12109,#12110,#12111));
#3329=EDGE_LOOP('',(#12112,#12113,#12114,#12115));
#3330=EDGE_LOOP('',(#12116,#12117,#12118,#12119));
#3331=EDGE_LOOP('',(#12120,#12121,#12122,#12123));
#3332=EDGE_LOOP('',(#12124,#12125,#12126,#12127));
#3333=EDGE_LOOP('',(#12128,#12129,#12130,#12131));
#3334=EDGE_LOOP('',(#12132,#12133,#12134,#12135));
#3335=EDGE_LOOP('',(#12136,#12137,#12138,#12139));
#3336=EDGE_LOOP('',(#12140,#12141,#12142,#12143));
#3337=EDGE_LOOP('',(#12144,#12145,#12146,#12147));
#3338=EDGE_LOOP('',(#12148,#12149,#12150,#12151));
#3339=EDGE_LOOP('',(#12152,#12153,#12154,#12155));
#3340=EDGE_LOOP('',(#12156,#12157,#12158,#12159));
#3341=EDGE_LOOP('',(#12160,#12161,#12162,#12163));
#3342=EDGE_LOOP('',(#12164,#12165,#12166,#12167));
#3343=EDGE_LOOP('',(#12168,#12169,#12170,#12171));
#3344=EDGE_LOOP('',(#12172,#12173,#12174,#12175));
#3345=EDGE_LOOP('',(#12176,#12177,#12178,#12179));
#3346=EDGE_LOOP('',(#12180,#12181,#12182,#12183));
#3347=EDGE_LOOP('',(#12184,#12185,#12186,#12187));
#3348=EDGE_LOOP('',(#12188,#12189,#12190,#12191));
#3349=EDGE_LOOP('',(#12192,#12193,#12194,#12195));
#3350=EDGE_LOOP('',(#12196,#12197,#12198,#12199));
#3351=EDGE_LOOP('',(#12200,#12201,#12202,#12203));
#3352=EDGE_LOOP('',(#12204,#12205,#12206,#12207));
#3353=EDGE_LOOP('',(#12208,#12209,#12210,#12211));
#3354=EDGE_LOOP('',(#12212,#12213,#12214,#12215));
#3355=EDGE_LOOP('',(#12216,#12217,#12218,#12219));
#3356=EDGE_LOOP('',(#12220,#12221,#12222,#12223));
#3357=EDGE_LOOP('',(#12224,#12225,#12226,#12227));
#3358=EDGE_LOOP('',(#12228,#12229,#12230,#12231));
#3359=EDGE_LOOP('',(#12232,#12233,#12234,#12235));
#3360=EDGE_LOOP('',(#12236,#12237,#12238,#12239));
#3361=EDGE_LOOP('',(#12240,#12241,#12242,#12243));
#3362=EDGE_LOOP('',(#12244,#12245,#12246,#12247));
#3363=EDGE_LOOP('',(#12248,#12249,#12250,#12251));
#3364=EDGE_LOOP('',(#12252,#12253,#12254,#12255));
#3365=EDGE_LOOP('',(#12256,#12257,#12258,#12259));
#3366=EDGE_LOOP('',(#12260,#12261,#12262,#12263));
#3367=EDGE_LOOP('',(#12264,#12265,#12266,#12267));
#3368=EDGE_LOOP('',(#12268,#12269,#12270,#12271));
#3369=EDGE_LOOP('',(#12272,#12273,#12274,#12275));
#3370=EDGE_LOOP('',(#12276,#12277,#12278,#12279));
#3371=EDGE_LOOP('',(#12280,#12281,#12282,#12283));
#3372=EDGE_LOOP('',(#12284,#12285,#12286,#12287));
#3373=EDGE_LOOP('',(#12288,#12289,#12290,#12291));
#3374=EDGE_LOOP('',(#12292,#12293,#12294,#12295));
#3375=EDGE_LOOP('',(#12296,#12297,#12298,#12299));
#3376=EDGE_LOOP('',(#12300,#12301,#12302,#12303));
#3377=EDGE_LOOP('',(#12304,#12305,#12306,#12307));
#3378=EDGE_LOOP('',(#12308,#12309,#12310,#12311));
#3379=EDGE_LOOP('',(#12312,#12313,#12314,#12315));
#3380=EDGE_LOOP('',(#12316,#12317,#12318,#12319));
#3381=EDGE_LOOP('',(#12320,#12321,#12322,#12323));
#3382=EDGE_LOOP('',(#12324,#12325,#12326,#12327));
#3383=EDGE_LOOP('',(#12328,#12329,#12330,#12331));
#3384=EDGE_LOOP('',(#12332,#12333,#12334,#12335));
#3385=EDGE_LOOP('',(#12336,#12337,#12338,#12339));
#3386=EDGE_LOOP('',(#12340,#12341,#12342,#12343));
#3387=EDGE_LOOP('',(#12344,#12345,#12346,#12347));
#3388=EDGE_LOOP('',(#12348,#12349,#12350,#12351));
#3389=EDGE_LOOP('',(#12352,#12353,#12354,#12355));
#3390=EDGE_LOOP('',(#12356,#12357,#12358,#12359));
#3391=EDGE_LOOP('',(#12360,#12361,#12362,#12363,#12364,#12365,#12366,#12367,
#12368,#12369,#12370,#12371,#12372,#12373,#12374,#12375,#12376,#12377,#12378,
#12379,#12380,#12381,#12382,#12383,#12384,#12385,#12386,#12387,#12388,#12389,
#12390,#12391,#12392,#12393,#12394,#12395,#12396,#12397,#12398,#12399,#12400,
#12401,#12402,#12403,#12404,#12405,#12406,#12407,#12408,#12409,#12410,#12411,
#12412,#12413,#12414,#12415,#12416,#12417,#12418,#12419,#12420,#12421,#12422,
#12423,#12424,#12425,#12426,#12427,#12428,#12429,#12430,#12431,#12432,#12433,
#12434,#12435,#12436,#12437,#12438,#12439,#12440,#12441,#12442,#12443,#12444,
#12445,#12446,#12447,#12448,#12449,#12450,#12451,#12452,#12453,#12454,#12455,
#12456,#12457,#12458,#12459,#12460,#12461,#12462,#12463,#12464,#12465,#12466,
#12467,#12468,#12469,#12470,#12471,#12472,#12473,#12474,#12475,#12476,#12477,
#12478,#12479,#12480,#12481,#12482,#12483,#12484,#12485,#12486,#12487,#12488,
#12489,#12490,#12491,#12492,#12493,#12494,#12495,#12496,#12497,#12498,#12499,
#12500,#12501,#12502,#12503,#12504,#12505,#12506,#12507,#12508,#12509,#12510,
#12511,#12512,#12513,#12514,#12515,#12516,#12517,#12518,#12519));
#3392=EDGE_LOOP('',(#12520));
#3393=EDGE_LOOP('',(#12521,#12522,#12523,#12524));
#3394=EDGE_LOOP('',(#12525,#12526,#12527,#12528));
#3395=EDGE_LOOP('',(#12529,#12530,#12531,#12532));
#3396=EDGE_LOOP('',(#12533,#12534,#12535,#12536));
#3397=EDGE_LOOP('',(#12537,#12538,#12539,#12540));
#3398=EDGE_LOOP('',(#12541,#12542,#12543,#12544));
#3399=EDGE_LOOP('',(#12545,#12546,#12547,#12548));
#3400=EDGE_LOOP('',(#12549,#12550,#12551,#12552,#12553,#12554));
#3401=EDGE_LOOP('',(#12555,#12556,#12557,#12558,#12559,#12560));
#3402=EDGE_LOOP('',(#12561));
#3403=EDGE_LOOP('',(#12562));
#3404=EDGE_LOOP('',(#12563,#12564,#12565,#12566));
#3405=EDGE_LOOP('',(#12567,#12568,#12569,#12570));
#3406=EDGE_LOOP('',(#12571,#12572,#12573,#12574));
#3407=EDGE_LOOP('',(#12575));
#3408=EDGE_LOOP('',(#12576));
#3409=EDGE_LOOP('',(#12577,#12578,#12579,#12580));
#3410=EDGE_LOOP('',(#12581,#12582,#12583,#12584));
#3411=LINE('',#19240,#4300);
#3412=LINE('',#19246,#4301);
#3413=LINE('',#19252,#4302);
#3414=LINE('',#19258,#4303);
#3415=LINE('',#19264,#4304);
#3416=LINE('',#19270,#4305);
#3417=LINE('',#19276,#4306);
#3418=LINE('',#19282,#4307);
#3419=LINE('',#19288,#4308);
#3420=LINE('',#19294,#4309);
#3421=LINE('',#19300,#4310);
#3422=LINE('',#19306,#4311);
#3423=LINE('',#19311,#4312);
#3424=LINE('',#19313,#4313);
#3425=LINE('',#19315,#4314);
#3426=LINE('',#19316,#4315);
#3427=LINE('',#19319,#4316);
#3428=LINE('',#19321,#4317);
#3429=LINE('',#19322,#4318);
#3430=LINE('',#19325,#4319);
#3431=LINE('',#19327,#4320);
#3432=LINE('',#19328,#4321);
#3433=LINE('',#19330,#4322);
#3434=LINE('',#19331,#4323);
#3435=LINE('',#19338,#4324);
#3436=LINE('',#19340,#4325);
#3437=LINE('',#19342,#4326);
#3438=LINE('',#19343,#4327);
#3439=LINE('',#19346,#4328);
#3440=LINE('',#19348,#4329);
#3441=LINE('',#19349,#4330);
#3442=LINE('',#19352,#4331);
#3443=LINE('',#19354,#4332);
#3444=LINE('',#19355,#4333);
#3445=LINE('',#19357,#4334);
#3446=LINE('',#19358,#4335);
#3447=LINE('',#19365,#4336);
#3448=LINE('',#19367,#4337);
#3449=LINE('',#19369,#4338);
#3450=LINE('',#19370,#4339);
#3451=LINE('',#19373,#4340);
#3452=LINE('',#19375,#4341);
#3453=LINE('',#19376,#4342);
#3454=LINE('',#19379,#4343);
#3455=LINE('',#19381,#4344);
#3456=LINE('',#19382,#4345);
#3457=LINE('',#19384,#4346);
#3458=LINE('',#19385,#4347);
#3459=LINE('',#19429,#4348);
#3460=LINE('',#19471,#4349);
#3461=LINE('',#19478,#4350);
#3462=LINE('',#19485,#4351);
#3463=LINE('',#19492,#4352);
#3464=LINE('',#19502,#4353);
#3465=LINE('',#19505,#4354);
#3466=LINE('',#19509,#4355);
#3467=LINE('',#19513,#4356);
#3468=LINE('',#19520,#4357);
#3469=LINE('',#19524,#4358);
#3470=LINE('',#19531,#4359);
#3471=LINE('',#19535,#4360);
#3472=LINE('',#19543,#4361);
#3473=LINE('',#19563,#4362);
#3474=LINE('',#19567,#4363);
#3475=LINE('',#19571,#4364);
#3476=LINE('',#19575,#4365);
#3477=LINE('',#19580,#4366);
#3478=LINE('',#19587,#4367);
#3479=LINE('',#19591,#4368);
#3480=LINE('',#19600,#4369);
#3481=LINE('',#19606,#4370);
#3482=LINE('',#19614,#4371);
#3483=LINE('',#19618,#4372);
#3484=LINE('',#19623,#4373);
#3485=LINE('',#19627,#4374);
#3486=LINE('',#19632,#4375);
#3487=LINE('',#19636,#4376);
#3488=LINE('',#19641,#4377);
#3489=LINE('',#19645,#4378);
#3490=LINE('',#19664,#4379);
#3491=LINE('',#19672,#4380);
#3492=LINE('',#19679,#4381);
#3493=LINE('',#19685,#4382);
#3494=LINE('',#19691,#4383);
#3495=LINE('',#19697,#4384);
#3496=LINE('',#19703,#4385);
#3497=LINE('',#19710,#4386);
#3498=LINE('',#19718,#4387);
#3499=LINE('',#19748,#4388);
#3500=LINE('',#19759,#4389);
#3501=LINE('',#19763,#4390);
#3502=LINE('',#19767,#4391);
#3503=LINE('',#19771,#4392);
#3504=LINE('',#19775,#4393);
#3505=LINE('',#19779,#4394);
#3506=LINE('',#19780,#4395);
#3507=LINE('',#19784,#4396);
#3508=LINE('',#19785,#4397);
#3509=LINE('',#19789,#4398);
#3510=LINE('',#19794,#4399);
#3511=LINE('',#19798,#4400);
#3512=LINE('',#19799,#4401);
#3513=LINE('',#19801,#4402);
#3514=LINE('',#19804,#4403);
#3515=LINE('',#19805,#4404);
#3516=LINE('',#19807,#4405);
#3517=LINE('',#19810,#4406);
#3518=LINE('',#19812,#4407);
#3519=LINE('',#19813,#4408);
#3520=LINE('',#19816,#4409);
#3521=LINE('',#19817,#4410);
#3522=LINE('',#19819,#4411);
#3523=LINE('',#19822,#4412);
#3524=LINE('',#19824,#4413);
#3525=LINE('',#19825,#4414);
#3526=LINE('',#19828,#4415);
#3527=LINE('',#19830,#4416);
#3528=LINE('',#19831,#4417);
#3529=LINE('',#19834,#4418);
#3530=LINE('',#19835,#4419);
#3531=LINE('',#19838,#4420);
#3532=LINE('',#19840,#4421);
#3533=LINE('',#19841,#4422);
#3534=LINE('',#19843,#4423);
#3535=LINE('',#19844,#4424);
#3536=LINE('',#19847,#4425);
#3537=LINE('',#19849,#4426);
#3538=LINE('',#19850,#4427);
#3539=LINE('',#19852,#4428);
#3540=LINE('',#19855,#4429);
#3541=LINE('',#19857,#4430);
#3542=LINE('',#19859,#4431);
#3543=LINE('',#19860,#4432);
#3544=LINE('',#19866,#4433);
#3545=LINE('',#19869,#4434);
#3546=LINE('',#19872,#4435);
#3547=LINE('',#19875,#4436);
#3548=LINE('',#19877,#4437);
#3549=LINE('',#19885,#4438);
#3550=LINE('',#19891,#4439);
#3551=LINE('',#19900,#4440);
#3552=LINE('',#19909,#4441);
#3553=LINE('',#19918,#4442);
#3554=LINE('',#19927,#4443);
#3555=LINE('',#19936,#4444);
#3556=LINE('',#19945,#4445);
#3557=LINE('',#19953,#4446);
#3558=LINE('',#19957,#4447);
#3559=LINE('',#19961,#4448);
#3560=LINE('',#19965,#4449);
#3561=LINE('',#19969,#4450);
#3562=LINE('',#19971,#4451);
#3563=LINE('',#19973,#4452);
#3564=LINE('',#19974,#4453);
#3565=LINE('',#19977,#4454);
#3566=LINE('',#19979,#4455);
#3567=LINE('',#19980,#4456);
#3568=LINE('',#19983,#4457);
#3569=LINE('',#19985,#4458);
#3570=LINE('',#19986,#4459);
#3571=LINE('',#19989,#4460);
#3572=LINE('',#19991,#4461);
#3573=LINE('',#19992,#4462);
#3574=LINE('',#19995,#4463);
#3575=LINE('',#19997,#4464);
#3576=LINE('',#19998,#4465);
#3577=LINE('',#20001,#4466);
#3578=LINE('',#20003,#4467);
#3579=LINE('',#20004,#4468);
#3580=LINE('',#20007,#4469);
#3581=LINE('',#20009,#4470);
#3582=LINE('',#20010,#4471);
#3583=LINE('',#20013,#4472);
#3584=LINE('',#20015,#4473);
#3585=LINE('',#20016,#4474);
#3586=LINE('',#20019,#4475);
#3587=LINE('',#20021,#4476);
#3588=LINE('',#20022,#4477);
#3589=LINE('',#20025,#4478);
#3590=LINE('',#20027,#4479);
#3591=LINE('',#20028,#4480);
#3592=LINE('',#20031,#4481);
#3593=LINE('',#20033,#4482);
#3594=LINE('',#20034,#4483);
#3595=LINE('',#20036,#4484);
#3596=LINE('',#20037,#4485);
#3597=LINE('',#20054,#4486);
#3598=LINE('',#20060,#4487);
#3599=LINE('',#20064,#4488);
#3600=LINE('',#20070,#4489);
#3601=LINE('',#20075,#4490);
#3602=LINE('',#20090,#4491);
#3603=LINE('',#20099,#4492);
#3604=LINE('',#20103,#4493);
#3605=LINE('',#20107,#4494);
#3606=LINE('',#20110,#4495);
#3607=LINE('',#20246,#4496);
#3608=LINE('',#20499,#4497);
#3609=LINE('',#20541,#4498);
#3610=LINE('',#20546,#4499);
#3611=LINE('',#20555,#4500);
#3612=LINE('',#20560,#4501);
#3613=LINE('',#20573,#4502);
#3614=LINE('',#20577,#4503);
#3615=LINE('',#20581,#4504);
#3616=LINE('',#20588,#4505);
#3617=LINE('',#20592,#4506);
#3618=LINE('',#20596,#4507);
#3619=LINE('',#20601,#4508);
#3620=LINE('',#20603,#4509);
#3621=LINE('',#20605,#4510);
#3622=LINE('',#20606,#4511);
#3623=LINE('',#20609,#4512);
#3624=LINE('',#20611,#4513);
#3625=LINE('',#20612,#4514);
#3626=LINE('',#20615,#4515);
#3627=LINE('',#20617,#4516);
#3628=LINE('',#20618,#4517);
#3629=LINE('',#20621,#4518);
#3630=LINE('',#20623,#4519);
#3631=LINE('',#20624,#4520);
#3632=LINE('',#20627,#4521);
#3633=LINE('',#20629,#4522);
#3634=LINE('',#20630,#4523);
#3635=LINE('',#20632,#4524);
#3636=LINE('',#20633,#4525);
#3637=LINE('',#20642,#4526);
#3638=LINE('',#20648,#4527);
#3639=LINE('',#20654,#4528);
#3640=LINE('',#20660,#4529);
#3641=LINE('',#20666,#4530);
#3642=LINE('',#20671,#4531);
#3643=LINE('',#20673,#4532);
#3644=LINE('',#20675,#4533);
#3645=LINE('',#20676,#4534);
#3646=LINE('',#20679,#4535);
#3647=LINE('',#20681,#4536);
#3648=LINE('',#20682,#4537);
#3649=LINE('',#20685,#4538);
#3650=LINE('',#20687,#4539);
#3651=LINE('',#20688,#4540);
#3652=LINE('',#20690,#4541);
#3653=LINE('',#20691,#4542);
#3654=LINE('',#20697,#4543);
#3655=LINE('',#20703,#4544);
#3656=LINE('',#20709,#4545);
#3657=LINE('',#20715,#4546);
#3658=LINE('',#20720,#4547);
#3659=LINE('',#20724,#4548);
#3660=LINE('',#20728,#4549);
#3661=LINE('',#20730,#4550);
#3662=LINE('',#20732,#4551);
#3663=LINE('',#20734,#4552);
#3664=LINE('',#20735,#4553);
#3665=LINE('',#20738,#4554);
#3666=LINE('',#20739,#4555);
#3667=LINE('',#20742,#4556);
#3668=LINE('',#20743,#4557);
#3669=LINE('',#20746,#4558);
#3670=LINE('',#20747,#4559);
#3671=LINE('',#20750,#4560);
#3672=LINE('',#20751,#4561);
#3673=LINE('',#20753,#4562);
#3674=LINE('',#20759,#4563);
#3675=LINE('',#20761,#4564);
#3676=LINE('',#20763,#4565);
#3677=LINE('',#20764,#4566);
#3678=LINE('',#20767,#4567);
#3679=LINE('',#20769,#4568);
#3680=LINE('',#20770,#4569);
#3681=LINE('',#20773,#4570);
#3682=LINE('',#20775,#4571);
#3683=LINE('',#20776,#4572);
#3684=LINE('',#20778,#4573);
#3685=LINE('',#20779,#4574);
#3686=LINE('',#20823,#4575);
#3687=LINE('',#20865,#4576);
#3688=LINE('',#20872,#4577);
#3689=LINE('',#20879,#4578);
#3690=LINE('',#20886,#4579);
#3691=LINE('',#20892,#4580);
#3692=LINE('',#20896,#4581);
#3693=LINE('',#20903,#4582);
#3694=LINE('',#20907,#4583);
#3695=LINE('',#20914,#4584);
#3696=LINE('',#20918,#4585);
#3697=LINE('',#20925,#4586);
#3698=LINE('',#20929,#4587);
#3699=LINE('',#20937,#4588);
#3700=LINE('',#20957,#4589);
#3701=LINE('',#20961,#4590);
#3702=LINE('',#20965,#4591);
#3703=LINE('',#20969,#4592);
#3704=LINE('',#20974,#4593);
#3705=LINE('',#20981,#4594);
#3706=LINE('',#20985,#4595);
#3707=LINE('',#20994,#4596);
#3708=LINE('',#21000,#4597);
#3709=LINE('',#21009,#4598);
#3710=LINE('',#21015,#4599);
#3711=LINE('',#21021,#4600);
#3712=LINE('',#21027,#4601);
#3713=LINE('',#21033,#4602);
#3714=LINE('',#21039,#4603);
#3715=LINE('',#21048,#4604);
#3716=LINE('',#21052,#4605);
#3717=LINE('',#21056,#4606);
#3718=LINE('',#21060,#4607);
#3719=LINE('',#21064,#4608);
#3720=LINE('',#21068,#4609);
#3721=LINE('',#21072,#4610);
#3722=LINE('',#21076,#4611);
#3723=LINE('',#21080,#4612);
#3724=LINE('',#21084,#4613);
#3725=LINE('',#21088,#4614);
#3726=LINE('',#21092,#4615);
#3727=LINE('',#21096,#4616);
#3728=LINE('',#21100,#4617);
#3729=LINE('',#21104,#4618);
#3730=LINE('',#21108,#4619);
#3731=LINE('',#21110,#4620);
#3732=LINE('',#21112,#4621);
#3733=LINE('',#21114,#4622);
#3734=LINE('',#21116,#4623);
#3735=LINE('',#21118,#4624);
#3736=LINE('',#21119,#4625);
#3737=LINE('',#21121,#4626);
#3738=LINE('',#21123,#4627);
#3739=LINE('',#21125,#4628);
#3740=LINE('',#21127,#4629);
#3741=LINE('',#21129,#4630);
#3742=LINE('',#21130,#4631);
#3743=LINE('',#21133,#4632);
#3744=LINE('',#21135,#4633);
#3745=LINE('',#21137,#4634);
#3746=LINE('',#21139,#4635);
#3747=LINE('',#21140,#4636);
#3748=LINE('',#21142,#4637);
#3749=LINE('',#21144,#4638);
#3750=LINE('',#21146,#4639);
#3751=LINE('',#21148,#4640);
#3752=LINE('',#21149,#4641);
#3753=LINE('',#21152,#4642);
#3754=LINE('',#21153,#4643);
#3755=LINE('',#21156,#4644);
#3756=LINE('',#21157,#4645);
#3757=LINE('',#21160,#4646);
#3758=LINE('',#21161,#4647);
#3759=LINE('',#21164,#4648);
#3760=LINE('',#21165,#4649);
#3761=LINE('',#21167,#4650);
#3762=LINE('',#21170,#4651);
#3763=LINE('',#21171,#4652);
#3764=LINE('',#21174,#4653);
#3765=LINE('',#21175,#4654);
#3766=LINE('',#21178,#4655);
#3767=LINE('',#21179,#4656);
#3768=LINE('',#21182,#4657);
#3769=LINE('',#21183,#4658);
#3770=LINE('',#21185,#4659);
#3771=LINE('',#21191,#4660);
#3772=LINE('',#21193,#4661);
#3773=LINE('',#21195,#4662);
#3774=LINE('',#21196,#4663);
#3775=LINE('',#21199,#4664);
#3776=LINE('',#21201,#4665);
#3777=LINE('',#21202,#4666);
#3778=LINE('',#21205,#4667);
#3779=LINE('',#21207,#4668);
#3780=LINE('',#21208,#4669);
#3781=LINE('',#21211,#4670);
#3782=LINE('',#21213,#4671);
#3783=LINE('',#21214,#4672);
#3784=LINE('',#21217,#4673);
#3785=LINE('',#21219,#4674);
#3786=LINE('',#21220,#4675);
#3787=LINE('',#21223,#4676);
#3788=LINE('',#21225,#4677);
#3789=LINE('',#21226,#4678);
#3790=LINE('',#21229,#4679);
#3791=LINE('',#21231,#4680);
#3792=LINE('',#21232,#4681);
#3793=LINE('',#21234,#4682);
#3794=LINE('',#21235,#4683);
#3795=LINE('',#21242,#4684);
#3796=LINE('',#21244,#4685);
#3797=LINE('',#21246,#4686);
#3798=LINE('',#21247,#4687);
#3799=LINE('',#21250,#4688);
#3800=LINE('',#21252,#4689);
#3801=LINE('',#21253,#4690);
#3802=LINE('',#21256,#4691);
#3803=LINE('',#21258,#4692);
#3804=LINE('',#21259,#4693);
#3805=LINE('',#21262,#4694);
#3806=LINE('',#21264,#4695);
#3807=LINE('',#21265,#4696);
#3808=LINE('',#21268,#4697);
#3809=LINE('',#21270,#4698);
#3810=LINE('',#21271,#4699);
#3811=LINE('',#21274,#4700);
#3812=LINE('',#21276,#4701);
#3813=LINE('',#21277,#4702);
#3814=LINE('',#21280,#4703);
#3815=LINE('',#21282,#4704);
#3816=LINE('',#21283,#4705);
#3817=LINE('',#21285,#4706);
#3818=LINE('',#21286,#4707);
#3819=LINE('',#21296,#4708);
#3820=LINE('',#21298,#4709);
#3821=LINE('',#21300,#4710);
#3822=LINE('',#21301,#4711);
#3823=LINE('',#21304,#4712);
#3824=LINE('',#21306,#4713);
#3825=LINE('',#21307,#4714);
#3826=LINE('',#21310,#4715);
#3827=LINE('',#21312,#4716);
#3828=LINE('',#21313,#4717);
#3829=LINE('',#21316,#4718);
#3830=LINE('',#21318,#4719);
#3831=LINE('',#21319,#4720);
#3832=LINE('',#21322,#4721);
#3833=LINE('',#21324,#4722);
#3834=LINE('',#21325,#4723);
#3835=LINE('',#21327,#4724);
#3836=LINE('',#21328,#4725);
#3837=LINE('',#21336,#4726);
#3838=LINE('',#21340,#4727);
#3839=LINE('',#21344,#4728);
#3840=LINE('',#21350,#4729);
#3841=LINE('',#21352,#4730);
#3842=LINE('',#21354,#4731);
#3843=LINE('',#21355,#4732);
#3844=LINE('',#21358,#4733);
#3845=LINE('',#21360,#4734);
#3846=LINE('',#21361,#4735);
#3847=LINE('',#21364,#4736);
#3848=LINE('',#21366,#4737);
#3849=LINE('',#21367,#4738);
#3850=LINE('',#21370,#4739);
#3851=LINE('',#21372,#4740);
#3852=LINE('',#21373,#4741);
#3853=LINE('',#21376,#4742);
#3854=LINE('',#21378,#4743);
#3855=LINE('',#21379,#4744);
#3856=LINE('',#21381,#4745);
#3857=LINE('',#21382,#4746);
#3858=LINE('',#21394,#4747);
#3859=LINE('',#21398,#4748);
#3860=LINE('',#21402,#4749);
#3861=LINE('',#21409,#4750);
#3862=LINE('',#21411,#4751);
#3863=LINE('',#21426,#4752);
#3864=LINE('',#21432,#4753);
#3865=LINE('',#21436,#4754);
#3866=LINE('',#21442,#4755);
#3867=LINE('',#21447,#4756);
#3868=LINE('',#21462,#4757);
#3869=LINE('',#21471,#4758);
#3870=LINE('',#21475,#4759);
#3871=LINE('',#21479,#4760);
#3872=LINE('',#21482,#4761);
#3873=LINE('',#21635,#4762);
#3874=LINE('',#21931,#4763);
#3875=LINE('',#21973,#4764);
#3876=LINE('',#21978,#4765);
#3877=LINE('',#21987,#4766);
#3878=LINE('',#21992,#4767);
#3879=LINE('',#22004,#4768);
#3880=LINE('',#22010,#4769);
#3881=LINE('',#22012,#4770);
#3882=LINE('',#22014,#4771);
#3883=LINE('',#22015,#4772);
#3884=LINE('',#22020,#4773);
#3885=LINE('',#22021,#4774);
#3886=LINE('',#22024,#4775);
#3887=LINE('',#22025,#4776);
#3888=LINE('',#22028,#4777);
#3889=LINE('',#22029,#4778);
#3890=LINE('',#22043,#4779);
#3891=LINE('',#22046,#4780);
#3892=LINE('',#22051,#4781);
#3893=LINE('',#22059,#4782);
#3894=LINE('',#22065,#4783);
#3895=LINE('',#22074,#4784);
#3896=LINE('',#22080,#4785);
#3897=LINE('',#22089,#4786);
#3898=LINE('',#22095,#4787);
#3899=LINE('',#22103,#4788);
#3900=LINE('',#22108,#4789);
#3901=LINE('',#22114,#4790);
#3902=LINE('',#22143,#4791);
#3903=LINE('',#22166,#4792);
#3904=LINE('',#22171,#4793);
#3905=LINE('',#22177,#4794);
#3906=LINE('',#22185,#4795);
#3907=LINE('',#22187,#4796);
#3908=LINE('',#22189,#4797);
#3909=LINE('',#22190,#4798);
#3910=LINE('',#22193,#4799);
#3911=LINE('',#22195,#4800);
#3912=LINE('',#22196,#4801);
#3913=LINE('',#22199,#4802);
#3914=LINE('',#22201,#4803);
#3915=LINE('',#22202,#4804);
#3916=LINE('',#22204,#4805);
#3917=LINE('',#22205,#4806);
#3918=LINE('',#22213,#4807);
#3919=LINE('',#22219,#4808);
#3920=LINE('',#22227,#4809);
#3921=LINE('',#22229,#4810);
#3922=LINE('',#22231,#4811);
#3923=LINE('',#22232,#4812);
#3924=LINE('',#22235,#4813);
#3925=LINE('',#22237,#4814);
#3926=LINE('',#22238,#4815);
#3927=LINE('',#22241,#4816);
#3928=LINE('',#22243,#4817);
#3929=LINE('',#22244,#4818);
#3930=LINE('',#22321,#4819);
#3931=LINE('',#22467,#4820);
#3932=LINE('',#22613,#4821);
#3933=LINE('',#22759,#4822);
#3934=LINE('',#22905,#4823);
#3935=LINE('',#23051,#4824);
#3936=LINE('',#23197,#4825);
#3937=LINE('',#23343,#4826);
#3938=LINE('',#23489,#4827);
#3939=LINE('',#23635,#4828);
#3940=LINE('',#23781,#4829);
#3941=LINE('',#23927,#4830);
#3942=LINE('',#24073,#4831);
#3943=LINE('',#24219,#4832);
#3944=LINE('',#24365,#4833);
#3945=LINE('',#24511,#4834);
#3946=LINE('',#24657,#4835);
#3947=LINE('',#24803,#4836);
#3948=LINE('',#24949,#4837);
#3949=LINE('',#25095,#4838);
#3950=LINE('',#25173,#4839);
#3951=LINE('',#25317,#4840);
#3952=LINE('',#25389,#4841);
#3953=LINE('',#25392,#4842);
#3954=LINE('',#25393,#4843);
#3955=LINE('',#25605,#4844);
#3956=LINE('',#25609,#4845);
#3957=LINE('',#25821,#4846);
#3958=LINE('',#25824,#4847);
#3959=LINE('',#25825,#4848);
#3960=LINE('',#26037,#4849);
#3961=LINE('',#26041,#4850);
#3962=LINE('',#26253,#4851);
#3963=LINE('',#26256,#4852);
#3964=LINE('',#26257,#4853);
#3965=LINE('',#26469,#4854);
#3966=LINE('',#26473,#4855);
#3967=LINE('',#26685,#4856);
#3968=LINE('',#26688,#4857);
#3969=LINE('',#26689,#4858);
#3970=LINE('',#26901,#4859);
#3971=LINE('',#26905,#4860);
#3972=LINE('',#27117,#4861);
#3973=LINE('',#27120,#4862);
#3974=LINE('',#27121,#4863);
#3975=LINE('',#27333,#4864);
#3976=LINE('',#27337,#4865);
#3977=LINE('',#27549,#4866);
#3978=LINE('',#27552,#4867);
#3979=LINE('',#27553,#4868);
#3980=LINE('',#27765,#4869);
#3981=LINE('',#27769,#4870);
#3982=LINE('',#27981,#4871);
#3983=LINE('',#27984,#4872);
#3984=LINE('',#27985,#4873);
#3985=LINE('',#28197,#4874);
#3986=LINE('',#28201,#4875);
#3987=LINE('',#28413,#4876);
#3988=LINE('',#28416,#4877);
#3989=LINE('',#28417,#4878);
#3990=LINE('',#28629,#4879);
#3991=LINE('',#28633,#4880);
#3992=LINE('',#28845,#4881);
#3993=LINE('',#28848,#4882);
#3994=LINE('',#28849,#4883);
#3995=LINE('',#29061,#4884);
#3996=LINE('',#29065,#4885);
#3997=LINE('',#29277,#4886);
#3998=LINE('',#29280,#4887);
#3999=LINE('',#29281,#4888);
#4000=LINE('',#29493,#4889);
#4001=LINE('',#29497,#4890);
#4002=LINE('',#29709,#4891);
#4003=LINE('',#29712,#4892);
#4004=LINE('',#29713,#4893);
#4005=LINE('',#29925,#4894);
#4006=LINE('',#29929,#4895);
#4007=LINE('',#30141,#4896);
#4008=LINE('',#30144,#4897);
#4009=LINE('',#30145,#4898);
#4010=LINE('',#30357,#4899);
#4011=LINE('',#30361,#4900);
#4012=LINE('',#30573,#4901);
#4013=LINE('',#30576,#4902);
#4014=LINE('',#30577,#4903);
#4015=LINE('',#30789,#4904);
#4016=LINE('',#30793,#4905);
#4017=LINE('',#31005,#4906);
#4018=LINE('',#31008,#4907);
#4019=LINE('',#31009,#4908);
#4020=LINE('',#31221,#4909);
#4021=LINE('',#31225,#4910);
#4022=LINE('',#31437,#4911);
#4023=LINE('',#31440,#4912);
#4024=LINE('',#31441,#4913);
#4025=LINE('',#31653,#4914);
#4026=LINE('',#31657,#4915);
#4027=LINE('',#31869,#4916);
#4028=LINE('',#31872,#4917);
#4029=LINE('',#31873,#4918);
#4030=LINE('',#32085,#4919);
#4031=LINE('',#32089,#4920);
#4032=LINE('',#32301,#4921);
#4033=LINE('',#32304,#4922);
#4034=LINE('',#32305,#4923);
#4035=LINE('',#32517,#4924);
#4036=LINE('',#32521,#4925);
#4037=LINE('',#32733,#4926);
#4038=LINE('',#32736,#4927);
#4039=LINE('',#32737,#4928);
#4040=LINE('',#32949,#4929);
#4041=LINE('',#32953,#4930);
#4042=LINE('',#33165,#4931);
#4043=LINE('',#33168,#4932);
#4044=LINE('',#33169,#4933);
#4045=LINE('',#33381,#4934);
#4046=LINE('',#33385,#4935);
#4047=LINE('',#33597,#4936);
#4048=LINE('',#33600,#4937);
#4049=LINE('',#33601,#4938);
#4050=LINE('',#33813,#4939);
#4051=LINE('',#33823,#4940);
#4052=LINE('',#33829,#4941);
#4053=LINE('',#33831,#4942);
#4054=LINE('',#33833,#4943);
#4055=LINE('',#33834,#4944);
#4056=LINE('',#33839,#4945);
#4057=LINE('',#33840,#4946);
#4058=LINE('',#33843,#4947);
#4059=LINE('',#33844,#4948);
#4060=LINE('',#33847,#4949);
#4061=LINE('',#33848,#4950);
#4062=LINE('',#33862,#4951);
#4063=LINE('',#33865,#4952);
#4064=LINE('',#33870,#4953);
#4065=LINE('',#33878,#4954);
#4066=LINE('',#33884,#4955);
#4067=LINE('',#33893,#4956);
#4068=LINE('',#33899,#4957);
#4069=LINE('',#33944,#4958);
#4070=LINE('',#33986,#4959);
#4071=LINE('',#33992,#4960);
#4072=LINE('',#34000,#4961);
#4073=LINE('',#34002,#4962);
#4074=LINE('',#34004,#4963);
#4075=LINE('',#34005,#4964);
#4076=LINE('',#34008,#4965);
#4077=LINE('',#34010,#4966);
#4078=LINE('',#34011,#4967);
#4079=LINE('',#34014,#4968);
#4080=LINE('',#34016,#4969);
#4081=LINE('',#34017,#4970);
#4082=LINE('',#34019,#4971);
#4083=LINE('',#34020,#4972);
#4084=LINE('',#34028,#4973);
#4085=LINE('',#34034,#4974);
#4086=LINE('',#34045,#4975);
#4087=LINE('',#34047,#4976);
#4088=LINE('',#34049,#4977);
#4089=LINE('',#34050,#4978);
#4090=LINE('',#34053,#4979);
#4091=LINE('',#34055,#4980);
#4092=LINE('',#34056,#4981);
#4093=LINE('',#34059,#4982);
#4094=LINE('',#34061,#4983);
#4095=LINE('',#34062,#4984);
#4096=LINE('',#34065,#4985);
#4097=LINE('',#34067,#4986);
#4098=LINE('',#34068,#4987);
#4099=LINE('',#34071,#4988);
#4100=LINE('',#34073,#4989);
#4101=LINE('',#34074,#4990);
#4102=LINE('',#34076,#4991);
#4103=LINE('',#34077,#4992);
#4104=LINE('',#34085,#4993);
#4105=LINE('',#34087,#4994);
#4106=LINE('',#34092,#4995);
#4107=LINE('',#34094,#4996);
#4108=LINE('',#34096,#4997);
#4109=LINE('',#34097,#4998);
#4110=LINE('',#34100,#4999);
#4111=LINE('',#34102,#5000);
#4112=LINE('',#34103,#5001);
#4113=LINE('',#34106,#5002);
#4114=LINE('',#34108,#5003);
#4115=LINE('',#34109,#5004);
#4116=LINE('',#34186,#5005);
#4117=LINE('',#34332,#5006);
#4118=LINE('',#34478,#5007);
#4119=LINE('',#34624,#5008);
#4120=LINE('',#34770,#5009);
#4121=LINE('',#34916,#5010);
#4122=LINE('',#35062,#5011);
#4123=LINE('',#35208,#5012);
#4124=LINE('',#35354,#5013);
#4125=LINE('',#35500,#5014);
#4126=LINE('',#35646,#5015);
#4127=LINE('',#35792,#5016);
#4128=LINE('',#35938,#5017);
#4129=LINE('',#36084,#5018);
#4130=LINE('',#36230,#5019);
#4131=LINE('',#36376,#5020);
#4132=LINE('',#36522,#5021);
#4133=LINE('',#36668,#5022);
#4134=LINE('',#36814,#5023);
#4135=LINE('',#36960,#5024);
#4136=LINE('',#37106,#5025);
#4137=LINE('',#37252,#5026);
#4138=LINE('',#37398,#5027);
#4139=LINE('',#37544,#5028);
#4140=LINE('',#37690,#5029);
#4141=LINE('',#37836,#5030);
#4142=LINE('',#37982,#5031);
#4143=LINE('',#38128,#5032);
#4144=LINE('',#38274,#5033);
#4145=LINE('',#38420,#5034);
#4146=LINE('',#38566,#5035);
#4147=LINE('',#38712,#5036);
#4148=LINE('',#38858,#5037);
#4149=LINE('',#39004,#5038);
#4150=LINE('',#39150,#5039);
#4151=LINE('',#39296,#5040);
#4152=LINE('',#39442,#5041);
#4153=LINE('',#39588,#5042);
#4154=LINE('',#39734,#5043);
#4155=LINE('',#39880,#5044);
#4156=LINE('',#39958,#5045);
#4157=LINE('',#40179,#5046);
#4158=LINE('',#40328,#5047);
#4159=LINE('',#40400,#5048);
#4160=LINE('',#40621,#5049);
#4161=LINE('',#40770,#5050);
#4162=LINE('',#40842,#5051);
#4163=LINE('',#41063,#5052);
#4164=LINE('',#41212,#5053);
#4165=LINE('',#41284,#5054);
#4166=LINE('',#41505,#5055);
#4167=LINE('',#41654,#5056);
#4168=LINE('',#41726,#5057);
#4169=LINE('',#41947,#5058);
#4170=LINE('',#42096,#5059);
#4171=LINE('',#42168,#5060);
#4172=LINE('',#42389,#5061);
#4173=LINE('',#42538,#5062);
#4174=LINE('',#42610,#5063);
#4175=LINE('',#42831,#5064);
#4176=LINE('',#42980,#5065);
#4177=LINE('',#43052,#5066);
#4178=LINE('',#43273,#5067);
#4179=LINE('',#43422,#5068);
#4180=LINE('',#43494,#5069);
#4181=LINE('',#43715,#5070);
#4182=LINE('',#43864,#5071);
#4183=LINE('',#43936,#5072);
#4184=LINE('',#44157,#5073);
#4185=LINE('',#44306,#5074);
#4186=LINE('',#44378,#5075);
#4187=LINE('',#44599,#5076);
#4188=LINE('',#44748,#5077);
#4189=LINE('',#44820,#5078);
#4190=LINE('',#45041,#5079);
#4191=LINE('',#45190,#5080);
#4192=LINE('',#45262,#5081);
#4193=LINE('',#45483,#5082);
#4194=LINE('',#45632,#5083);
#4195=LINE('',#45704,#5084);
#4196=LINE('',#45925,#5085);
#4197=LINE('',#46074,#5086);
#4198=LINE('',#46146,#5087);
#4199=LINE('',#46367,#5088);
#4200=LINE('',#46516,#5089);
#4201=LINE('',#46588,#5090);
#4202=LINE('',#46809,#5091);
#4203=LINE('',#46958,#5092);
#4204=LINE('',#47030,#5093);
#4205=LINE('',#47251,#5094);
#4206=LINE('',#47400,#5095);
#4207=LINE('',#47472,#5096);
#4208=LINE('',#47693,#5097);
#4209=LINE('',#47842,#5098);
#4210=LINE('',#47914,#5099);
#4211=LINE('',#48135,#5100);
#4212=LINE('',#48284,#5101);
#4213=LINE('',#48356,#5102);
#4214=LINE('',#48577,#5103);
#4215=LINE('',#48726,#5104);
#4216=LINE('',#48798,#5105);
#4217=LINE('',#49019,#5106);
#4218=LINE('',#49168,#5107);
#4219=LINE('',#49240,#5108);
#4220=LINE('',#49461,#5109);
#4221=LINE('',#49610,#5110);
#4222=LINE('',#49682,#5111);
#4223=LINE('',#49903,#5112);
#4224=LINE('',#50052,#5113);
#4225=LINE('',#50124,#5114);
#4226=LINE('',#50345,#5115);
#4227=LINE('',#50494,#5116);
#4228=LINE('',#50566,#5117);
#4229=LINE('',#50787,#5118);
#4230=LINE('',#50936,#5119);
#4231=LINE('',#51008,#5120);
#4232=LINE('',#51229,#5121);
#4233=LINE('',#51378,#5122);
#4234=LINE('',#51450,#5123);
#4235=LINE('',#51671,#5124);
#4236=LINE('',#51820,#5125);
#4237=LINE('',#51892,#5126);
#4238=LINE('',#52113,#5127);
#4239=LINE('',#52262,#5128);
#4240=LINE('',#52334,#5129);
#4241=LINE('',#52555,#5130);
#4242=LINE('',#52704,#5131);
#4243=LINE('',#52776,#5132);
#4244=LINE('',#52997,#5133);
#4245=LINE('',#53146,#5134);
#4246=LINE('',#53218,#5135);
#4247=LINE('',#53439,#5136);
#4248=LINE('',#53588,#5137);
#4249=LINE('',#53660,#5138);
#4250=LINE('',#53881,#5139);
#4251=LINE('',#54030,#5140);
#4252=LINE('',#54102,#5141);
#4253=LINE('',#54323,#5142);
#4254=LINE('',#54472,#5143);
#4255=LINE('',#54544,#5144);
#4256=LINE('',#54765,#5145);
#4257=LINE('',#54914,#5146);
#4258=LINE('',#54986,#5147);
#4259=LINE('',#55207,#5148);
#4260=LINE('',#55356,#5149);
#4261=LINE('',#55428,#5150);
#4262=LINE('',#55649,#5151);
#4263=LINE('',#55798,#5152);
#4264=LINE('',#55870,#5153);
#4265=LINE('',#56091,#5154);
#4266=LINE('',#56240,#5155);
#4267=LINE('',#56312,#5156);
#4268=LINE('',#56533,#5157);
#4269=LINE('',#56682,#5158);
#4270=LINE('',#56754,#5159);
#4271=LINE('',#56975,#5160);
#4272=LINE('',#56978,#5161);
#4273=LINE('',#56979,#5162);
#4274=LINE('',#57354,#5163);
#4275=LINE('',#57636,#5164);
#4276=LINE('',#57638,#5165);
#4277=LINE('',#57646,#5166);
#4278=LINE('',#57648,#5167);
#4279=LINE('',#57650,#5168);
#4280=LINE('',#57651,#5169);
#4281=LINE('',#57654,#5170);
#4282=LINE('',#57656,#5171);
#4283=LINE('',#57657,#5172);
#4284=LINE('',#57660,#5173);
#4285=LINE('',#57662,#5174);
#4286=LINE('',#57663,#5175);
#4287=LINE('',#57666,#5176);
#4288=LINE('',#57668,#5177);
#4289=LINE('',#57669,#5178);
#4290=LINE('',#57672,#5179);
#4291=LINE('',#57674,#5180);
#4292=LINE('',#57675,#5181);
#4293=LINE('',#57677,#5182);
#4294=LINE('',#57678,#5183);
#4295=LINE('',#57690,#5184);
#4296=LINE('',#57694,#5185);
#4297=LINE('',#57698,#5186);
#4298=LINE('',#57705,#5187);
#4299=LINE('',#57707,#5188);
#4300=VECTOR('',#15588,0.164999999999999);
#4301=VECTOR('',#15595,0.164999999999999);
#4302=VECTOR('',#15602,0.164999999999999);
#4303=VECTOR('',#15609,0.164999999999999);
#4304=VECTOR('',#15616,0.21);
#4305=VECTOR('',#15623,0.21);
#4306=VECTOR('',#15630,0.21);
#4307=VECTOR('',#15637,0.21);
#4308=VECTOR('',#15644,0.164999999999999);
#4309=VECTOR('',#15651,0.164999999999999);
#4310=VECTOR('',#15658,0.165);
#4311=VECTOR('',#15665,0.165);
#4312=VECTOR('',#15670,1.);
#4313=VECTOR('',#15671,1.);
#4314=VECTOR('',#15672,1.);
#4315=VECTOR('',#15673,1.);
#4316=VECTOR('',#15676,1.);
#4317=VECTOR('',#15677,1.);
#4318=VECTOR('',#15678,1.);
#4319=VECTOR('',#15681,1.);
#4320=VECTOR('',#15682,1.);
#4321=VECTOR('',#15683,1.);
#4322=VECTOR('',#15686,1.);
#4323=VECTOR('',#15687,1.);
#4324=VECTOR('',#15696,1.);
#4325=VECTOR('',#15697,1.);
#4326=VECTOR('',#15698,1.);
#4327=VECTOR('',#15699,1.);
#4328=VECTOR('',#15702,1.);
#4329=VECTOR('',#15703,1.);
#4330=VECTOR('',#15704,1.);
#4331=VECTOR('',#15707,1.);
#4332=VECTOR('',#15708,1.);
#4333=VECTOR('',#15709,1.);
#4334=VECTOR('',#15712,1.);
#4335=VECTOR('',#15713,1.);
#4336=VECTOR('',#15722,1.);
#4337=VECTOR('',#15723,1.);
#4338=VECTOR('',#15724,1.);
#4339=VECTOR('',#15725,1.);
#4340=VECTOR('',#15728,1.);
#4341=VECTOR('',#15729,1.);
#4342=VECTOR('',#15730,1.);
#4343=VECTOR('',#15733,1.);
#4344=VECTOR('',#15734,1.);
#4345=VECTOR('',#15735,1.);
#4346=VECTOR('',#15738,1.);
#4347=VECTOR('',#15739,1.);
#4348=VECTOR('',#15748,0.25);
#4349=VECTOR('',#15753,0.165);
#4350=VECTOR('',#15762,0.165);
#4351=VECTOR('',#15771,0.165);
#4352=VECTOR('',#15780,0.165);
#4353=VECTOR('',#15793,1.);
#4354=VECTOR('',#15796,1.);
#4355=VECTOR('',#15799,1.);
#4356=VECTOR('',#15802,1.);
#4357=VECTOR('',#15811,1.);
#4358=VECTOR('',#15814,1.);
#4359=VECTOR('',#15823,1.);
#4360=VECTOR('',#15826,1.);
#4361=VECTOR('',#15837,2.2);
#4362=VECTOR('',#15864,0.275);
#4363=VECTOR('',#15869,0.275);
#4364=VECTOR('',#15874,0.275);
#4365=VECTOR('',#15879,0.275);
#4366=VECTOR('',#15884,1.6);
#4367=VECTOR('',#15893,3.);
#4368=VECTOR('',#15898,1.3);
#4369=VECTOR('',#15911,1.1);
#4370=VECTOR('',#15918,1.59);
#4371=VECTOR('',#15929,1.);
#4372=VECTOR('',#15932,1.);
#4373=VECTOR('',#15937,1.);
#4374=VECTOR('',#15940,1.);
#4375=VECTOR('',#15945,1.);
#4376=VECTOR('',#15948,1.);
#4377=VECTOR('',#15953,1.);
#4378=VECTOR('',#15956,1.);
#4379=VECTOR('',#15989,1.59);
#4380=VECTOR('',#16000,1.1);
#4381=VECTOR('',#16009,0.225);
#4382=VECTOR('',#16016,0.225);
#4383=VECTOR('',#16023,0.225);
#4384=VECTOR('',#16030,0.225);
#4385=VECTOR('',#16037,0.6);
#4386=VECTOR('',#16046,1.5);
#4387=VECTOR('',#16057,1.);
#4388=VECTOR('',#16064,0.164999999999999);
#4389=VECTOR('',#16069,1.);
#4390=VECTOR('',#16072,1.);
#4391=VECTOR('',#16075,1.);
#4392=VECTOR('',#16078,1.);
#4393=VECTOR('',#16081,1.);
#4394=VECTOR('',#16084,1.);
#4395=VECTOR('',#16085,1.);
#4396=VECTOR('',#16088,1.);
#4397=VECTOR('',#16089,1.);
#4398=VECTOR('',#16092,1.);
#4399=VECTOR('',#16097,1.);
#4400=VECTOR('',#16100,1.);
#4401=VECTOR('',#16101,1.);
#4402=VECTOR('',#16104,1.);
#4403=VECTOR('',#16107,1.);
#4404=VECTOR('',#16108,1.);
#4405=VECTOR('',#16109,1.);
#4406=VECTOR('',#16112,1.);
#4407=VECTOR('',#16113,1.);
#4408=VECTOR('',#16114,1.);
#4409=VECTOR('',#16117,1.);
#4410=VECTOR('',#16118,1.);
#4411=VECTOR('',#16121,1.);
#4412=VECTOR('',#16124,1.);
#4413=VECTOR('',#16125,1.);
#4414=VECTOR('',#16126,1.);
#4415=VECTOR('',#16129,1.);
#4416=VECTOR('',#16130,1.);
#4417=VECTOR('',#16131,1.);
#4418=VECTOR('',#16134,1.);
#4419=VECTOR('',#16135,1.);
#4420=VECTOR('',#16138,1.);
#4421=VECTOR('',#16139,1.);
#4422=VECTOR('',#16140,1.);
#4423=VECTOR('',#16143,1.);
#4424=VECTOR('',#16144,1.);
#4425=VECTOR('',#16147,1.);
#4426=VECTOR('',#16148,1.);
#4427=VECTOR('',#16149,1.);
#4428=VECTOR('',#16152,1.);
#4429=VECTOR('',#16157,1.);
#4430=VECTOR('',#16160,1.);
#4431=VECTOR('',#16161,1.);
#4432=VECTOR('',#16162,1.);
#4433=VECTOR('',#16169,0.605);
#4434=VECTOR('',#16172,1.);
#4435=VECTOR('',#16177,1.);
#4436=VECTOR('',#16182,1.);
#4437=VECTOR('',#16185,1.);
#4438=VECTOR('',#16196,0.205);
#4439=VECTOR('',#16203,1.);
#4440=VECTOR('',#16216,1.);
#4441=VECTOR('',#16229,0.2);
#4442=VECTOR('',#16242,0.375);
#4443=VECTOR('',#16253,0.375);
#4444=VECTOR('',#16264,0.375);
#4445=VECTOR('',#16275,0.375);
#4446=VECTOR('',#16286,0.225);
#4447=VECTOR('',#16291,0.225);
#4448=VECTOR('',#16296,0.225);
#4449=VECTOR('',#16301,0.225000000000001);
#4450=VECTOR('',#16304,1.);
#4451=VECTOR('',#16305,1.);
#4452=VECTOR('',#16306,1.);
#4453=VECTOR('',#16307,1.);
#4454=VECTOR('',#16310,1.);
#4455=VECTOR('',#16311,1.);
#4456=VECTOR('',#16312,1.);
#4457=VECTOR('',#16315,1.);
#4458=VECTOR('',#16316,1.);
#4459=VECTOR('',#16317,1.);
#4460=VECTOR('',#16320,1.);
#4461=VECTOR('',#16321,1.);
#4462=VECTOR('',#16322,1.);
#4463=VECTOR('',#16325,1.);
#4464=VECTOR('',#16326,1.);
#4465=VECTOR('',#16327,1.);
#4466=VECTOR('',#16330,1.);
#4467=VECTOR('',#16331,1.);
#4468=VECTOR('',#16332,1.);
#4469=VECTOR('',#16335,1.);
#4470=VECTOR('',#16336,1.);
#4471=VECTOR('',#16337,1.);
#4472=VECTOR('',#16340,1.);
#4473=VECTOR('',#16341,1.);
#4474=VECTOR('',#16342,1.);
#4475=VECTOR('',#16345,1.);
#4476=VECTOR('',#16346,1.);
#4477=VECTOR('',#16347,1.);
#4478=VECTOR('',#16350,1.);
#4479=VECTOR('',#16351,1.);
#4480=VECTOR('',#16352,1.);
#4481=VECTOR('',#16355,1.);
#4482=VECTOR('',#16356,1.);
#4483=VECTOR('',#16357,1.);
#4484=VECTOR('',#16360,1.);
#4485=VECTOR('',#16361,1.);
#4486=VECTOR('',#16384,1.070235);
#4487=VECTOR('',#16391,0.6);
#4488=VECTOR('',#16396,0.63);
#4489=VECTOR('',#16405,1.070235);
#4490=VECTOR('',#16412,0.63);
#4491=VECTOR('',#16431,1.129765);
#4492=VECTOR('',#16442,1.57);
#4493=VECTOR('',#16447,1.6);
#4494=VECTOR('',#16452,1.57);
#4495=VECTOR('',#16457,1.129765);
#4496=VECTOR('',#16504,1.123812);
#4497=VECTOR('',#16573,1.076188);
#4498=VECTOR('',#16602,1.119765);
#4499=VECTOR('',#16609,1.085235);
#4500=VECTOR('',#16620,1.119765);
#4501=VECTOR('',#16627,1.085235);
#4502=VECTOR('',#16648,0.325);
#4503=VECTOR('',#16653,0.35);
#4504=VECTOR('',#16658,0.335);
#4505=VECTOR('',#16667,0.21);
#4506=VECTOR('',#16672,0.2);
#4507=VECTOR('',#16677,0.18);
#4508=VECTOR('',#16682,1.);
#4509=VECTOR('',#16683,1.);
#4510=VECTOR('',#16684,1.);
#4511=VECTOR('',#16685,1.);
#4512=VECTOR('',#16688,1.);
#4513=VECTOR('',#16689,1.);
#4514=VECTOR('',#16690,1.);
#4515=VECTOR('',#16693,1.);
#4516=VECTOR('',#16694,1.);
#4517=VECTOR('',#16695,1.);
#4518=VECTOR('',#16698,1.);
#4519=VECTOR('',#16699,1.);
#4520=VECTOR('',#16700,1.);
#4521=VECTOR('',#16703,1.);
#4522=VECTOR('',#16704,1.);
#4523=VECTOR('',#16705,1.);
#4524=VECTOR('',#16708,1.);
#4525=VECTOR('',#16709,1.);
#4526=VECTOR('',#16722,0.21);
#4527=VECTOR('',#16729,0.21);
#4528=VECTOR('',#16736,0.210000000000001);
#4529=VECTOR('',#16743,0.210000000000001);
#4530=VECTOR('',#16750,0.164999999999999);
#4531=VECTOR('',#16755,1.);
#4532=VECTOR('',#16756,1.);
#4533=VECTOR('',#16757,1.);
#4534=VECTOR('',#16758,1.);
#4535=VECTOR('',#16761,1.);
#4536=VECTOR('',#16762,1.);
#4537=VECTOR('',#16763,1.);
#4538=VECTOR('',#16766,1.);
#4539=VECTOR('',#16767,1.);
#4540=VECTOR('',#16768,1.);
#4541=VECTOR('',#16771,1.);
#4542=VECTOR('',#16772,1.);
#4543=VECTOR('',#16779,0.275);
#4544=VECTOR('',#16786,0.275);
#4545=VECTOR('',#16793,0.275);
#4546=VECTOR('',#16800,0.275);
#4547=VECTOR('',#16805,1.);
#4548=VECTOR('',#16808,1.);
#4549=VECTOR('',#16813,1.);
#4550=VECTOR('',#16814,1.);
#4551=VECTOR('',#16815,1.);
#4552=VECTOR('',#16816,1.);
#4553=VECTOR('',#16817,1.);
#4554=VECTOR('',#16820,1.);
#4555=VECTOR('',#16821,1.);
#4556=VECTOR('',#16824,1.);
#4557=VECTOR('',#16825,1.);
#4558=VECTOR('',#16828,1.);
#4559=VECTOR('',#16829,1.);
#4560=VECTOR('',#16832,1.);
#4561=VECTOR('',#16833,1.);
#4562=VECTOR('',#16836,1.);
#4563=VECTOR('',#16843,1.);
#4564=VECTOR('',#16844,1.);
#4565=VECTOR('',#16845,1.);
#4566=VECTOR('',#16846,1.);
#4567=VECTOR('',#16849,1.);
#4568=VECTOR('',#16850,1.);
#4569=VECTOR('',#16851,1.);
#4570=VECTOR('',#16854,1.);
#4571=VECTOR('',#16855,1.);
#4572=VECTOR('',#16856,1.);
#4573=VECTOR('',#16859,1.);
#4574=VECTOR('',#16860,1.);
#4575=VECTOR('',#16869,0.25);
#4576=VECTOR('',#16874,0.165);
#4577=VECTOR('',#16883,0.165);
#4578=VECTOR('',#16892,0.164999999999999);
#4579=VECTOR('',#16901,0.165);
#4580=VECTOR('',#16908,1.);
#4581=VECTOR('',#16911,1.);
#4582=VECTOR('',#16920,1.);
#4583=VECTOR('',#16923,1.);
#4584=VECTOR('',#16932,1.);
#4585=VECTOR('',#16935,1.);
#4586=VECTOR('',#16944,1.);
#4587=VECTOR('',#16947,1.);
#4588=VECTOR('',#16958,0.275);
#4589=VECTOR('',#16985,0.275);
#4590=VECTOR('',#16990,0.275);
#4591=VECTOR('',#16995,0.275);
#4592=VECTOR('',#17000,3.);
#4593=VECTOR('',#17005,2.35);
#4594=VECTOR('',#17014,3.5);
#4595=VECTOR('',#17019,1.6);
#4596=VECTOR('',#17032,1.7);
#4597=VECTOR('',#17039,2.34);
#4598=VECTOR('',#17052,0.225);
#4599=VECTOR('',#17059,0.225);
#4600=VECTOR('',#17066,0.225);
#4601=VECTOR('',#17073,0.225000000000001);
#4602=VECTOR('',#17080,1.7);
#4603=VECTOR('',#17087,3.);
#4604=VECTOR('',#17100,1.);
#4605=VECTOR('',#17105,1.);
#4606=VECTOR('',#17108,0.21);
#4607=VECTOR('',#17113,1.);
#4608=VECTOR('',#17116,1.);
#4609=VECTOR('',#17121,1.);
#4610=VECTOR('',#17124,0.21);
#4611=VECTOR('',#17129,1.);
#4612=VECTOR('',#17132,1.);
#4613=VECTOR('',#17137,1.);
#4614=VECTOR('',#17140,0.21);
#4615=VECTOR('',#17145,1.);
#4616=VECTOR('',#17148,1.);
#4617=VECTOR('',#17153,1.);
#4618=VECTOR('',#17156,0.21);
#4619=VECTOR('',#17161,1.);
#4620=VECTOR('',#17164,1.);
#4621=VECTOR('',#17165,1.);
#4622=VECTOR('',#17166,1.);
#4623=VECTOR('',#17167,1.);
#4624=VECTOR('',#17168,1.);
#4625=VECTOR('',#17169,1.);
#4626=VECTOR('',#17172,1.);
#4627=VECTOR('',#17173,1.);
#4628=VECTOR('',#17174,1.);
#4629=VECTOR('',#17175,1.);
#4630=VECTOR('',#17176,1.);
#4631=VECTOR('',#17177,1.);
#4632=VECTOR('',#17180,1.);
#4633=VECTOR('',#17181,1.);
#4634=VECTOR('',#17182,1.);
#4635=VECTOR('',#17183,1.);
#4636=VECTOR('',#17184,1.);
#4637=VECTOR('',#17185,1.);
#4638=VECTOR('',#17186,1.);
#4639=VECTOR('',#17187,1.);
#4640=VECTOR('',#17188,1.);
#4641=VECTOR('',#17189,1.);
#4642=VECTOR('',#17192,1.);
#4643=VECTOR('',#17193,1.);
#4644=VECTOR('',#17196,1.);
#4645=VECTOR('',#17197,1.);
#4646=VECTOR('',#17200,1.);
#4647=VECTOR('',#17201,1.);
#4648=VECTOR('',#17204,1.);
#4649=VECTOR('',#17205,1.);
#4650=VECTOR('',#17208,1.);
#4651=VECTOR('',#17211,1.);
#4652=VECTOR('',#17212,1.);
#4653=VECTOR('',#17215,1.);
#4654=VECTOR('',#17216,1.);
#4655=VECTOR('',#17219,1.);
#4656=VECTOR('',#17220,1.);
#4657=VECTOR('',#17223,1.);
#4658=VECTOR('',#17224,1.);
#4659=VECTOR('',#17227,1.);
#4660=VECTOR('',#17234,1.);
#4661=VECTOR('',#17235,1.);
#4662=VECTOR('',#17236,1.);
#4663=VECTOR('',#17237,1.);
#4664=VECTOR('',#17240,1.);
#4665=VECTOR('',#17241,1.);
#4666=VECTOR('',#17242,1.);
#4667=VECTOR('',#17245,1.);
#4668=VECTOR('',#17246,1.);
#4669=VECTOR('',#17247,1.);
#4670=VECTOR('',#17250,1.);
#4671=VECTOR('',#17251,1.);
#4672=VECTOR('',#17252,1.);
#4673=VECTOR('',#17255,1.);
#4674=VECTOR('',#17256,1.);
#4675=VECTOR('',#17257,1.);
#4676=VECTOR('',#17260,1.);
#4677=VECTOR('',#17261,1.);
#4678=VECTOR('',#17262,1.);
#4679=VECTOR('',#17265,1.);
#4680=VECTOR('',#17266,1.);
#4681=VECTOR('',#17267,1.);
#4682=VECTOR('',#17270,1.);
#4683=VECTOR('',#17271,1.);
#4684=VECTOR('',#17280,1.);
#4685=VECTOR('',#17281,1.);
#4686=VECTOR('',#17282,1.);
#4687=VECTOR('',#17283,1.);
#4688=VECTOR('',#17286,1.);
#4689=VECTOR('',#17287,1.);
#4690=VECTOR('',#17288,1.);
#4691=VECTOR('',#17291,1.);
#4692=VECTOR('',#17292,1.);
#4693=VECTOR('',#17293,1.);
#4694=VECTOR('',#17296,1.);
#4695=VECTOR('',#17297,1.);
#4696=VECTOR('',#17298,1.);
#4697=VECTOR('',#17301,1.);
#4698=VECTOR('',#17302,1.);
#4699=VECTOR('',#17303,1.);
#4700=VECTOR('',#17306,1.);
#4701=VECTOR('',#17307,1.);
#4702=VECTOR('',#17308,1.);
#4703=VECTOR('',#17311,1.);
#4704=VECTOR('',#17312,1.);
#4705=VECTOR('',#17313,1.);
#4706=VECTOR('',#17316,1.);
#4707=VECTOR('',#17317,1.);
#4708=VECTOR('',#17332,1.);
#4709=VECTOR('',#17333,1.);
#4710=VECTOR('',#17334,1.);
#4711=VECTOR('',#17335,1.);
#4712=VECTOR('',#17338,1.);
#4713=VECTOR('',#17339,1.);
#4714=VECTOR('',#17340,1.);
#4715=VECTOR('',#17343,1.);
#4716=VECTOR('',#17344,1.);
#4717=VECTOR('',#17345,1.);
#4718=VECTOR('',#17348,1.);
#4719=VECTOR('',#17349,1.);
#4720=VECTOR('',#17350,1.);
#4721=VECTOR('',#17353,1.);
#4722=VECTOR('',#17354,1.);
#4723=VECTOR('',#17355,1.);
#4724=VECTOR('',#17358,1.);
#4725=VECTOR('',#17359,1.);
#4726=VECTOR('',#17370,0.185);
#4727=VECTOR('',#17375,0.2);
#4728=VECTOR('',#17380,0.1625);
#4729=VECTOR('',#17387,1.);
#4730=VECTOR('',#17388,1.);
#4731=VECTOR('',#17389,1.);
#4732=VECTOR('',#17390,1.);
#4733=VECTOR('',#17393,1.);
#4734=VECTOR('',#17394,1.);
#4735=VECTOR('',#17395,1.);
#4736=VECTOR('',#17398,1.);
#4737=VECTOR('',#17399,1.);
#4738=VECTOR('',#17400,1.);
#4739=VECTOR('',#17403,1.);
#4740=VECTOR('',#17404,1.);
#4741=VECTOR('',#17405,1.);
#4742=VECTOR('',#17408,1.);
#4743=VECTOR('',#17409,1.);
#4744=VECTOR('',#17410,1.);
#4745=VECTOR('',#17413,1.);
#4746=VECTOR('',#17414,1.);
#4747=VECTOR('',#17431,0.4);
#4748=VECTOR('',#17436,0.425);
#4749=VECTOR('',#17441,0.41);
#4750=VECTOR('',#17450,0.26);
#4751=VECTOR('',#17453,0.25);
#4752=VECTOR('',#17472,1.63531);
#4753=VECTOR('',#17479,1.);
#4754=VECTOR('',#17484,1.05);
#4755=VECTOR('',#17493,1.63531);
#4756=VECTOR('',#17500,1.05);
#4757=VECTOR('',#17519,1.71469);
#4758=VECTOR('',#17530,2.3);
#4759=VECTOR('',#17535,2.35);
#4760=VECTOR('',#17540,2.3);
#4761=VECTOR('',#17545,1.71469);
#4762=VECTOR('',#17596,1.706752);
#4763=VECTOR('',#17673,1.643248);
#4764=VECTOR('',#17702,1.70469);
#4765=VECTOR('',#17709,1.65031);
#4766=VECTOR('',#17720,1.70469);
#4767=VECTOR('',#17727,1.65031);
#4768=VECTOR('',#17746,0.165);
#4769=VECTOR('',#17753,1.);
#4770=VECTOR('',#17754,1.);
#4771=VECTOR('',#17755,1.);
#4772=VECTOR('',#17756,1.);
#4773=VECTOR('',#17761,1.);
#4774=VECTOR('',#17762,1.);
#4775=VECTOR('',#17765,1.);
#4776=VECTOR('',#17766,1.);
#4777=VECTOR('',#17769,1.);
#4778=VECTOR('',#17770,1.);
#4779=VECTOR('',#17789,0.8);
#4780=VECTOR('',#17792,0.6);
#4781=VECTOR('',#17799,0.6);
#4782=VECTOR('',#17810,0.605);
#4783=VECTOR('',#17817,0.8);
#4784=VECTOR('',#17830,0.605);
#4785=VECTOR('',#17837,0.8);
#4786=VECTOR('',#17850,0.605);
#4787=VECTOR('',#17857,0.8);
#4788=VECTOR('',#17868,1.);
#4789=VECTOR('',#17873,1.);
#4790=VECTOR('',#17878,1.);
#4791=VECTOR('',#17885,0.165);
#4792=VECTOR('',#17888,1.);
#4793=VECTOR('',#17893,0.605);
#4794=VECTOR('',#17900,1.2);
#4795=VECTOR('',#17911,1.);
#4796=VECTOR('',#17912,1.);
#4797=VECTOR('',#17913,1.);
#4798=VECTOR('',#17914,1.);
#4799=VECTOR('',#17917,1.);
#4800=VECTOR('',#17918,1.);
#4801=VECTOR('',#17919,1.);
#4802=VECTOR('',#17922,1.);
#4803=VECTOR('',#17923,1.);
#4804=VECTOR('',#17924,1.);
#4805=VECTOR('',#17927,1.);
#4806=VECTOR('',#17928,1.);
#4807=VECTOR('',#17939,0.225);
#4808=VECTOR('',#17946,0.9);
#4809=VECTOR('',#17957,1.);
#4810=VECTOR('',#17958,1.);
#4811=VECTOR('',#17959,1.);
#4812=VECTOR('',#17960,1.);
#4813=VECTOR('',#17963,1.);
#4814=VECTOR('',#17964,1.);
#4815=VECTOR('',#17965,1.);
#4816=VECTOR('',#17968,1.);
#4817=VECTOR('',#17969,1.);
#4818=VECTOR('',#17970,1.);
#4819=VECTOR('',#17975,1.);
#4820=VECTOR('',#17978,1.);
#4821=VECTOR('',#17981,1.);
#4822=VECTOR('',#17984,1.);
#4823=VECTOR('',#17987,1.);
#4824=VECTOR('',#17990,1.);
#4825=VECTOR('',#17993,1.);
#4826=VECTOR('',#17996,1.);
#4827=VECTOR('',#17999,1.);
#4828=VECTOR('',#18002,1.);
#4829=VECTOR('',#18005,1.);
#4830=VECTOR('',#18008,1.);
#4831=VECTOR('',#18011,1.);
#4832=VECTOR('',#18014,1.);
#4833=VECTOR('',#18017,1.);
#4834=VECTOR('',#18020,1.);
#4835=VECTOR('',#18023,1.);
#4836=VECTOR('',#18026,1.);
#4837=VECTOR('',#18029,1.);
#4838=VECTOR('',#18032,1.);
#4839=VECTOR('',#18043,1.4);
#4840=VECTOR('',#18048,1.);
#4841=VECTOR('',#18049,1.);
#4842=VECTOR('',#18052,1.);
#4843=VECTOR('',#18053,1.);
#4844=VECTOR('',#18054,1.);
#4845=VECTOR('',#18059,1.);
#4846=VECTOR('',#18060,1.);
#4847=VECTOR('',#18063,1.);
#4848=VECTOR('',#18064,1.);
#4849=VECTOR('',#18065,1.);
#4850=VECTOR('',#18070,1.);
#4851=VECTOR('',#18071,1.);
#4852=VECTOR('',#18074,1.);
#4853=VECTOR('',#18075,1.);
#4854=VECTOR('',#18076,1.);
#4855=VECTOR('',#18081,1.);
#4856=VECTOR('',#18082,1.);
#4857=VECTOR('',#18085,1.);
#4858=VECTOR('',#18086,1.);
#4859=VECTOR('',#18087,1.);
#4860=VECTOR('',#18092,1.);
#4861=VECTOR('',#18093,1.);
#4862=VECTOR('',#18096,1.);
#4863=VECTOR('',#18097,1.);
#4864=VECTOR('',#18098,1.);
#4865=VECTOR('',#18103,1.);
#4866=VECTOR('',#18104,1.);
#4867=VECTOR('',#18107,1.);
#4868=VECTOR('',#18108,1.);
#4869=VECTOR('',#18109,1.);
#4870=VECTOR('',#18114,1.);
#4871=VECTOR('',#18115,1.);
#4872=VECTOR('',#18118,1.);
#4873=VECTOR('',#18119,1.);
#4874=VECTOR('',#18120,1.);
#4875=VECTOR('',#18125,1.);
#4876=VECTOR('',#18126,1.);
#4877=VECTOR('',#18129,1.);
#4878=VECTOR('',#18130,1.);
#4879=VECTOR('',#18131,1.);
#4880=VECTOR('',#18136,1.);
#4881=VECTOR('',#18137,1.);
#4882=VECTOR('',#18140,1.);
#4883=VECTOR('',#18141,1.);
#4884=VECTOR('',#18142,1.);
#4885=VECTOR('',#18147,1.);
#4886=VECTOR('',#18148,1.);
#4887=VECTOR('',#18151,1.);
#4888=VECTOR('',#18152,1.);
#4889=VECTOR('',#18153,1.);
#4890=VECTOR('',#18158,1.);
#4891=VECTOR('',#18159,1.);
#4892=VECTOR('',#18162,1.);
#4893=VECTOR('',#18163,1.);
#4894=VECTOR('',#18164,1.);
#4895=VECTOR('',#18169,1.);
#4896=VECTOR('',#18170,1.);
#4897=VECTOR('',#18173,1.);
#4898=VECTOR('',#18174,1.);
#4899=VECTOR('',#18175,1.);
#4900=VECTOR('',#18180,1.);
#4901=VECTOR('',#18181,1.);
#4902=VECTOR('',#18184,1.);
#4903=VECTOR('',#18185,1.);
#4904=VECTOR('',#18186,1.);
#4905=VECTOR('',#18191,1.);
#4906=VECTOR('',#18192,1.);
#4907=VECTOR('',#18195,1.);
#4908=VECTOR('',#18196,1.);
#4909=VECTOR('',#18197,1.);
#4910=VECTOR('',#18202,1.);
#4911=VECTOR('',#18203,1.);
#4912=VECTOR('',#18206,1.);
#4913=VECTOR('',#18207,1.);
#4914=VECTOR('',#18208,1.);
#4915=VECTOR('',#18213,1.);
#4916=VECTOR('',#18214,1.);
#4917=VECTOR('',#18217,1.);
#4918=VECTOR('',#18218,1.);
#4919=VECTOR('',#18219,1.);
#4920=VECTOR('',#18224,1.);
#4921=VECTOR('',#18225,1.);
#4922=VECTOR('',#18228,1.);
#4923=VECTOR('',#18229,1.);
#4924=VECTOR('',#18230,1.);
#4925=VECTOR('',#18235,1.);
#4926=VECTOR('',#18236,1.);
#4927=VECTOR('',#18239,1.);
#4928=VECTOR('',#18240,1.);
#4929=VECTOR('',#18241,1.);
#4930=VECTOR('',#18246,1.);
#4931=VECTOR('',#18247,1.);
#4932=VECTOR('',#18250,1.);
#4933=VECTOR('',#18251,1.);
#4934=VECTOR('',#18252,1.);
#4935=VECTOR('',#18257,1.);
#4936=VECTOR('',#18258,1.);
#4937=VECTOR('',#18261,1.);
#4938=VECTOR('',#18262,1.);
#4939=VECTOR('',#18263,1.);
#4940=VECTOR('',#18278,0.165);
#4941=VECTOR('',#18285,1.);
#4942=VECTOR('',#18286,1.);
#4943=VECTOR('',#18287,1.);
#4944=VECTOR('',#18288,1.);
#4945=VECTOR('',#18293,1.);
#4946=VECTOR('',#18294,1.);
#4947=VECTOR('',#18297,1.);
#4948=VECTOR('',#18298,1.);
#4949=VECTOR('',#18301,1.);
#4950=VECTOR('',#18302,1.);
#4951=VECTOR('',#18321,1.2);
#4952=VECTOR('',#18324,1.);
#4953=VECTOR('',#18331,1.);
#4954=VECTOR('',#18342,1.005);
#4955=VECTOR('',#18349,1.2);
#4956=VECTOR('',#18362,1.005);
#4957=VECTOR('',#18369,1.2);
#4958=VECTOR('',#18380,0.165);
#4959=VECTOR('',#18385,1.005);
#4960=VECTOR('',#18392,1.5);
#4961=VECTOR('',#18403,1.);
#4962=VECTOR('',#18404,1.);
#4963=VECTOR('',#18405,1.);
#4964=VECTOR('',#18406,1.);
#4965=VECTOR('',#18409,1.);
#4966=VECTOR('',#18410,1.);
#4967=VECTOR('',#18411,1.);
#4968=VECTOR('',#18414,1.);
#4969=VECTOR('',#18415,1.);
#4970=VECTOR('',#18416,1.);
#4971=VECTOR('',#18419,1.);
#4972=VECTOR('',#18420,1.);
#4973=VECTOR('',#18431,0.225);
#4974=VECTOR('',#18438,1.3);
#4975=VECTOR('',#18453,1.);
#4976=VECTOR('',#18454,1.);
#4977=VECTOR('',#18455,1.);
#4978=VECTOR('',#18456,1.);
#4979=VECTOR('',#18459,1.);
#4980=VECTOR('',#18460,1.);
#4981=VECTOR('',#18461,1.);
#4982=VECTOR('',#18464,1.);
#4983=VECTOR('',#18465,1.);
#4984=VECTOR('',#18466,1.);
#4985=VECTOR('',#18469,1.);
#4986=VECTOR('',#18470,1.);
#4987=VECTOR('',#18471,1.);
#4988=VECTOR('',#18474,1.);
#4989=VECTOR('',#18475,1.);
#4990=VECTOR('',#18476,1.);
#4991=VECTOR('',#18479,1.);
#4992=VECTOR('',#18480,1.);
#4993=VECTOR('',#18491,0.185);
#4994=VECTOR('',#18494,0.2);
#4995=VECTOR('',#18499,1.);
#4996=VECTOR('',#18500,1.);
#4997=VECTOR('',#18501,1.);
#4998=VECTOR('',#18502,1.);
#4999=VECTOR('',#18505,1.);
#5000=VECTOR('',#18506,1.);
#5001=VECTOR('',#18507,1.);
#5002=VECTOR('',#18510,1.);
#5003=VECTOR('',#18511,1.);
#5004=VECTOR('',#18512,1.);
#5005=VECTOR('',#18517,1.);
#5006=VECTOR('',#18520,1.);
#5007=VECTOR('',#18523,1.);
#5008=VECTOR('',#18526,1.);
#5009=VECTOR('',#18529,1.);
#5010=VECTOR('',#18532,1.);
#5011=VECTOR('',#18535,1.);
#5012=VECTOR('',#18538,1.);
#5013=VECTOR('',#18541,1.);
#5014=VECTOR('',#18544,1.);
#5015=VECTOR('',#18547,1.);
#5016=VECTOR('',#18550,1.);
#5017=VECTOR('',#18553,1.);
#5018=VECTOR('',#18556,1.);
#5019=VECTOR('',#18559,1.);
#5020=VECTOR('',#18562,1.);
#5021=VECTOR('',#18565,1.);
#5022=VECTOR('',#18568,1.);
#5023=VECTOR('',#18571,1.);
#5024=VECTOR('',#18574,1.);
#5025=VECTOR('',#18577,1.);
#5026=VECTOR('',#18580,1.);
#5027=VECTOR('',#18583,1.);
#5028=VECTOR('',#18586,1.);
#5029=VECTOR('',#18589,1.);
#5030=VECTOR('',#18592,1.);
#5031=VECTOR('',#18595,1.);
#5032=VECTOR('',#18598,1.);
#5033=VECTOR('',#18601,1.);
#5034=VECTOR('',#18604,1.);
#5035=VECTOR('',#18607,1.);
#5036=VECTOR('',#18610,1.);
#5037=VECTOR('',#18613,1.);
#5038=VECTOR('',#18616,1.);
#5039=VECTOR('',#18619,1.);
#5040=VECTOR('',#18622,1.);
#5041=VECTOR('',#18625,1.);
#5042=VECTOR('',#18628,1.);
#5043=VECTOR('',#18631,1.);
#5044=VECTOR('',#18634,1.);
#5045=VECTOR('',#18645,2.);
#5046=VECTOR('',#18650,1.);
#5047=VECTOR('',#18651,1.);
#5048=VECTOR('',#18654,1.);
#5049=VECTOR('',#18659,1.);
#5050=VECTOR('',#18660,1.);
#5051=VECTOR('',#18663,1.);
#5052=VECTOR('',#18668,1.);
#5053=VECTOR('',#18669,1.);
#5054=VECTOR('',#18672,1.);
#5055=VECTOR('',#18677,1.);
#5056=VECTOR('',#18678,1.);
#5057=VECTOR('',#18681,1.);
#5058=VECTOR('',#18686,1.);
#5059=VECTOR('',#18687,1.);
#5060=VECTOR('',#18690,1.);
#5061=VECTOR('',#18695,1.);
#5062=VECTOR('',#18696,1.);
#5063=VECTOR('',#18699,1.);
#5064=VECTOR('',#18704,1.);
#5065=VECTOR('',#18705,1.);
#5066=VECTOR('',#18708,1.);
#5067=VECTOR('',#18713,1.);
#5068=VECTOR('',#18714,1.);
#5069=VECTOR('',#18717,1.);
#5070=VECTOR('',#18722,1.);
#5071=VECTOR('',#18723,1.);
#5072=VECTOR('',#18726,1.);
#5073=VECTOR('',#18731,1.);
#5074=VECTOR('',#18732,1.);
#5075=VECTOR('',#18735,1.);
#5076=VECTOR('',#18740,1.);
#5077=VECTOR('',#18741,1.);
#5078=VECTOR('',#18744,1.);
#5079=VECTOR('',#18749,1.);
#5080=VECTOR('',#18750,1.);
#5081=VECTOR('',#18753,1.);
#5082=VECTOR('',#18758,1.);
#5083=VECTOR('',#18759,1.);
#5084=VECTOR('',#18762,1.);
#5085=VECTOR('',#18767,1.);
#5086=VECTOR('',#18768,1.);
#5087=VECTOR('',#18771,1.);
#5088=VECTOR('',#18776,1.);
#5089=VECTOR('',#18777,1.);
#5090=VECTOR('',#18780,1.);
#5091=VECTOR('',#18785,1.);
#5092=VECTOR('',#18786,1.);
#5093=VECTOR('',#18789,1.);
#5094=VECTOR('',#18794,1.);
#5095=VECTOR('',#18795,1.);
#5096=VECTOR('',#18798,1.);
#5097=VECTOR('',#18803,1.);
#5098=VECTOR('',#18804,1.);
#5099=VECTOR('',#18807,1.);
#5100=VECTOR('',#18812,1.);
#5101=VECTOR('',#18813,1.);
#5102=VECTOR('',#18816,1.);
#5103=VECTOR('',#18821,1.);
#5104=VECTOR('',#18822,1.);
#5105=VECTOR('',#18825,1.);
#5106=VECTOR('',#18830,1.);
#5107=VECTOR('',#18831,1.);
#5108=VECTOR('',#18834,1.);
#5109=VECTOR('',#18839,1.);
#5110=VECTOR('',#18840,1.);
#5111=VECTOR('',#18843,1.);
#5112=VECTOR('',#18848,1.);
#5113=VECTOR('',#18849,1.);
#5114=VECTOR('',#18852,1.);
#5115=VECTOR('',#18857,1.);
#5116=VECTOR('',#18858,1.);
#5117=VECTOR('',#18861,1.);
#5118=VECTOR('',#18866,1.);
#5119=VECTOR('',#18867,1.);
#5120=VECTOR('',#18870,1.);
#5121=VECTOR('',#18875,1.);
#5122=VECTOR('',#18876,1.);
#5123=VECTOR('',#18879,1.);
#5124=VECTOR('',#18884,1.);
#5125=VECTOR('',#18885,1.);
#5126=VECTOR('',#18888,1.);
#5127=VECTOR('',#18893,1.);
#5128=VECTOR('',#18894,1.);
#5129=VECTOR('',#18897,1.);
#5130=VECTOR('',#18902,1.);
#5131=VECTOR('',#18903,1.);
#5132=VECTOR('',#18906,1.);
#5133=VECTOR('',#18911,1.);
#5134=VECTOR('',#18912,1.);
#5135=VECTOR('',#18915,1.);
#5136=VECTOR('',#18920,1.);
#5137=VECTOR('',#18921,1.);
#5138=VECTOR('',#18924,1.);
#5139=VECTOR('',#18929,1.);
#5140=VECTOR('',#18930,1.);
#5141=VECTOR('',#18933,1.);
#5142=VECTOR('',#18938,1.);
#5143=VECTOR('',#18939,1.);
#5144=VECTOR('',#18942,1.);
#5145=VECTOR('',#18947,1.);
#5146=VECTOR('',#18948,1.);
#5147=VECTOR('',#18951,1.);
#5148=VECTOR('',#18956,1.);
#5149=VECTOR('',#18957,1.);
#5150=VECTOR('',#18960,1.);
#5151=VECTOR('',#18965,1.);
#5152=VECTOR('',#18966,1.);
#5153=VECTOR('',#18969,1.);
#5154=VECTOR('',#18974,1.);
#5155=VECTOR('',#18975,1.);
#5156=VECTOR('',#18978,1.);
#5157=VECTOR('',#18983,1.);
#5158=VECTOR('',#18984,1.);
#5159=VECTOR('',#18987,1.);
#5160=VECTOR('',#18992,1.);
#5161=VECTOR('',#18995,1.);
#5162=VECTOR('',#18996,1.);
#5163=VECTOR('',#19001,1.);
#5164=VECTOR('',#19002,1.);
#5165=VECTOR('',#19005,1.);
#5166=VECTOR('',#19016,1.);
#5167=VECTOR('',#19017,1.);
#5168=VECTOR('',#19018,1.);
#5169=VECTOR('',#19019,1.);
#5170=VECTOR('',#19022,1.);
#5171=VECTOR('',#19023,1.);
#5172=VECTOR('',#19024,1.);
#5173=VECTOR('',#19027,1.);
#5174=VECTOR('',#19028,1.);
#5175=VECTOR('',#19029,1.);
#5176=VECTOR('',#19032,1.);
#5177=VECTOR('',#19033,1.);
#5178=VECTOR('',#19034,1.);
#5179=VECTOR('',#19037,1.);
#5180=VECTOR('',#19038,1.);
#5181=VECTOR('',#19039,1.);
#5182=VECTOR('',#19042,1.);
#5183=VECTOR('',#19043,1.);
#5184=VECTOR('',#19060,0.325);
#5185=VECTOR('',#19065,0.35);
#5186=VECTOR('',#19070,0.335);
#5187=VECTOR('',#19079,0.21);
#5188=VECTOR('',#19082,0.2);
#5189=CIRCLE('',#14199,0.164999999999999);
#5190=CIRCLE('',#14200,0.164999999999999);
#5191=CIRCLE('',#14202,0.164999999999999);
#5192=CIRCLE('',#14203,0.164999999999999);
#5193=CIRCLE('',#14205,0.164999999999999);
#5194=CIRCLE('',#14206,0.164999999999999);
#5195=CIRCLE('',#14208,0.164999999999999);
#5196=CIRCLE('',#14209,0.164999999999999);
#5197=CIRCLE('',#14211,0.21);
#5198=CIRCLE('',#14212,0.21);
#5199=CIRCLE('',#14214,0.21);
#5200=CIRCLE('',#14215,0.21);
#5201=CIRCLE('',#14217,0.21);
#5202=CIRCLE('',#14218,0.21);
#5203=CIRCLE('',#14220,0.21);
#5204=CIRCLE('',#14221,0.21);
#5205=CIRCLE('',#14223,0.164999999999999);
#5206=CIRCLE('',#14224,0.164999999999999);
#5207=CIRCLE('',#14226,0.164999999999999);
#5208=CIRCLE('',#14227,0.164999999999999);
#5209=CIRCLE('',#14229,0.165);
#5210=CIRCLE('',#14230,0.165);
#5211=CIRCLE('',#14232,0.165);
#5212=CIRCLE('',#14233,0.165);
#5213=CIRCLE('',#14257,0.165);
#5214=CIRCLE('',#14258,0.165);
#5215=CIRCLE('',#14261,0.165);
#5216=CIRCLE('',#14262,0.165);
#5217=CIRCLE('',#14265,0.165);
#5218=CIRCLE('',#14266,0.165);
#5219=CIRCLE('',#14269,0.165);
#5220=CIRCLE('',#14270,0.165);
#5221=CIRCLE('',#14273,2.2);
#5222=CIRCLE('',#14274,0.525);
#5223=CIRCLE('',#14276,0.525);
#5224=CIRCLE('',#14278,0.525);
#5225=CIRCLE('',#14279,0.525);
#5226=CIRCLE('',#14281,2.2);
#5227=CIRCLE('',#14283,0.525);
#5228=CIRCLE('',#14284,0.525);
#5229=CIRCLE('',#14286,2.2);
#5230=CIRCLE('',#14288,0.525);
#5231=CIRCLE('',#14289,0.525);
#5232=CIRCLE('',#14291,2.2);
#5233=CIRCLE('',#14293,2.2);
#5234=CIRCLE('',#14294,2.2);
#5235=CIRCLE('',#14295,2.2);
#5236=CIRCLE('',#14296,2.2);
#5237=CIRCLE('',#14297,2.2);
#5238=CIRCLE('',#14298,2.2);
#5239=CIRCLE('',#14300,3.);
#5240=CIRCLE('',#14301,0.275);
#5241=CIRCLE('',#14302,0.275);
#5242=CIRCLE('',#14303,0.275);
#5243=CIRCLE('',#14304,0.275);
#5244=CIRCLE('',#14306,0.275);
#5245=CIRCLE('',#14308,0.275);
#5246=CIRCLE('',#14310,0.275);
#5247=CIRCLE('',#14312,0.275);
#5248=CIRCLE('',#14314,1.6);
#5249=CIRCLE('',#14315,1.6);
#5250=CIRCLE('',#14317,1.3);
#5251=CIRCLE('',#14319,3.);
#5252=CIRCLE('',#14321,1.3);
#5253=CIRCLE('',#14326,1.1);
#5254=CIRCLE('',#14327,1.1);
#5255=CIRCLE('',#14329,1.59);
#5256=CIRCLE('',#14330,1.59);
#5257=CIRCLE('',#14335,0.225);
#5258=CIRCLE('',#14336,0.225);
#5259=CIRCLE('',#14338,0.225);
#5260=CIRCLE('',#14339,0.225);
#5261=CIRCLE('',#14341,0.225);
#5262=CIRCLE('',#14342,0.225);
#5263=CIRCLE('',#14344,0.225);
#5264=CIRCLE('',#14345,0.225);
#5265=CIRCLE('',#14347,2.2);
#5266=CIRCLE('',#14348,2.2);
#5267=CIRCLE('',#14349,2.2);
#5268=CIRCLE('',#14350,2.2);
#5269=CIRCLE('',#14351,1.59);
#5270=CIRCLE('',#14353,2.2);
#5271=CIRCLE('',#14355,2.2);
#5272=CIRCLE('',#14357,2.2);
#5273=CIRCLE('',#14359,2.2);
#5274=CIRCLE('',#14361,1.59);
#5275=CIRCLE('',#14363,1.1);
#5276=CIRCLE('',#14365,1.1);
#5277=CIRCLE('',#14369,0.225);
#5278=CIRCLE('',#14370,0.225);
#5279=CIRCLE('',#14372,0.225);
#5280=CIRCLE('',#14373,0.225);
#5281=CIRCLE('',#14375,0.225);
#5282=CIRCLE('',#14376,0.225);
#5283=CIRCLE('',#14378,0.225);
#5284=CIRCLE('',#14379,0.225);
#5285=CIRCLE('',#14381,0.6);
#5286=CIRCLE('',#14382,0.6);
#5287=CIRCLE('',#14385,1.5);
#5288=CIRCLE('',#14386,1.5);
#5289=CIRCLE('',#14391,0.164999999999999);
#5290=CIRCLE('',#14393,0.164999999999999);
#5291=CIRCLE('',#14394,0.164999999999999);
#5292=CIRCLE('',#14397,1.);
#5293=CIRCLE('',#14398,1.);
#5294=CIRCLE('',#14399,1.);
#5295=CIRCLE('',#14400,1.);
#5296=CIRCLE('',#14401,1.);
#5297=CIRCLE('',#14402,1.);
#5298=CIRCLE('',#14403,1.);
#5299=CIRCLE('',#14404,1.);
#5300=CIRCLE('',#14405,1.);
#5301=CIRCLE('',#14406,1.);
#5302=CIRCLE('',#14408,1.5);
#5303=CIRCLE('',#14421,0.605);
#5304=CIRCLE('',#14423,0.605);
#5305=CIRCLE('',#14425,1.5);
#5306=CIRCLE('',#14434,0.205);
#5307=CIRCLE('',#14435,0.205);
#5308=CIRCLE('',#14437,1.);
#5309=CIRCLE('',#14438,1.);
#5310=CIRCLE('',#14443,1.);
#5311=CIRCLE('',#14444,1.);
#5312=CIRCLE('',#14449,0.2);
#5313=CIRCLE('',#14450,0.2);
#5314=CIRCLE('',#14455,0.375);
#5315=CIRCLE('',#14456,0.375);
#5316=CIRCLE('',#14458,0.225);
#5317=CIRCLE('',#14460,0.375);
#5318=CIRCLE('',#14461,0.375);
#5319=CIRCLE('',#14463,0.225);
#5320=CIRCLE('',#14465,0.375);
#5321=CIRCLE('',#14466,0.375);
#5322=CIRCLE('',#14468,0.225);
#5323=CIRCLE('',#14470,0.375);
#5324=CIRCLE('',#14471,0.375);
#5325=CIRCLE('',#14473,0.225000000000001);
#5326=CIRCLE('',#14475,0.225);
#5327=CIRCLE('',#14477,0.225);
#5328=CIRCLE('',#14479,0.225);
#5329=CIRCLE('',#14481,0.225000000000001);
#5330=CIRCLE('',#14499,1.070235);
#5331=CIRCLE('',#14500,1.070235);
#5332=CIRCLE('',#14501,0.309556);
#5333=CIRCLE('',#14502,1.070235);
#5334=CIRCLE('',#14503,1.070235);
#5335=CIRCLE('',#14505,1.070235);
#5336=CIRCLE('',#14507,0.6);
#5337=CIRCLE('',#14508,0.6);
#5338=CIRCLE('',#14510,0.66);
#5339=CIRCLE('',#14513,1.070235);
#5340=CIRCLE('',#14515,0.66);
#5341=CIRCLE('',#14519,1.129765);
#5342=CIRCLE('',#14520,1.129765);
#5343=CIRCLE('',#14521,0.309556);
#5344=CIRCLE('',#14522,1.129765);
#5345=CIRCLE('',#14523,1.129765);
#5346=CIRCLE('',#14525,1.129765);
#5347=CIRCLE('',#14527,1.54);
#5348=CIRCLE('',#14528,1.129765);
#5349=CIRCLE('',#14530,1.6);
#5350=CIRCLE('',#14532,1.6);
#5351=CIRCLE('',#14534,1.54);
#5352=CIRCLE('',#14539,0.29765);
#5353=CIRCLE('',#14541,0.29765);
#5354=CIRCLE('',#14543,0.29765);
#5355=CIRCLE('',#14545,0.29765);
#5356=CIRCLE('',#14547,0.29765);
#5357=CIRCLE('',#14549,0.29765);
#5358=CIRCLE('',#14551,0.29765);
#5359=CIRCLE('',#14554,0.303778037777585);
#5360=CIRCLE('',#14555,0.303778037777585);
#5361=CIRCLE('',#14557,1.123812);
#5362=CIRCLE('',#14558,1.123812);
#5363=CIRCLE('',#14559,1.123812);
#5364=CIRCLE('',#14560,1.123812);
#5365=CIRCLE('',#14561,1.123812);
#5366=CIRCLE('',#14562,1.123812);
#5367=CIRCLE('',#14563,1.123812);
#5368=CIRCLE('',#14564,1.123812);
#5369=CIRCLE('',#14565,1.123812);
#5370=CIRCLE('',#14567,1.076188);
#5371=CIRCLE('',#14568,0.303778037777585);
#5372=CIRCLE('',#14570,0.303778037777585);
#5373=CIRCLE('',#14572,1.076188);
#5374=CIRCLE('',#14573,0.303778037777585);
#5375=CIRCLE('',#14575,0.303778037777585);
#5376=CIRCLE('',#14577,1.076188);
#5377=CIRCLE('',#14578,1.076188);
#5378=CIRCLE('',#14579,0.303778037777585);
#5379=CIRCLE('',#14581,0.303778037777585);
#5380=CIRCLE('',#14583,1.076188);
#5381=CIRCLE('',#14584,0.303778037777585);
#5382=CIRCLE('',#14586,0.303778037777585);
#5383=CIRCLE('',#14588,1.076188);
#5384=CIRCLE('',#14589,0.303778037777585);
#5385=CIRCLE('',#14591,0.303778037777585);
#5386=CIRCLE('',#14593,1.076188);
#5387=CIRCLE('',#14594,1.076188);
#5388=CIRCLE('',#14595,1.076188);
#5389=CIRCLE('',#14597,0.303778037777585);
#5390=CIRCLE('',#14599,0.303778037777585);
#5391=CIRCLE('',#14604,1.119765);
#5392=CIRCLE('',#14605,1.085235);
#5393=CIRCLE('',#14607,1.119765);
#5394=CIRCLE('',#14609,1.085235);
#5395=CIRCLE('',#14612,1.119765);
#5396=CIRCLE('',#14613,1.085235);
#5397=CIRCLE('',#14615,1.119765);
#5398=CIRCLE('',#14617,1.085235);
#5399=CIRCLE('',#14626,0.3);
#5400=CIRCLE('',#14628,0.35);
#5401=CIRCLE('',#14630,0.35);
#5402=CIRCLE('',#14632,0.32);
#5403=CIRCLE('',#14634,0.22);
#5404=CIRCLE('',#14636,0.1954);
#5405=CIRCLE('',#14638,0.1954);
#5406=CIRCLE('',#14640,0.16);
#5407=CIRCLE('',#14653,0.21);
#5408=CIRCLE('',#14654,0.21);
#5409=CIRCLE('',#14656,0.21);
#5410=CIRCLE('',#14657,0.21);
#5411=CIRCLE('',#14659,0.210000000000001);
#5412=CIRCLE('',#14660,0.210000000000001);
#5413=CIRCLE('',#14662,0.210000000000001);
#5414=CIRCLE('',#14663,0.210000000000001);
#5415=CIRCLE('',#14665,0.164999999999999);
#5416=CIRCLE('',#14666,0.164999999999999);
#5417=CIRCLE('',#14673,0.275);
#5418=CIRCLE('',#14674,0.275);
#5419=CIRCLE('',#14676,0.275);
#5420=CIRCLE('',#14677,0.275);
#5421=CIRCLE('',#14679,0.275);
#5422=CIRCLE('',#14680,0.275);
#5423=CIRCLE('',#14682,0.275);
#5424=CIRCLE('',#14683,0.275);
#5425=CIRCLE('',#14685,2.42);
#5426=CIRCLE('',#14686,2.42);
#5427=CIRCLE('',#14704,0.165);
#5428=CIRCLE('',#14705,0.165);
#5429=CIRCLE('',#14708,0.165);
#5430=CIRCLE('',#14709,0.165);
#5431=CIRCLE('',#14712,0.164999999999999);
#5432=CIRCLE('',#14713,0.164999999999999);
#5433=CIRCLE('',#14716,0.165);
#5434=CIRCLE('',#14717,0.165);
#5435=CIRCLE('',#14720,0.525);
#5436=CIRCLE('',#14721,0.525);
#5437=CIRCLE('',#14723,3.);
#5438=CIRCLE('',#14725,0.525);
#5439=CIRCLE('',#14726,0.525);
#5440=CIRCLE('',#14728,3.);
#5441=CIRCLE('',#14730,0.525);
#5442=CIRCLE('',#14731,0.525);
#5443=CIRCLE('',#14733,3.);
#5444=CIRCLE('',#14735,0.525);
#5445=CIRCLE('',#14736,0.525);
#5446=CIRCLE('',#14738,3.);
#5447=CIRCLE('',#14740,0.275);
#5448=CIRCLE('',#14741,0.275);
#5449=CIRCLE('',#14743,3.5);
#5450=CIRCLE('',#14744,3.);
#5451=CIRCLE('',#14745,3.);
#5452=CIRCLE('',#14746,3.);
#5453=CIRCLE('',#14747,3.);
#5454=CIRCLE('',#14748,3.);
#5455=CIRCLE('',#14749,0.275);
#5456=CIRCLE('',#14750,0.275);
#5457=CIRCLE('',#14751,0.275);
#5458=CIRCLE('',#14753,0.275);
#5459=CIRCLE('',#14755,0.275);
#5460=CIRCLE('',#14757,0.275);
#5461=CIRCLE('',#14759,3.);
#5462=CIRCLE('',#14761,2.35);
#5463=CIRCLE('',#14762,2.35);
#5464=CIRCLE('',#14764,1.6);
#5465=CIRCLE('',#14766,3.5);
#5466=CIRCLE('',#14768,1.6);
#5467=CIRCLE('',#14773,1.7);
#5468=CIRCLE('',#14774,1.7);
#5469=CIRCLE('',#14776,2.34);
#5470=CIRCLE('',#14777,2.34);
#5471=CIRCLE('',#14782,0.225);
#5472=CIRCLE('',#14783,0.225);
#5473=CIRCLE('',#14785,0.225);
#5474=CIRCLE('',#14786,0.225);
#5475=CIRCLE('',#14788,0.225);
#5476=CIRCLE('',#14789,0.225);
#5477=CIRCLE('',#14791,0.225000000000001);
#5478=CIRCLE('',#14792,0.225000000000001);
#5479=CIRCLE('',#14794,1.7);
#5480=CIRCLE('',#14795,1.7);
#5481=CIRCLE('',#14797,3.);
#5482=CIRCLE('',#14798,3.);
#5483=CIRCLE('',#14804,0.21);
#5484=CIRCLE('',#14806,0.21);
#5485=CIRCLE('',#14807,0.21);
#5486=CIRCLE('',#14808,0.21);
#5487=CIRCLE('',#14810,0.21);
#5488=CIRCLE('',#14812,0.21);
#5489=CIRCLE('',#14813,0.21);
#5490=CIRCLE('',#14814,0.21);
#5491=CIRCLE('',#14816,0.21);
#5492=CIRCLE('',#14818,0.21);
#5493=CIRCLE('',#14819,0.21);
#5494=CIRCLE('',#14820,0.21);
#5495=CIRCLE('',#14822,0.21);
#5496=CIRCLE('',#14824,0.21);
#5497=CIRCLE('',#14825,0.21);
#5498=CIRCLE('',#14826,0.21);
#5499=CIRCLE('',#14875,0.17);
#5500=CIRCLE('',#14877,0.1954);
#5501=CIRCLE('',#14879,0.1954);
#5502=CIRCLE('',#14881,0.125);
#5503=CIRCLE('',#14893,0.24505);
#5504=CIRCLE('',#14895,0.375);
#5505=CIRCLE('',#14897,0.425);
#5506=CIRCLE('',#14899,0.425);
#5507=CIRCLE('',#14901,0.395);
#5508=CIRCLE('',#14903,0.27);
#5509=CIRCLE('',#14905,0.24505);
#5510=CIRCLE('',#14910,1.63531);
#5511=CIRCLE('',#14911,1.63531);
#5512=CIRCLE('',#14912,0.412776);
#5513=CIRCLE('',#14913,1.63531);
#5514=CIRCLE('',#14914,1.63531);
#5515=CIRCLE('',#14916,1.63531);
#5516=CIRCLE('',#14918,1.);
#5517=CIRCLE('',#14919,1.);
#5518=CIRCLE('',#14921,1.1);
#5519=CIRCLE('',#14924,1.63531);
#5520=CIRCLE('',#14926,1.1);
#5521=CIRCLE('',#14930,1.71469);
#5522=CIRCLE('',#14931,1.71469);
#5523=CIRCLE('',#14932,0.412776);
#5524=CIRCLE('',#14933,1.71469);
#5525=CIRCLE('',#14934,1.71469);
#5526=CIRCLE('',#14936,1.71469);
#5527=CIRCLE('',#14938,2.25);
#5528=CIRCLE('',#14939,1.71469);
#5529=CIRCLE('',#14941,2.35);
#5530=CIRCLE('',#14943,2.35);
#5531=CIRCLE('',#14945,2.25);
#5532=CIRCLE('',#14950,0.3969);
#5533=CIRCLE('',#14952,0.3969);
#5534=CIRCLE('',#14954,0.3969);
#5535=CIRCLE('',#14956,0.3969);
#5536=CIRCLE('',#14958,0.3969);
#5537=CIRCLE('',#14960,0.3969);
#5538=CIRCLE('',#14962,0.3969);
#5539=CIRCLE('',#14964,0.3969);
#5540=CIRCLE('',#14967,0.405071403305639);
#5541=CIRCLE('',#14968,0.405071403305639);
#5542=CIRCLE('',#14970,1.706752);
#5543=CIRCLE('',#14971,1.706752);
#5544=CIRCLE('',#14972,1.706752);
#5545=CIRCLE('',#14973,1.706752);
#5546=CIRCLE('',#14974,1.706752);
#5547=CIRCLE('',#14975,1.706752);
#5548=CIRCLE('',#14976,1.706752);
#5549=CIRCLE('',#14977,1.706752);
#5550=CIRCLE('',#14978,1.706752);
#5551=CIRCLE('',#14980,1.643248);
#5552=CIRCLE('',#14981,0.405071403305639);
#5553=CIRCLE('',#14983,0.405071403305639);
#5554=CIRCLE('',#14985,1.643248);
#5555=CIRCLE('',#14986,0.405071403305639);
#5556=CIRCLE('',#14988,0.405071403305639);
#5557=CIRCLE('',#14990,1.643248);
#5558=CIRCLE('',#14991,0.405071403305639);
#5559=CIRCLE('',#14993,0.405071403305639);
#5560=CIRCLE('',#14995,1.643248);
#5561=CIRCLE('',#14996,0.405071403305639);
#5562=CIRCLE('',#14998,0.405071403305639);
#5563=CIRCLE('',#15000,1.643248);
#5564=CIRCLE('',#15001,0.405071403305639);
#5565=CIRCLE('',#15003,0.405071403305639);
#5566=CIRCLE('',#15005,1.643248);
#5567=CIRCLE('',#15006,0.405071403305639);
#5568=CIRCLE('',#15008,0.405071403305639);
#5569=CIRCLE('',#15010,1.643248);
#5570=CIRCLE('',#15011,1.643248);
#5571=CIRCLE('',#15012,1.643248);
#5572=CIRCLE('',#15014,0.405071403305639);
#5573=CIRCLE('',#15016,0.405071403305639);
#5574=CIRCLE('',#15021,1.70469);
#5575=CIRCLE('',#15022,1.65031);
#5576=CIRCLE('',#15024,1.70469);
#5577=CIRCLE('',#15026,1.65031);
#5578=CIRCLE('',#15029,1.70469);
#5579=CIRCLE('',#15030,1.65031);
#5580=CIRCLE('',#15032,1.70469);
#5581=CIRCLE('',#15034,1.65031);
#5582=CIRCLE('',#15044,0.165);
#5583=CIRCLE('',#15045,0.165);
#5584=CIRCLE('',#15049,0.6);
#5585=CIRCLE('',#15053,0.6);
#5586=CIRCLE('',#15055,0.8);
#5587=CIRCLE('',#15056,0.6);
#5588=CIRCLE('',#15058,0.8);
#5589=CIRCLE('',#15059,0.6);
#5590=CIRCLE('',#15062,0.6);
#5591=CIRCLE('',#15064,0.6);
#5592=CIRCLE('',#15069,0.605);
#5593=CIRCLE('',#15070,0.605);
#5594=CIRCLE('',#15072,0.8);
#5595=CIRCLE('',#15073,0.8);
#5596=CIRCLE('',#15078,0.605);
#5597=CIRCLE('',#15079,0.605);
#5598=CIRCLE('',#15081,0.8);
#5599=CIRCLE('',#15082,0.8);
#5600=CIRCLE('',#15087,0.605);
#5601=CIRCLE('',#15088,0.605);
#5602=CIRCLE('',#15090,0.8);
#5603=CIRCLE('',#15091,0.8);
#5604=CIRCLE('',#15096,0.165);
#5605=CIRCLE('',#15098,0.165);
#5606=CIRCLE('',#15099,0.165);
#5607=CIRCLE('',#15100,0.165);
#5608=CIRCLE('',#15102,0.165);
#5609=CIRCLE('',#15105,0.605);
#5610=CIRCLE('',#15106,0.605);
#5611=CIRCLE('',#15108,1.2);
#5612=CIRCLE('',#15109,1.2);
#5613=CIRCLE('',#15121,0.225);
#5614=CIRCLE('',#15122,0.225);
#5615=CIRCLE('',#15124,0.9);
#5616=CIRCLE('',#15125,0.9);
#5617=CIRCLE('',#15133,1.75);
#5618=CIRCLE('',#15134,1.75);
#5619=CIRCLE('',#15135,1.75);
#5620=CIRCLE('',#15136,1.75);
#5621=CIRCLE('',#15137,1.75);
#5622=CIRCLE('',#15138,1.75);
#5623=CIRCLE('',#15139,1.75);
#5624=CIRCLE('',#15140,1.75);
#5625=CIRCLE('',#15141,1.75);
#5626=CIRCLE('',#15142,1.75);
#5627=CIRCLE('',#15143,1.75);
#5628=CIRCLE('',#15144,1.75);
#5629=CIRCLE('',#15145,1.75);
#5630=CIRCLE('',#15146,1.75);
#5631=CIRCLE('',#15147,1.75);
#5632=CIRCLE('',#15148,1.75);
#5633=CIRCLE('',#15149,1.75);
#5634=CIRCLE('',#15150,1.75);
#5635=CIRCLE('',#15151,1.75);
#5636=CIRCLE('',#15152,1.75);
#5637=CIRCLE('',#15153,0.6);
#5638=CIRCLE('',#15155,0.6);
#5639=CIRCLE('',#15157,1.4);
#5640=CIRCLE('',#15158,1.4);
#5641=CIRCLE('',#15162,1.75);
#5642=CIRCLE('',#15165,1.75);
#5643=CIRCLE('',#15168,1.75);
#5644=CIRCLE('',#15171,1.75);
#5645=CIRCLE('',#15174,1.75);
#5646=CIRCLE('',#15177,1.75);
#5647=CIRCLE('',#15180,1.75);
#5648=CIRCLE('',#15183,1.75);
#5649=CIRCLE('',#15186,1.75);
#5650=CIRCLE('',#15189,1.75);
#5651=CIRCLE('',#15192,1.75);
#5652=CIRCLE('',#15195,1.75);
#5653=CIRCLE('',#15198,1.75);
#5654=CIRCLE('',#15201,1.75);
#5655=CIRCLE('',#15204,1.75);
#5656=CIRCLE('',#15207,1.75);
#5657=CIRCLE('',#15210,1.75);
#5658=CIRCLE('',#15213,1.75);
#5659=CIRCLE('',#15216,1.75);
#5660=CIRCLE('',#15219,1.75);
#5661=CIRCLE('',#15224,0.165);
#5662=CIRCLE('',#15225,0.165);
#5663=CIRCLE('',#15229,1.);
#5664=CIRCLE('',#15233,1.);
#5665=CIRCLE('',#15235,1.2);
#5666=CIRCLE('',#15236,1.);
#5667=CIRCLE('',#15238,1.2);
#5668=CIRCLE('',#15239,1.);
#5669=CIRCLE('',#15242,1.);
#5670=CIRCLE('',#15244,1.);
#5671=CIRCLE('',#15249,1.005);
#5672=CIRCLE('',#15250,1.005);
#5673=CIRCLE('',#15252,1.2);
#5674=CIRCLE('',#15253,1.2);
#5675=CIRCLE('',#15258,1.005);
#5676=CIRCLE('',#15259,1.005);
#5677=CIRCLE('',#15261,1.2);
#5678=CIRCLE('',#15262,1.2);
#5679=CIRCLE('',#15268,1.005);
#5680=CIRCLE('',#15269,1.005);
#5681=CIRCLE('',#15271,1.5);
#5682=CIRCLE('',#15272,1.5);
#5683=CIRCLE('',#15284,0.225);
#5684=CIRCLE('',#15285,0.225);
#5685=CIRCLE('',#15287,1.3);
#5686=CIRCLE('',#15288,1.3);
#5687=CIRCLE('',#15293,0.1954);
#5688=CIRCLE('',#15302,0.17);
#5689=CIRCLE('',#15304,0.1954);
#5690=CIRCLE('',#15311,3.75);
#5691=CIRCLE('',#15312,3.75);
#5692=CIRCLE('',#15313,3.75);
#5693=CIRCLE('',#15314,3.75);
#5694=CIRCLE('',#15315,3.75);
#5695=CIRCLE('',#15316,3.75);
#5696=CIRCLE('',#15317,3.75);
#5697=CIRCLE('',#15318,3.75);
#5698=CIRCLE('',#15319,3.75);
#5699=CIRCLE('',#15320,3.75);
#5700=CIRCLE('',#15321,3.75);
#5701=CIRCLE('',#15322,3.75);
#5702=CIRCLE('',#15323,3.75);
#5703=CIRCLE('',#15324,3.75);
#5704=CIRCLE('',#15325,3.75);
#5705=CIRCLE('',#15326,3.75);
#5706=CIRCLE('',#15327,3.75);
#5707=CIRCLE('',#15328,3.75);
#5708=CIRCLE('',#15329,3.75);
#5709=CIRCLE('',#15330,3.75);
#5710=CIRCLE('',#15331,3.75);
#5711=CIRCLE('',#15332,3.75);
#5712=CIRCLE('',#15333,3.75);
#5713=CIRCLE('',#15334,3.75);
#5714=CIRCLE('',#15335,3.75);
#5715=CIRCLE('',#15336,3.75);
#5716=CIRCLE('',#15337,3.75);
#5717=CIRCLE('',#15338,3.75);
#5718=CIRCLE('',#15339,3.75);
#5719=CIRCLE('',#15340,3.75);
#5720=CIRCLE('',#15341,3.75);
#5721=CIRCLE('',#15342,3.75);
#5722=CIRCLE('',#15343,3.75);
#5723=CIRCLE('',#15344,3.75);
#5724=CIRCLE('',#15345,3.75);
#5725=CIRCLE('',#15346,3.75);
#5726=CIRCLE('',#15347,3.75);
#5727=CIRCLE('',#15348,3.75);
#5728=CIRCLE('',#15349,3.75);
#5729=CIRCLE('',#15350,3.75);
#5730=CIRCLE('',#15351,1.);
#5731=CIRCLE('',#15353,1.);
#5732=CIRCLE('',#15355,2.);
#5733=CIRCLE('',#15356,2.);
#5734=CIRCLE('',#15360,3.75);
#5735=CIRCLE('',#15363,3.75);
#5736=CIRCLE('',#15366,3.75);
#5737=CIRCLE('',#15369,3.75);
#5738=CIRCLE('',#15372,3.75);
#5739=CIRCLE('',#15375,3.75);
#5740=CIRCLE('',#15378,3.75);
#5741=CIRCLE('',#15381,3.75);
#5742=CIRCLE('',#15384,3.75);
#5743=CIRCLE('',#15387,3.75);
#5744=CIRCLE('',#15390,3.75);
#5745=CIRCLE('',#15393,3.75);
#5746=CIRCLE('',#15396,3.75);
#5747=CIRCLE('',#15399,3.75);
#5748=CIRCLE('',#15402,3.75);
#5749=CIRCLE('',#15405,3.75);
#5750=CIRCLE('',#15408,3.75);
#5751=CIRCLE('',#15411,3.75);
#5752=CIRCLE('',#15414,3.75);
#5753=CIRCLE('',#15417,3.75);
#5754=CIRCLE('',#15420,3.75);
#5755=CIRCLE('',#15423,3.75);
#5756=CIRCLE('',#15426,3.75);
#5757=CIRCLE('',#15429,3.75);
#5758=CIRCLE('',#15432,3.75);
#5759=CIRCLE('',#15435,3.75);
#5760=CIRCLE('',#15438,3.75);
#5761=CIRCLE('',#15441,3.75);
#5762=CIRCLE('',#15444,3.75);
#5763=CIRCLE('',#15447,3.75);
#5764=CIRCLE('',#15450,3.75);
#5765=CIRCLE('',#15453,3.75);
#5766=CIRCLE('',#15456,3.75);
#5767=CIRCLE('',#15459,3.75);
#5768=CIRCLE('',#15462,3.75);
#5769=CIRCLE('',#15465,3.75);
#5770=CIRCLE('',#15468,3.75);
#5771=CIRCLE('',#15471,3.75);
#5772=CIRCLE('',#15474,3.75);
#5773=CIRCLE('',#15477,3.75);
#5774=CIRCLE('',#15489,0.1954);
#5775=CIRCLE('',#15491,0.3);
#5776=CIRCLE('',#15493,0.35);
#5777=CIRCLE('',#15495,0.35);
#5778=CIRCLE('',#15497,0.32);
#5779=CIRCLE('',#15499,0.22);
#5780=CIRCLE('',#15501,0.1954);
#5781=VERTEX_POINT('',#19237);
#5782=VERTEX_POINT('',#19239);
#5783=VERTEX_POINT('',#19243);
#5784=VERTEX_POINT('',#19245);
#5785=VERTEX_POINT('',#19249);
#5786=VERTEX_POINT('',#19251);
#5787=VERTEX_POINT('',#19255);
#5788=VERTEX_POINT('',#19257);
#5789=VERTEX_POINT('',#19261);
#5790=VERTEX_POINT('',#19263);
#5791=VERTEX_POINT('',#19267);
#5792=VERTEX_POINT('',#19269);
#5793=VERTEX_POINT('',#19273);
#5794=VERTEX_POINT('',#19275);
#5795=VERTEX_POINT('',#19279);
#5796=VERTEX_POINT('',#19281);
#5797=VERTEX_POINT('',#19285);
#5798=VERTEX_POINT('',#19287);
#5799=VERTEX_POINT('',#19291);
#5800=VERTEX_POINT('',#19293);
#5801=VERTEX_POINT('',#19297);
#5802=VERTEX_POINT('',#19299);
#5803=VERTEX_POINT('',#19303);
#5804=VERTEX_POINT('',#19305);
#5805=VERTEX_POINT('',#19309);
#5806=VERTEX_POINT('',#19310);
#5807=VERTEX_POINT('',#19312);
#5808=VERTEX_POINT('',#19314);
#5809=VERTEX_POINT('',#19318);
#5810=VERTEX_POINT('',#19320);
#5811=VERTEX_POINT('',#19324);
#5812=VERTEX_POINT('',#19326);
#5813=VERTEX_POINT('',#19336);
#5814=VERTEX_POINT('',#19337);
#5815=VERTEX_POINT('',#19339);
#5816=VERTEX_POINT('',#19341);
#5817=VERTEX_POINT('',#19345);
#5818=VERTEX_POINT('',#19347);
#5819=VERTEX_POINT('',#19351);
#5820=VERTEX_POINT('',#19353);
#5821=VERTEX_POINT('',#19363);
#5822=VERTEX_POINT('',#19364);
#5823=VERTEX_POINT('',#19366);
#5824=VERTEX_POINT('',#19368);
#5825=VERTEX_POINT('',#19372);
#5826=VERTEX_POINT('',#19374);
#5827=VERTEX_POINT('',#19378);
#5828=VERTEX_POINT('',#19380);
#5829=VERTEX_POINT('',#19390);
#5830=VERTEX_POINT('',#19391);
#5831=VERTEX_POINT('',#19428);
#5832=VERTEX_POINT('',#19430);
#5833=VERTEX_POINT('',#19468);
#5834=VERTEX_POINT('',#19470);
#5835=VERTEX_POINT('',#19475);
#5836=VERTEX_POINT('',#19477);
#5837=VERTEX_POINT('',#19482);
#5838=VERTEX_POINT('',#19484);
#5839=VERTEX_POINT('',#19489);
#5840=VERTEX_POINT('',#19491);
#5841=VERTEX_POINT('',#19496);
#5842=VERTEX_POINT('',#19497);
#5843=VERTEX_POINT('',#19501);
#5844=VERTEX_POINT('',#19503);
#5845=VERTEX_POINT('',#19507);
#5846=VERTEX_POINT('',#19508);
#5847=VERTEX_POINT('',#19510);
#5848=VERTEX_POINT('',#19512);
#5849=VERTEX_POINT('',#19518);
#5850=VERTEX_POINT('',#19519);
#5851=VERTEX_POINT('',#19521);
#5852=VERTEX_POINT('',#19523);
#5853=VERTEX_POINT('',#19529);
#5854=VERTEX_POINT('',#19530);
#5855=VERTEX_POINT('',#19532);
#5856=VERTEX_POINT('',#19534);
#5857=VERTEX_POINT('',#19540);
#5858=VERTEX_POINT('',#19542);
#5859=VERTEX_POINT('',#19550);
#5860=VERTEX_POINT('',#19552);
#5861=VERTEX_POINT('',#19554);
#5862=VERTEX_POINT('',#19556);
#5863=VERTEX_POINT('',#19558);
#5864=VERTEX_POINT('',#19561);
#5865=VERTEX_POINT('',#19565);
#5866=VERTEX_POINT('',#19569);
#5867=VERTEX_POINT('',#19573);
#5868=VERTEX_POINT('',#19577);
#5869=VERTEX_POINT('',#19579);
#5870=VERTEX_POINT('',#19583);
#5871=VERTEX_POINT('',#19586);
#5872=VERTEX_POINT('',#19590);
#5873=VERTEX_POINT('',#19597);
#5874=VERTEX_POINT('',#19599);
#5875=VERTEX_POINT('',#19603);
#5876=VERTEX_POINT('',#19605);
#5877=VERTEX_POINT('',#19612);
#5878=VERTEX_POINT('',#19613);
#5879=VERTEX_POINT('',#19615);
#5880=VERTEX_POINT('',#19617);
#5881=VERTEX_POINT('',#19621);
#5882=VERTEX_POINT('',#19622);
#5883=VERTEX_POINT('',#19624);
#5884=VERTEX_POINT('',#19626);
#5885=VERTEX_POINT('',#19630);
#5886=VERTEX_POINT('',#19631);
#5887=VERTEX_POINT('',#19633);
#5888=VERTEX_POINT('',#19635);
#5889=VERTEX_POINT('',#19639);
#5890=VERTEX_POINT('',#19640);
#5891=VERTEX_POINT('',#19642);
#5892=VERTEX_POINT('',#19644);
#5893=VERTEX_POINT('',#19652);
#5894=VERTEX_POINT('',#19663);
#5895=VERTEX_POINT('',#19667);
#5896=VERTEX_POINT('',#19670);
#5897=VERTEX_POINT('',#19676);
#5898=VERTEX_POINT('',#19678);
#5899=VERTEX_POINT('',#19682);
#5900=VERTEX_POINT('',#19684);
#5901=VERTEX_POINT('',#19688);
#5902=VERTEX_POINT('',#19690);
#5903=VERTEX_POINT('',#19694);
#5904=VERTEX_POINT('',#19696);
#5905=VERTEX_POINT('',#19700);
#5906=VERTEX_POINT('',#19702);
#5907=VERTEX_POINT('',#19707);
#5908=VERTEX_POINT('',#19709);
#5909=VERTEX_POINT('',#19716);
#5910=VERTEX_POINT('',#19717);
#5911=VERTEX_POINT('',#19721);
#5912=VERTEX_POINT('',#19736);
#5913=VERTEX_POINT('',#19738);
#5914=VERTEX_POINT('',#19747);
#5915=VERTEX_POINT('',#19761);
#5916=VERTEX_POINT('',#19762);
#5917=VERTEX_POINT('',#19764);
#5918=VERTEX_POINT('',#19766);
#5919=VERTEX_POINT('',#19768);
#5920=VERTEX_POINT('',#19770);
#5921=VERTEX_POINT('',#19772);
#5922=VERTEX_POINT('',#19774);
#5923=VERTEX_POINT('',#19776);
#5924=VERTEX_POINT('',#19778);
#5925=VERTEX_POINT('',#19781);
#5926=VERTEX_POINT('',#19783);
#5927=VERTEX_POINT('',#19786);
#5928=VERTEX_POINT('',#19788);
#5929=VERTEX_POINT('',#19791);
#5930=VERTEX_POINT('',#19793);
#5931=VERTEX_POINT('',#19795);
#5932=VERTEX_POINT('',#19797);
#5933=VERTEX_POINT('',#19803);
#5934=VERTEX_POINT('',#19806);
#5935=VERTEX_POINT('',#19808);
#5936=VERTEX_POINT('',#19811);
#5937=VERTEX_POINT('',#19815);
#5938=VERTEX_POINT('',#19821);
#5939=VERTEX_POINT('',#19823);
#5940=VERTEX_POINT('',#19827);
#5941=VERTEX_POINT('',#19829);
#5942=VERTEX_POINT('',#19833);
#5943=VERTEX_POINT('',#19837);
#5944=VERTEX_POINT('',#19839);
#5945=VERTEX_POINT('',#19846);
#5946=VERTEX_POINT('',#19848);
#5947=VERTEX_POINT('',#19858);
#5948=VERTEX_POINT('',#19861);
#5949=VERTEX_POINT('',#19864);
#5950=VERTEX_POINT('',#19868);
#5951=VERTEX_POINT('',#19882);
#5952=VERTEX_POINT('',#19884);
#5953=VERTEX_POINT('',#19888);
#5954=VERTEX_POINT('',#19890);
#5955=VERTEX_POINT('',#19897);
#5956=VERTEX_POINT('',#19899);
#5957=VERTEX_POINT('',#19906);
#5958=VERTEX_POINT('',#19908);
#5959=VERTEX_POINT('',#19915);
#5960=VERTEX_POINT('',#19917);
#5961=VERTEX_POINT('',#19921);
#5962=VERTEX_POINT('',#19924);
#5963=VERTEX_POINT('',#19926);
#5964=VERTEX_POINT('',#19930);
#5965=VERTEX_POINT('',#19933);
#5966=VERTEX_POINT('',#19935);
#5967=VERTEX_POINT('',#19939);
#5968=VERTEX_POINT('',#19942);
#5969=VERTEX_POINT('',#19944);
#5970=VERTEX_POINT('',#19948);
#5971=VERTEX_POINT('',#19951);
#5972=VERTEX_POINT('',#19955);
#5973=VERTEX_POINT('',#19959);
#5974=VERTEX_POINT('',#19963);
#5975=VERTEX_POINT('',#19967);
#5976=VERTEX_POINT('',#19968);
#5977=VERTEX_POINT('',#19970);
#5978=VERTEX_POINT('',#19972);
#5979=VERTEX_POINT('',#19976);
#5980=VERTEX_POINT('',#19978);
#5981=VERTEX_POINT('',#19982);
#5982=VERTEX_POINT('',#19984);
#5983=VERTEX_POINT('',#19988);
#5984=VERTEX_POINT('',#19990);
#5985=VERTEX_POINT('',#19994);
#5986=VERTEX_POINT('',#19996);
#5987=VERTEX_POINT('',#20000);
#5988=VERTEX_POINT('',#20002);
#5989=VERTEX_POINT('',#20006);
#5990=VERTEX_POINT('',#20008);
#5991=VERTEX_POINT('',#20012);
#5992=VERTEX_POINT('',#20014);
#5993=VERTEX_POINT('',#20018);
#5994=VERTEX_POINT('',#20020);
#5995=VERTEX_POINT('',#20024);
#5996=VERTEX_POINT('',#20026);
#5997=VERTEX_POINT('',#20030);
#5998=VERTEX_POINT('',#20032);
#5999=VERTEX_POINT('',#20043);
#6000=VERTEX_POINT('',#20044);
#6001=VERTEX_POINT('',#20047);
#6002=VERTEX_POINT('',#20049);
#6003=VERTEX_POINT('',#20053);
#6004=VERTEX_POINT('',#20057);
#6005=VERTEX_POINT('',#20059);
#6006=VERTEX_POINT('',#20063);
#6007=VERTEX_POINT('',#20068);
#6008=VERTEX_POINT('',#20072);
#6009=VERTEX_POINT('',#20078);
#6010=VERTEX_POINT('',#20079);
#6011=VERTEX_POINT('',#20082);
#6012=VERTEX_POINT('',#20084);
#6013=VERTEX_POINT('',#20088);
#6014=VERTEX_POINT('',#20092);
#6015=VERTEX_POINT('',#20094);
#6016=VERTEX_POINT('',#20097);
#6017=VERTEX_POINT('',#20101);
#6018=VERTEX_POINT('',#20105);
#6019=VERTEX_POINT('',#20113);
#6020=VERTEX_POINT('',#20114);
#6021=VERTEX_POINT('',#20117);
#6022=VERTEX_POINT('',#20118);
#6023=VERTEX_POINT('',#20121);
#6024=VERTEX_POINT('',#20122);
#6025=VERTEX_POINT('',#20125);
#6026=VERTEX_POINT('',#20126);
#6027=VERTEX_POINT('',#20129);
#6028=VERTEX_POINT('',#20130);
#6029=VERTEX_POINT('',#20133);
#6030=VERTEX_POINT('',#20134);
#6031=VERTEX_POINT('',#20137);
#6032=VERTEX_POINT('',#20138);
#6033=VERTEX_POINT('',#20142);
#6034=VERTEX_POINT('',#20143);
#6035=VERTEX_POINT('',#20166);
#6036=VERTEX_POINT('',#20168);
#6037=VERTEX_POINT('',#20193);
#6038=VERTEX_POINT('',#20195);
#6039=VERTEX_POINT('',#20218);
#6040=VERTEX_POINT('',#20220);
#6041=VERTEX_POINT('',#20243);
#6042=VERTEX_POINT('',#20245);
#6043=VERTEX_POINT('',#20248);
#6044=VERTEX_POINT('',#20250);
#6045=VERTEX_POINT('',#20273);
#6046=VERTEX_POINT('',#20275);
#6047=VERTEX_POINT('',#20298);
#6048=VERTEX_POINT('',#20300);
#6049=VERTEX_POINT('',#20323);
#6050=VERTEX_POINT('',#20325);
#6051=VERTEX_POINT('',#20350);
#6052=VERTEX_POINT('',#20354);
#6053=VERTEX_POINT('',#20379);
#6054=VERTEX_POINT('',#20383);
#6055=VERTEX_POINT('',#20408);
#6056=VERTEX_POINT('',#20410);
#6057=VERTEX_POINT('',#20414);
#6058=VERTEX_POINT('',#20439);
#6059=VERTEX_POINT('',#20443);
#6060=VERTEX_POINT('',#20468);
#6061=VERTEX_POINT('',#20472);
#6062=VERTEX_POINT('',#20497);
#6063=VERTEX_POINT('',#20500);
#6064=VERTEX_POINT('',#20502);
#6065=VERTEX_POINT('',#20534);
#6066=VERTEX_POINT('',#20536);
#6067=VERTEX_POINT('',#20539);
#6068=VERTEX_POINT('',#20543);
#6069=VERTEX_POINT('',#20548);
#6070=VERTEX_POINT('',#20550);
#6071=VERTEX_POINT('',#20553);
#6072=VERTEX_POINT('',#20557);
#6073=VERTEX_POINT('',#20568);
#6074=VERTEX_POINT('',#20571);
#6075=VERTEX_POINT('',#20575);
#6076=VERTEX_POINT('',#20579);
#6077=VERTEX_POINT('',#20583);
#6078=VERTEX_POINT('',#20586);
#6079=VERTEX_POINT('',#20590);
#6080=VERTEX_POINT('',#20594);
#6081=VERTEX_POINT('',#20599);
#6082=VERTEX_POINT('',#20600);
#6083=VERTEX_POINT('',#20602);
#6084=VERTEX_POINT('',#20604);
#6085=VERTEX_POINT('',#20608);
#6086=VERTEX_POINT('',#20610);
#6087=VERTEX_POINT('',#20614);
#6088=VERTEX_POINT('',#20616);
#6089=VERTEX_POINT('',#20620);
#6090=VERTEX_POINT('',#20622);
#6091=VERTEX_POINT('',#20626);
#6092=VERTEX_POINT('',#20628);
#6093=VERTEX_POINT('',#20639);
#6094=VERTEX_POINT('',#20641);
#6095=VERTEX_POINT('',#20645);
#6096=VERTEX_POINT('',#20647);
#6097=VERTEX_POINT('',#20651);
#6098=VERTEX_POINT('',#20653);
#6099=VERTEX_POINT('',#20657);
#6100=VERTEX_POINT('',#20659);
#6101=VERTEX_POINT('',#20663);
#6102=VERTEX_POINT('',#20665);
#6103=VERTEX_POINT('',#20669);
#6104=VERTEX_POINT('',#20670);
#6105=VERTEX_POINT('',#20672);
#6106=VERTEX_POINT('',#20674);
#6107=VERTEX_POINT('',#20678);
#6108=VERTEX_POINT('',#20680);
#6109=VERTEX_POINT('',#20684);
#6110=VERTEX_POINT('',#20686);
#6111=VERTEX_POINT('',#20694);
#6112=VERTEX_POINT('',#20696);
#6113=VERTEX_POINT('',#20700);
#6114=VERTEX_POINT('',#20702);
#6115=VERTEX_POINT('',#20706);
#6116=VERTEX_POINT('',#20708);
#6117=VERTEX_POINT('',#20712);
#6118=VERTEX_POINT('',#20714);
#6119=VERTEX_POINT('',#20718);
#6120=VERTEX_POINT('',#20719);
#6121=VERTEX_POINT('',#20721);
#6122=VERTEX_POINT('',#20723);
#6123=VERTEX_POINT('',#20727);
#6124=VERTEX_POINT('',#20729);
#6125=VERTEX_POINT('',#20731);
#6126=VERTEX_POINT('',#20733);
#6127=VERTEX_POINT('',#20737);
#6128=VERTEX_POINT('',#20741);
#6129=VERTEX_POINT('',#20745);
#6130=VERTEX_POINT('',#20749);
#6131=VERTEX_POINT('',#20757);
#6132=VERTEX_POINT('',#20758);
#6133=VERTEX_POINT('',#20760);
#6134=VERTEX_POINT('',#20762);
#6135=VERTEX_POINT('',#20766);
#6136=VERTEX_POINT('',#20768);
#6137=VERTEX_POINT('',#20772);
#6138=VERTEX_POINT('',#20774);
#6139=VERTEX_POINT('',#20784);
#6140=VERTEX_POINT('',#20785);
#6141=VERTEX_POINT('',#20822);
#6142=VERTEX_POINT('',#20824);
#6143=VERTEX_POINT('',#20862);
#6144=VERTEX_POINT('',#20864);
#6145=VERTEX_POINT('',#20869);
#6146=VERTEX_POINT('',#20871);
#6147=VERTEX_POINT('',#20876);
#6148=VERTEX_POINT('',#20878);
#6149=VERTEX_POINT('',#20883);
#6150=VERTEX_POINT('',#20885);
#6151=VERTEX_POINT('',#20890);
#6152=VERTEX_POINT('',#20891);
#6153=VERTEX_POINT('',#20893);
#6154=VERTEX_POINT('',#20895);
#6155=VERTEX_POINT('',#20901);
#6156=VERTEX_POINT('',#20902);
#6157=VERTEX_POINT('',#20904);
#6158=VERTEX_POINT('',#20906);
#6159=VERTEX_POINT('',#20912);
#6160=VERTEX_POINT('',#20913);
#6161=VERTEX_POINT('',#20915);
#6162=VERTEX_POINT('',#20917);
#6163=VERTEX_POINT('',#20923);
#6164=VERTEX_POINT('',#20924);
#6165=VERTEX_POINT('',#20926);
#6166=VERTEX_POINT('',#20928);
#6167=VERTEX_POINT('',#20934);
#6168=VERTEX_POINT('',#20936);
#6169=VERTEX_POINT('',#20940);
#6170=VERTEX_POINT('',#20942);
#6171=VERTEX_POINT('',#20948);
#6172=VERTEX_POINT('',#20950);
#6173=VERTEX_POINT('',#20952);
#6174=VERTEX_POINT('',#20955);
#6175=VERTEX_POINT('',#20959);
#6176=VERTEX_POINT('',#20963);
#6177=VERTEX_POINT('',#20967);
#6178=VERTEX_POINT('',#20971);
#6179=VERTEX_POINT('',#20973);
#6180=VERTEX_POINT('',#20977);
#6181=VERTEX_POINT('',#20980);
#6182=VERTEX_POINT('',#20984);
#6183=VERTEX_POINT('',#20991);
#6184=VERTEX_POINT('',#20993);
#6185=VERTEX_POINT('',#20997);
#6186=VERTEX_POINT('',#20999);
#6187=VERTEX_POINT('',#21006);
#6188=VERTEX_POINT('',#21008);
#6189=VERTEX_POINT('',#21012);
#6190=VERTEX_POINT('',#21014);
#6191=VERTEX_POINT('',#21018);
#6192=VERTEX_POINT('',#21020);
#6193=VERTEX_POINT('',#21024);
#6194=VERTEX_POINT('',#21026);
#6195=VERTEX_POINT('',#21030);
#6196=VERTEX_POINT('',#21032);
#6197=VERTEX_POINT('',#21036);
#6198=VERTEX_POINT('',#21038);
#6199=VERTEX_POINT('',#21046);
#6200=VERTEX_POINT('',#21047);
#6201=VERTEX_POINT('',#21051);
#6202=VERTEX_POINT('',#21053);
#6203=VERTEX_POINT('',#21055);
#6204=VERTEX_POINT('',#21058);
#6205=VERTEX_POINT('',#21062);
#6206=VERTEX_POINT('',#21063);
#6207=VERTEX_POINT('',#21067);
#6208=VERTEX_POINT('',#21069);
#6209=VERTEX_POINT('',#21071);
#6210=VERTEX_POINT('',#21074);
#6211=VERTEX_POINT('',#21078);
#6212=VERTEX_POINT('',#21079);
#6213=VERTEX_POINT('',#21083);
#6214=VERTEX_POINT('',#21085);
#6215=VERTEX_POINT('',#21087);
#6216=VERTEX_POINT('',#21090);
#6217=VERTEX_POINT('',#21094);
#6218=VERTEX_POINT('',#21095);
#6219=VERTEX_POINT('',#21099);
#6220=VERTEX_POINT('',#21101);
#6221=VERTEX_POINT('',#21103);
#6222=VERTEX_POINT('',#21106);
#6223=VERTEX_POINT('',#21111);
#6224=VERTEX_POINT('',#21113);
#6225=VERTEX_POINT('',#21115);
#6226=VERTEX_POINT('',#21117);
#6227=VERTEX_POINT('',#21122);
#6228=VERTEX_POINT('',#21124);
#6229=VERTEX_POINT('',#21126);
#6230=VERTEX_POINT('',#21128);
#6231=VERTEX_POINT('',#21132);
#6232=VERTEX_POINT('',#21134);
#6233=VERTEX_POINT('',#21136);
#6234=VERTEX_POINT('',#21138);
#6235=VERTEX_POINT('',#21141);
#6236=VERTEX_POINT('',#21143);
#6237=VERTEX_POINT('',#21145);
#6238=VERTEX_POINT('',#21147);
#6239=VERTEX_POINT('',#21151);
#6240=VERTEX_POINT('',#21155);
#6241=VERTEX_POINT('',#21159);
#6242=VERTEX_POINT('',#21163);
#6243=VERTEX_POINT('',#21169);
#6244=VERTEX_POINT('',#21173);
#6245=VERTEX_POINT('',#21177);
#6246=VERTEX_POINT('',#21181);
#6247=VERTEX_POINT('',#21189);
#6248=VERTEX_POINT('',#21190);
#6249=VERTEX_POINT('',#21192);
#6250=VERTEX_POINT('',#21194);
#6251=VERTEX_POINT('',#21198);
#6252=VERTEX_POINT('',#21200);
#6253=VERTEX_POINT('',#21204);
#6254=VERTEX_POINT('',#21206);
#6255=VERTEX_POINT('',#21210);
#6256=VERTEX_POINT('',#21212);
#6257=VERTEX_POINT('',#21216);
#6258=VERTEX_POINT('',#21218);
#6259=VERTEX_POINT('',#21222);
#6260=VERTEX_POINT('',#21224);
#6261=VERTEX_POINT('',#21228);
#6262=VERTEX_POINT('',#21230);
#6263=VERTEX_POINT('',#21240);
#6264=VERTEX_POINT('',#21241);
#6265=VERTEX_POINT('',#21243);
#6266=VERTEX_POINT('',#21245);
#6267=VERTEX_POINT('',#21249);
#6268=VERTEX_POINT('',#21251);
#6269=VERTEX_POINT('',#21255);
#6270=VERTEX_POINT('',#21257);
#6271=VERTEX_POINT('',#21261);
#6272=VERTEX_POINT('',#21263);
#6273=VERTEX_POINT('',#21267);
#6274=VERTEX_POINT('',#21269);
#6275=VERTEX_POINT('',#21273);
#6276=VERTEX_POINT('',#21275);
#6277=VERTEX_POINT('',#21279);
#6278=VERTEX_POINT('',#21281);
#6279=VERTEX_POINT('',#21294);
#6280=VERTEX_POINT('',#21295);
#6281=VERTEX_POINT('',#21297);
#6282=VERTEX_POINT('',#21299);
#6283=VERTEX_POINT('',#21303);
#6284=VERTEX_POINT('',#21305);
#6285=VERTEX_POINT('',#21309);
#6286=VERTEX_POINT('',#21311);
#6287=VERTEX_POINT('',#21315);
#6288=VERTEX_POINT('',#21317);
#6289=VERTEX_POINT('',#21321);
#6290=VERTEX_POINT('',#21323);
#6291=VERTEX_POINT('',#21331);
#6292=VERTEX_POINT('',#21334);
#6293=VERTEX_POINT('',#21338);
#6294=VERTEX_POINT('',#21342);
#6295=VERTEX_POINT('',#21348);
#6296=VERTEX_POINT('',#21349);
#6297=VERTEX_POINT('',#21351);
#6298=VERTEX_POINT('',#21353);
#6299=VERTEX_POINT('',#21357);
#6300=VERTEX_POINT('',#21359);
#6301=VERTEX_POINT('',#21363);
#6302=VERTEX_POINT('',#21365);
#6303=VERTEX_POINT('',#21369);
#6304=VERTEX_POINT('',#21371);
#6305=VERTEX_POINT('',#21375);
#6306=VERTEX_POINT('',#21377);
#6307=VERTEX_POINT('',#21386);
#6308=VERTEX_POINT('',#21389);
#6309=VERTEX_POINT('',#21392);
#6310=VERTEX_POINT('',#21396);
#6311=VERTEX_POINT('',#21400);
#6312=VERTEX_POINT('',#21404);
#6313=VERTEX_POINT('',#21407);
#6314=VERTEX_POINT('',#21415);
#6315=VERTEX_POINT('',#21416);
#6316=VERTEX_POINT('',#21419);
#6317=VERTEX_POINT('',#21421);
#6318=VERTEX_POINT('',#21425);
#6319=VERTEX_POINT('',#21429);
#6320=VERTEX_POINT('',#21431);
#6321=VERTEX_POINT('',#21435);
#6322=VERTEX_POINT('',#21440);
#6323=VERTEX_POINT('',#21444);
#6324=VERTEX_POINT('',#21450);
#6325=VERTEX_POINT('',#21451);
#6326=VERTEX_POINT('',#21454);
#6327=VERTEX_POINT('',#21456);
#6328=VERTEX_POINT('',#21460);
#6329=VERTEX_POINT('',#21464);
#6330=VERTEX_POINT('',#21466);
#6331=VERTEX_POINT('',#21469);
#6332=VERTEX_POINT('',#21473);
#6333=VERTEX_POINT('',#21477);
#6334=VERTEX_POINT('',#21485);
#6335=VERTEX_POINT('',#21486);
#6336=VERTEX_POINT('',#21489);
#6337=VERTEX_POINT('',#21490);
#6338=VERTEX_POINT('',#21493);
#6339=VERTEX_POINT('',#21494);
#6340=VERTEX_POINT('',#21497);
#6341=VERTEX_POINT('',#21498);
#6342=VERTEX_POINT('',#21501);
#6343=VERTEX_POINT('',#21502);
#6344=VERTEX_POINT('',#21505);
#6345=VERTEX_POINT('',#21506);
#6346=VERTEX_POINT('',#21509);
#6347=VERTEX_POINT('',#21510);
#6348=VERTEX_POINT('',#21513);
#6349=VERTEX_POINT('',#21514);
#6350=VERTEX_POINT('',#21518);
#6351=VERTEX_POINT('',#21519);
#6352=VERTEX_POINT('',#21542);
#6353=VERTEX_POINT('',#21544);
#6354=VERTEX_POINT('',#21569);
#6355=VERTEX_POINT('',#21571);
#6356=VERTEX_POINT('',#21594);
#6357=VERTEX_POINT('',#21596);
#6358=VERTEX_POINT('',#21619);
#6359=VERTEX_POINT('',#21621);
#6360=VERTEX_POINT('',#21634);
#6361=VERTEX_POINT('',#21637);
#6362=VERTEX_POINT('',#21650);
#6363=VERTEX_POINT('',#21652);
#6364=VERTEX_POINT('',#21675);
#6365=VERTEX_POINT('',#21677);
#6366=VERTEX_POINT('',#21700);
#6367=VERTEX_POINT('',#21702);
#6368=VERTEX_POINT('',#21725);
#6369=VERTEX_POINT('',#21727);
#6370=VERTEX_POINT('',#21752);
#6371=VERTEX_POINT('',#21756);
#6372=VERTEX_POINT('',#21781);
#6373=VERTEX_POINT('',#21785);
#6374=VERTEX_POINT('',#21810);
#6375=VERTEX_POINT('',#21814);
#6376=VERTEX_POINT('',#21815);
#6377=VERTEX_POINT('',#21842);
#6378=VERTEX_POINT('',#21846);
#6379=VERTEX_POINT('',#21871);
#6380=VERTEX_POINT('',#21875);
#6381=VERTEX_POINT('',#21900);
#6382=VERTEX_POINT('',#21904);
#6383=VERTEX_POINT('',#21929);
#6384=VERTEX_POINT('',#21932);
#6385=VERTEX_POINT('',#21934);
#6386=VERTEX_POINT('',#21966);
#6387=VERTEX_POINT('',#21968);
#6388=VERTEX_POINT('',#21971);
#6389=VERTEX_POINT('',#21975);
#6390=VERTEX_POINT('',#21980);
#6391=VERTEX_POINT('',#21982);
#6392=VERTEX_POINT('',#21985);
#6393=VERTEX_POINT('',#21989);
#6394=VERTEX_POINT('',#22001);
#6395=VERTEX_POINT('',#22003);
#6396=VERTEX_POINT('',#22008);
#6397=VERTEX_POINT('',#22009);
#6398=VERTEX_POINT('',#22011);
#6399=VERTEX_POINT('',#22013);
#6400=VERTEX_POINT('',#22017);
#6401=VERTEX_POINT('',#22019);
#6402=VERTEX_POINT('',#22023);
#6403=VERTEX_POINT('',#22027);
#6404=VERTEX_POINT('',#22033);
#6405=VERTEX_POINT('',#22035);
#6406=VERTEX_POINT('',#22038);
#6407=VERTEX_POINT('',#22040);
#6408=VERTEX_POINT('',#22045);
#6409=VERTEX_POINT('',#22049);
#6410=VERTEX_POINT('',#22056);
#6411=VERTEX_POINT('',#22058);
#6412=VERTEX_POINT('',#22062);
#6413=VERTEX_POINT('',#22064);
#6414=VERTEX_POINT('',#22071);
#6415=VERTEX_POINT('',#22073);
#6416=VERTEX_POINT('',#22077);
#6417=VERTEX_POINT('',#22079);
#6418=VERTEX_POINT('',#22086);
#6419=VERTEX_POINT('',#22088);
#6420=VERTEX_POINT('',#22092);
#6421=VERTEX_POINT('',#22094);
#6422=VERTEX_POINT('',#22101);
#6423=VERTEX_POINT('',#22102);
#6424=VERTEX_POINT('',#22106);
#6425=VERTEX_POINT('',#22107);
#6426=VERTEX_POINT('',#22109);
#6427=VERTEX_POINT('',#22111);
#6428=VERTEX_POINT('',#22113);
#6429=VERTEX_POINT('',#22117);
#6430=VERTEX_POINT('',#22132);
#6431=VERTEX_POINT('',#22134);
#6432=VERTEX_POINT('',#22168);
#6433=VERTEX_POINT('',#22170);
#6434=VERTEX_POINT('',#22174);
#6435=VERTEX_POINT('',#22176);
#6436=VERTEX_POINT('',#22183);
#6437=VERTEX_POINT('',#22184);
#6438=VERTEX_POINT('',#22186);
#6439=VERTEX_POINT('',#22188);
#6440=VERTEX_POINT('',#22192);
#6441=VERTEX_POINT('',#22194);
#6442=VERTEX_POINT('',#22198);
#6443=VERTEX_POINT('',#22200);
#6444=VERTEX_POINT('',#22210);
#6445=VERTEX_POINT('',#22212);
#6446=VERTEX_POINT('',#22216);
#6447=VERTEX_POINT('',#22218);
#6448=VERTEX_POINT('',#22225);
#6449=VERTEX_POINT('',#22226);
#6450=VERTEX_POINT('',#22228);
#6451=VERTEX_POINT('',#22230);
#6452=VERTEX_POINT('',#22234);
#6453=VERTEX_POINT('',#22236);
#6454=VERTEX_POINT('',#22240);
#6455=VERTEX_POINT('',#22242);
#6456=VERTEX_POINT('',#22246);
#6457=VERTEX_POINT('',#22247);
#6458=VERTEX_POINT('',#22249);
#6459=VERTEX_POINT('',#22320);
#6460=VERTEX_POINT('',#22322);
#6461=VERTEX_POINT('',#22393);
#6462=VERTEX_POINT('',#22395);
#6463=VERTEX_POINT('',#22466);
#6464=VERTEX_POINT('',#22468);
#6465=VERTEX_POINT('',#22539);
#6466=VERTEX_POINT('',#22541);
#6467=VERTEX_POINT('',#22612);
#6468=VERTEX_POINT('',#22614);
#6469=VERTEX_POINT('',#22685);
#6470=VERTEX_POINT('',#22687);
#6471=VERTEX_POINT('',#22758);
#6472=VERTEX_POINT('',#22760);
#6473=VERTEX_POINT('',#22831);
#6474=VERTEX_POINT('',#22833);
#6475=VERTEX_POINT('',#22904);
#6476=VERTEX_POINT('',#22906);
#6477=VERTEX_POINT('',#22977);
#6478=VERTEX_POINT('',#22979);
#6479=VERTEX_POINT('',#23050);
#6480=VERTEX_POINT('',#23052);
#6481=VERTEX_POINT('',#23123);
#6482=VERTEX_POINT('',#23125);
#6483=VERTEX_POINT('',#23196);
#6484=VERTEX_POINT('',#23198);
#6485=VERTEX_POINT('',#23269);
#6486=VERTEX_POINT('',#23271);
#6487=VERTEX_POINT('',#23342);
#6488=VERTEX_POINT('',#23344);
#6489=VERTEX_POINT('',#23415);
#6490=VERTEX_POINT('',#23417);
#6491=VERTEX_POINT('',#23488);
#6492=VERTEX_POINT('',#23490);
#6493=VERTEX_POINT('',#23561);
#6494=VERTEX_POINT('',#23563);
#6495=VERTEX_POINT('',#23634);
#6496=VERTEX_POINT('',#23636);
#6497=VERTEX_POINT('',#23707);
#6498=VERTEX_POINT('',#23709);
#6499=VERTEX_POINT('',#23780);
#6500=VERTEX_POINT('',#23782);
#6501=VERTEX_POINT('',#23853);
#6502=VERTEX_POINT('',#23855);
#6503=VERTEX_POINT('',#23926);
#6504=VERTEX_POINT('',#23928);
#6505=VERTEX_POINT('',#23999);
#6506=VERTEX_POINT('',#24001);
#6507=VERTEX_POINT('',#24072);
#6508=VERTEX_POINT('',#24074);
#6509=VERTEX_POINT('',#24145);
#6510=VERTEX_POINT('',#24147);
#6511=VERTEX_POINT('',#24218);
#6512=VERTEX_POINT('',#24220);
#6513=VERTEX_POINT('',#24291);
#6514=VERTEX_POINT('',#24293);
#6515=VERTEX_POINT('',#24364);
#6516=VERTEX_POINT('',#24366);
#6517=VERTEX_POINT('',#24437);
#6518=VERTEX_POINT('',#24439);
#6519=VERTEX_POINT('',#24510);
#6520=VERTEX_POINT('',#24512);
#6521=VERTEX_POINT('',#24583);
#6522=VERTEX_POINT('',#24585);
#6523=VERTEX_POINT('',#24656);
#6524=VERTEX_POINT('',#24658);
#6525=VERTEX_POINT('',#24729);
#6526=VERTEX_POINT('',#24731);
#6527=VERTEX_POINT('',#24802);
#6528=VERTEX_POINT('',#24804);
#6529=VERTEX_POINT('',#24875);
#6530=VERTEX_POINT('',#24877);
#6531=VERTEX_POINT('',#24948);
#6532=VERTEX_POINT('',#24950);
#6533=VERTEX_POINT('',#25021);
#6534=VERTEX_POINT('',#25023);
#6535=VERTEX_POINT('',#25094);
#6536=VERTEX_POINT('',#25170);
#6537=VERTEX_POINT('',#25172);
#6538=VERTEX_POINT('',#25316);
#6539=VERTEX_POINT('',#25318);
#6540=VERTEX_POINT('',#25391);
#6541=VERTEX_POINT('',#25534);
#6542=VERTEX_POINT('',#25607);
#6543=VERTEX_POINT('',#25750);
#6544=VERTEX_POINT('',#25823);
#6545=VERTEX_POINT('',#25966);
#6546=VERTEX_POINT('',#26039);
#6547=VERTEX_POINT('',#26182);
#6548=VERTEX_POINT('',#26255);
#6549=VERTEX_POINT('',#26398);
#6550=VERTEX_POINT('',#26471);
#6551=VERTEX_POINT('',#26614);
#6552=VERTEX_POINT('',#26687);
#6553=VERTEX_POINT('',#26830);
#6554=VERTEX_POINT('',#26903);
#6555=VERTEX_POINT('',#27046);
#6556=VERTEX_POINT('',#27119);
#6557=VERTEX_POINT('',#27262);
#6558=VERTEX_POINT('',#27335);
#6559=VERTEX_POINT('',#27478);
#6560=VERTEX_POINT('',#27551);
#6561=VERTEX_POINT('',#27694);
#6562=VERTEX_POINT('',#27767);
#6563=VERTEX_POINT('',#27910);
#6564=VERTEX_POINT('',#27983);
#6565=VERTEX_POINT('',#28126);
#6566=VERTEX_POINT('',#28199);
#6567=VERTEX_POINT('',#28342);
#6568=VERTEX_POINT('',#28415);
#6569=VERTEX_POINT('',#28558);
#6570=VERTEX_POINT('',#28631);
#6571=VERTEX_POINT('',#28774);
#6572=VERTEX_POINT('',#28847);
#6573=VERTEX_POINT('',#28990);
#6574=VERTEX_POINT('',#29063);
#6575=VERTEX_POINT('',#29206);
#6576=VERTEX_POINT('',#29279);
#6577=VERTEX_POINT('',#29422);
#6578=VERTEX_POINT('',#29495);
#6579=VERTEX_POINT('',#29638);
#6580=VERTEX_POINT('',#29711);
#6581=VERTEX_POINT('',#29854);
#6582=VERTEX_POINT('',#29927);
#6583=VERTEX_POINT('',#30070);
#6584=VERTEX_POINT('',#30143);
#6585=VERTEX_POINT('',#30286);
#6586=VERTEX_POINT('',#30359);
#6587=VERTEX_POINT('',#30502);
#6588=VERTEX_POINT('',#30575);
#6589=VERTEX_POINT('',#30718);
#6590=VERTEX_POINT('',#30791);
#6591=VERTEX_POINT('',#30934);
#6592=VERTEX_POINT('',#31007);
#6593=VERTEX_POINT('',#31150);
#6594=VERTEX_POINT('',#31223);
#6595=VERTEX_POINT('',#31366);
#6596=VERTEX_POINT('',#31439);
#6597=VERTEX_POINT('',#31582);
#6598=VERTEX_POINT('',#31655);
#6599=VERTEX_POINT('',#31798);
#6600=VERTEX_POINT('',#31871);
#6601=VERTEX_POINT('',#32014);
#6602=VERTEX_POINT('',#32087);
#6603=VERTEX_POINT('',#32230);
#6604=VERTEX_POINT('',#32303);
#6605=VERTEX_POINT('',#32446);
#6606=VERTEX_POINT('',#32519);
#6607=VERTEX_POINT('',#32662);
#6608=VERTEX_POINT('',#32735);
#6609=VERTEX_POINT('',#32878);
#6610=VERTEX_POINT('',#32951);
#6611=VERTEX_POINT('',#33094);
#6612=VERTEX_POINT('',#33167);
#6613=VERTEX_POINT('',#33310);
#6614=VERTEX_POINT('',#33383);
#6615=VERTEX_POINT('',#33526);
#6616=VERTEX_POINT('',#33599);
#6617=VERTEX_POINT('',#33742);
#6618=VERTEX_POINT('',#33820);
#6619=VERTEX_POINT('',#33822);
#6620=VERTEX_POINT('',#33827);
#6621=VERTEX_POINT('',#33828);
#6622=VERTEX_POINT('',#33830);
#6623=VERTEX_POINT('',#33832);
#6624=VERTEX_POINT('',#33836);
#6625=VERTEX_POINT('',#33838);
#6626=VERTEX_POINT('',#33842);
#6627=VERTEX_POINT('',#33846);
#6628=VERTEX_POINT('',#33852);
#6629=VERTEX_POINT('',#33854);
#6630=VERTEX_POINT('',#33857);
#6631=VERTEX_POINT('',#33859);
#6632=VERTEX_POINT('',#33864);
#6633=VERTEX_POINT('',#33868);
#6634=VERTEX_POINT('',#33875);
#6635=VERTEX_POINT('',#33877);
#6636=VERTEX_POINT('',#33881);
#6637=VERTEX_POINT('',#33883);
#6638=VERTEX_POINT('',#33890);
#6639=VERTEX_POINT('',#33892);
#6640=VERTEX_POINT('',#33896);
#6641=VERTEX_POINT('',#33898);
#6642=VERTEX_POINT('',#33905);
#6643=VERTEX_POINT('',#33906);
#6644=VERTEX_POINT('',#33943);
#6645=VERTEX_POINT('',#33945);
#6646=VERTEX_POINT('',#33983);
#6647=VERTEX_POINT('',#33985);
#6648=VERTEX_POINT('',#33989);
#6649=VERTEX_POINT('',#33991);
#6650=VERTEX_POINT('',#33998);
#6651=VERTEX_POINT('',#33999);
#6652=VERTEX_POINT('',#34001);
#6653=VERTEX_POINT('',#34003);
#6654=VERTEX_POINT('',#34007);
#6655=VERTEX_POINT('',#34009);
#6656=VERTEX_POINT('',#34013);
#6657=VERTEX_POINT('',#34015);
#6658=VERTEX_POINT('',#34025);
#6659=VERTEX_POINT('',#34027);
#6660=VERTEX_POINT('',#34031);
#6661=VERTEX_POINT('',#34033);
#6662=VERTEX_POINT('',#34040);
#6663=VERTEX_POINT('',#34043);
#6664=VERTEX_POINT('',#34044);
#6665=VERTEX_POINT('',#34046);
#6666=VERTEX_POINT('',#34048);
#6667=VERTEX_POINT('',#34052);
#6668=VERTEX_POINT('',#34054);
#6669=VERTEX_POINT('',#34058);
#6670=VERTEX_POINT('',#34060);
#6671=VERTEX_POINT('',#34064);
#6672=VERTEX_POINT('',#34066);
#6673=VERTEX_POINT('',#34070);
#6674=VERTEX_POINT('',#34072);
#6675=VERTEX_POINT('',#34080);
#6676=VERTEX_POINT('',#34083);
#6677=VERTEX_POINT('',#34090);
#6678=VERTEX_POINT('',#34091);
#6679=VERTEX_POINT('',#34093);
#6680=VERTEX_POINT('',#34095);
#6681=VERTEX_POINT('',#34099);
#6682=VERTEX_POINT('',#34101);
#6683=VERTEX_POINT('',#34105);
#6684=VERTEX_POINT('',#34107);
#6685=VERTEX_POINT('',#34111);
#6686=VERTEX_POINT('',#34112);
#6687=VERTEX_POINT('',#34114);
#6688=VERTEX_POINT('',#34185);
#6689=VERTEX_POINT('',#34187);
#6690=VERTEX_POINT('',#34258);
#6691=VERTEX_POINT('',#34260);
#6692=VERTEX_POINT('',#34331);
#6693=VERTEX_POINT('',#34333);
#6694=VERTEX_POINT('',#34404);
#6695=VERTEX_POINT('',#34406);
#6696=VERTEX_POINT('',#34477);
#6697=VERTEX_POINT('',#34479);
#6698=VERTEX_POINT('',#34550);
#6699=VERTEX_POINT('',#34552);
#6700=VERTEX_POINT('',#34623);
#6701=VERTEX_POINT('',#34625);
#6702=VERTEX_POINT('',#34696);
#6703=VERTEX_POINT('',#34698);
#6704=VERTEX_POINT('',#34769);
#6705=VERTEX_POINT('',#34771);
#6706=VERTEX_POINT('',#34842);
#6707=VERTEX_POINT('',#34844);
#6708=VERTEX_POINT('',#34915);
#6709=VERTEX_POINT('',#34917);
#6710=VERTEX_POINT('',#34988);
#6711=VERTEX_POINT('',#34990);
#6712=VERTEX_POINT('',#35061);
#6713=VERTEX_POINT('',#35063);
#6714=VERTEX_POINT('',#35134);
#6715=VERTEX_POINT('',#35136);
#6716=VERTEX_POINT('',#35207);
#6717=VERTEX_POINT('',#35209);
#6718=VERTEX_POINT('',#35280);
#6719=VERTEX_POINT('',#35282);
#6720=VERTEX_POINT('',#35353);
#6721=VERTEX_POINT('',#35355);
#6722=VERTEX_POINT('',#35426);
#6723=VERTEX_POINT('',#35428);
#6724=VERTEX_POINT('',#35499);
#6725=VERTEX_POINT('',#35501);
#6726=VERTEX_POINT('',#35572);
#6727=VERTEX_POINT('',#35574);
#6728=VERTEX_POINT('',#35645);
#6729=VERTEX_POINT('',#35647);
#6730=VERTEX_POINT('',#35718);
#6731=VERTEX_POINT('',#35720);
#6732=VERTEX_POINT('',#35791);
#6733=VERTEX_POINT('',#35793);
#6734=VERTEX_POINT('',#35864);
#6735=VERTEX_POINT('',#35866);
#6736=VERTEX_POINT('',#35937);
#6737=VERTEX_POINT('',#35939);
#6738=VERTEX_POINT('',#36010);
#6739=VERTEX_POINT('',#36012);
#6740=VERTEX_POINT('',#36083);
#6741=VERTEX_POINT('',#36085);
#6742=VERTEX_POINT('',#36156);
#6743=VERTEX_POINT('',#36158);
#6744=VERTEX_POINT('',#36229);
#6745=VERTEX_POINT('',#36231);
#6746=VERTEX_POINT('',#36302);
#6747=VERTEX_POINT('',#36304);
#6748=VERTEX_POINT('',#36375);
#6749=VERTEX_POINT('',#36377);
#6750=VERTEX_POINT('',#36448);
#6751=VERTEX_POINT('',#36450);
#6752=VERTEX_POINT('',#36521);
#6753=VERTEX_POINT('',#36523);
#6754=VERTEX_POINT('',#36594);
#6755=VERTEX_POINT('',#36596);
#6756=VERTEX_POINT('',#36667);
#6757=VERTEX_POINT('',#36669);
#6758=VERTEX_POINT('',#36740);
#6759=VERTEX_POINT('',#36742);
#6760=VERTEX_POINT('',#36813);
#6761=VERTEX_POINT('',#36815);
#6762=VERTEX_POINT('',#36886);
#6763=VERTEX_POINT('',#36888);
#6764=VERTEX_POINT('',#36959);
#6765=VERTEX_POINT('',#36961);
#6766=VERTEX_POINT('',#37032);
#6767=VERTEX_POINT('',#37034);
#6768=VERTEX_POINT('',#37105);
#6769=VERTEX_POINT('',#37107);
#6770=VERTEX_POINT('',#37178);
#6771=VERTEX_POINT('',#37180);
#6772=VERTEX_POINT('',#37251);
#6773=VERTEX_POINT('',#37253);
#6774=VERTEX_POINT('',#37324);
#6775=VERTEX_POINT('',#37326);
#6776=VERTEX_POINT('',#37397);
#6777=VERTEX_POINT('',#37399);
#6778=VERTEX_POINT('',#37470);
#6779=VERTEX_POINT('',#37472);
#6780=VERTEX_POINT('',#37543);
#6781=VERTEX_POINT('',#37545);
#6782=VERTEX_POINT('',#37616);
#6783=VERTEX_POINT('',#37618);
#6784=VERTEX_POINT('',#37689);
#6785=VERTEX_POINT('',#37691);
#6786=VERTEX_POINT('',#37762);
#6787=VERTEX_POINT('',#37764);
#6788=VERTEX_POINT('',#37835);
#6789=VERTEX_POINT('',#37837);
#6790=VERTEX_POINT('',#37908);
#6791=VERTEX_POINT('',#37910);
#6792=VERTEX_POINT('',#37981);
#6793=VERTEX_POINT('',#37983);
#6794=VERTEX_POINT('',#38054);
#6795=VERTEX_POINT('',#38056);
#6796=VERTEX_POINT('',#38127);
#6797=VERTEX_POINT('',#38129);
#6798=VERTEX_POINT('',#38200);
#6799=VERTEX_POINT('',#38202);
#6800=VERTEX_POINT('',#38273);
#6801=VERTEX_POINT('',#38275);
#6802=VERTEX_POINT('',#38346);
#6803=VERTEX_POINT('',#38348);
#6804=VERTEX_POINT('',#38419);
#6805=VERTEX_POINT('',#38421);
#6806=VERTEX_POINT('',#38492);
#6807=VERTEX_POINT('',#38494);
#6808=VERTEX_POINT('',#38565);
#6809=VERTEX_POINT('',#38567);
#6810=VERTEX_POINT('',#38638);
#6811=VERTEX_POINT('',#38640);
#6812=VERTEX_POINT('',#38711);
#6813=VERTEX_POINT('',#38713);
#6814=VERTEX_POINT('',#38784);
#6815=VERTEX_POINT('',#38786);
#6816=VERTEX_POINT('',#38857);
#6817=VERTEX_POINT('',#38859);
#6818=VERTEX_POINT('',#38930);
#6819=VERTEX_POINT('',#38932);
#6820=VERTEX_POINT('',#39003);
#6821=VERTEX_POINT('',#39005);
#6822=VERTEX_POINT('',#39076);
#6823=VERTEX_POINT('',#39078);
#6824=VERTEX_POINT('',#39149);
#6825=VERTEX_POINT('',#39151);
#6826=VERTEX_POINT('',#39222);
#6827=VERTEX_POINT('',#39224);
#6828=VERTEX_POINT('',#39295);
#6829=VERTEX_POINT('',#39297);
#6830=VERTEX_POINT('',#39368);
#6831=VERTEX_POINT('',#39370);
#6832=VERTEX_POINT('',#39441);
#6833=VERTEX_POINT('',#39443);
#6834=VERTEX_POINT('',#39514);
#6835=VERTEX_POINT('',#39516);
#6836=VERTEX_POINT('',#39587);
#6837=VERTEX_POINT('',#39589);
#6838=VERTEX_POINT('',#39660);
#6839=VERTEX_POINT('',#39662);
#6840=VERTEX_POINT('',#39733);
#6841=VERTEX_POINT('',#39735);
#6842=VERTEX_POINT('',#39806);
#6843=VERTEX_POINT('',#39808);
#6844=VERTEX_POINT('',#39879);
#6845=VERTEX_POINT('',#39955);
#6846=VERTEX_POINT('',#39957);
#6847=VERTEX_POINT('',#40101);
#6848=VERTEX_POINT('',#40108);
#6849=VERTEX_POINT('',#40320);
#6850=VERTEX_POINT('',#40327);
#6851=VERTEX_POINT('',#40402);
#6852=VERTEX_POINT('',#40550);
#6853=VERTEX_POINT('',#40762);
#6854=VERTEX_POINT('',#40769);
#6855=VERTEX_POINT('',#40844);
#6856=VERTEX_POINT('',#40992);
#6857=VERTEX_POINT('',#41204);
#6858=VERTEX_POINT('',#41211);
#6859=VERTEX_POINT('',#41286);
#6860=VERTEX_POINT('',#41434);
#6861=VERTEX_POINT('',#41646);
#6862=VERTEX_POINT('',#41653);
#6863=VERTEX_POINT('',#41728);
#6864=VERTEX_POINT('',#41876);
#6865=VERTEX_POINT('',#42088);
#6866=VERTEX_POINT('',#42095);
#6867=VERTEX_POINT('',#42170);
#6868=VERTEX_POINT('',#42318);
#6869=VERTEX_POINT('',#42530);
#6870=VERTEX_POINT('',#42537);
#6871=VERTEX_POINT('',#42612);
#6872=VERTEX_POINT('',#42760);
#6873=VERTEX_POINT('',#42972);
#6874=VERTEX_POINT('',#42979);
#6875=VERTEX_POINT('',#43054);
#6876=VERTEX_POINT('',#43202);
#6877=VERTEX_POINT('',#43414);
#6878=VERTEX_POINT('',#43421);
#6879=VERTEX_POINT('',#43496);
#6880=VERTEX_POINT('',#43644);
#6881=VERTEX_POINT('',#43856);
#6882=VERTEX_POINT('',#43863);
#6883=VERTEX_POINT('',#43938);
#6884=VERTEX_POINT('',#44086);
#6885=VERTEX_POINT('',#44298);
#6886=VERTEX_POINT('',#44305);
#6887=VERTEX_POINT('',#44380);
#6888=VERTEX_POINT('',#44528);
#6889=VERTEX_POINT('',#44740);
#6890=VERTEX_POINT('',#44747);
#6891=VERTEX_POINT('',#44822);
#6892=VERTEX_POINT('',#44970);
#6893=VERTEX_POINT('',#45182);
#6894=VERTEX_POINT('',#45189);
#6895=VERTEX_POINT('',#45264);
#6896=VERTEX_POINT('',#45412);
#6897=VERTEX_POINT('',#45624);
#6898=VERTEX_POINT('',#45631);
#6899=VERTEX_POINT('',#45706);
#6900=VERTEX_POINT('',#45854);
#6901=VERTEX_POINT('',#46066);
#6902=VERTEX_POINT('',#46073);
#6903=VERTEX_POINT('',#46148);
#6904=VERTEX_POINT('',#46296);
#6905=VERTEX_POINT('',#46508);
#6906=VERTEX_POINT('',#46515);
#6907=VERTEX_POINT('',#46590);
#6908=VERTEX_POINT('',#46738);
#6909=VERTEX_POINT('',#46950);
#6910=VERTEX_POINT('',#46957);
#6911=VERTEX_POINT('',#47032);
#6912=VERTEX_POINT('',#47180);
#6913=VERTEX_POINT('',#47392);
#6914=VERTEX_POINT('',#47399);
#6915=VERTEX_POINT('',#47474);
#6916=VERTEX_POINT('',#47622);
#6917=VERTEX_POINT('',#47834);
#6918=VERTEX_POINT('',#47841);
#6919=VERTEX_POINT('',#47916);
#6920=VERTEX_POINT('',#48064);
#6921=VERTEX_POINT('',#48276);
#6922=VERTEX_POINT('',#48283);
#6923=VERTEX_POINT('',#48358);
#6924=VERTEX_POINT('',#48506);
#6925=VERTEX_POINT('',#48718);
#6926=VERTEX_POINT('',#48725);
#6927=VERTEX_POINT('',#48800);
#6928=VERTEX_POINT('',#48948);
#6929=VERTEX_POINT('',#49160);
#6930=VERTEX_POINT('',#49167);
#6931=VERTEX_POINT('',#49242);
#6932=VERTEX_POINT('',#49390);
#6933=VERTEX_POINT('',#49602);
#6934=VERTEX_POINT('',#49609);
#6935=VERTEX_POINT('',#49684);
#6936=VERTEX_POINT('',#49832);
#6937=VERTEX_POINT('',#50044);
#6938=VERTEX_POINT('',#50051);
#6939=VERTEX_POINT('',#50126);
#6940=VERTEX_POINT('',#50274);
#6941=VERTEX_POINT('',#50486);
#6942=VERTEX_POINT('',#50493);
#6943=VERTEX_POINT('',#50568);
#6944=VERTEX_POINT('',#50716);
#6945=VERTEX_POINT('',#50928);
#6946=VERTEX_POINT('',#50935);
#6947=VERTEX_POINT('',#51010);
#6948=VERTEX_POINT('',#51158);
#6949=VERTEX_POINT('',#51370);
#6950=VERTEX_POINT('',#51377);
#6951=VERTEX_POINT('',#51452);
#6952=VERTEX_POINT('',#51600);
#6953=VERTEX_POINT('',#51812);
#6954=VERTEX_POINT('',#51819);
#6955=VERTEX_POINT('',#51894);
#6956=VERTEX_POINT('',#52042);
#6957=VERTEX_POINT('',#52254);
#6958=VERTEX_POINT('',#52261);
#6959=VERTEX_POINT('',#52336);
#6960=VERTEX_POINT('',#52484);
#6961=VERTEX_POINT('',#52696);
#6962=VERTEX_POINT('',#52703);
#6963=VERTEX_POINT('',#52778);
#6964=VERTEX_POINT('',#52926);
#6965=VERTEX_POINT('',#53138);
#6966=VERTEX_POINT('',#53145);
#6967=VERTEX_POINT('',#53220);
#6968=VERTEX_POINT('',#53368);
#6969=VERTEX_POINT('',#53580);
#6970=VERTEX_POINT('',#53587);
#6971=VERTEX_POINT('',#53662);
#6972=VERTEX_POINT('',#53810);
#6973=VERTEX_POINT('',#54022);
#6974=VERTEX_POINT('',#54029);
#6975=VERTEX_POINT('',#54104);
#6976=VERTEX_POINT('',#54252);
#6977=VERTEX_POINT('',#54464);
#6978=VERTEX_POINT('',#54471);
#6979=VERTEX_POINT('',#54546);
#6980=VERTEX_POINT('',#54694);
#6981=VERTEX_POINT('',#54906);
#6982=VERTEX_POINT('',#54913);
#6983=VERTEX_POINT('',#54988);
#6984=VERTEX_POINT('',#55136);
#6985=VERTEX_POINT('',#55348);
#6986=VERTEX_POINT('',#55355);
#6987=VERTEX_POINT('',#55430);
#6988=VERTEX_POINT('',#55578);
#6989=VERTEX_POINT('',#55790);
#6990=VERTEX_POINT('',#55797);
#6991=VERTEX_POINT('',#55872);
#6992=VERTEX_POINT('',#56020);
#6993=VERTEX_POINT('',#56232);
#6994=VERTEX_POINT('',#56239);
#6995=VERTEX_POINT('',#56314);
#6996=VERTEX_POINT('',#56462);
#6997=VERTEX_POINT('',#56674);
#6998=VERTEX_POINT('',#56681);
#6999=VERTEX_POINT('',#56756);
#7000=VERTEX_POINT('',#56904);
#7001=VERTEX_POINT('',#56977);
#7002=VERTEX_POINT('',#57120);
#7003=VERTEX_POINT('',#57198);
#7004=VERTEX_POINT('',#57346);
#7005=VERTEX_POINT('',#57353);
#7006=VERTEX_POINT('',#57565);
#7007=VERTEX_POINT('',#57644);
#7008=VERTEX_POINT('',#57645);
#7009=VERTEX_POINT('',#57647);
#7010=VERTEX_POINT('',#57649);
#7011=VERTEX_POINT('',#57653);
#7012=VERTEX_POINT('',#57655);
#7013=VERTEX_POINT('',#57659);
#7014=VERTEX_POINT('',#57661);
#7015=VERTEX_POINT('',#57665);
#7016=VERTEX_POINT('',#57667);
#7017=VERTEX_POINT('',#57671);
#7018=VERTEX_POINT('',#57673);
#7019=VERTEX_POINT('',#57682);
#7020=VERTEX_POINT('',#57685);
#7021=VERTEX_POINT('',#57688);
#7022=VERTEX_POINT('',#57692);
#7023=VERTEX_POINT('',#57696);
#7024=VERTEX_POINT('',#57700);
#7025=VERTEX_POINT('',#57703);
#7026=EDGE_CURVE('',#5781,#5781,#5189,.T.);
#7027=EDGE_CURVE('',#5781,#5782,#3411,.T.);
#7028=EDGE_CURVE('',#5782,#5782,#5190,.T.);
#7029=EDGE_CURVE('',#5783,#5783,#5191,.T.);
#7030=EDGE_CURVE('',#5783,#5784,#3412,.T.);
#7031=EDGE_CURVE('',#5784,#5784,#5192,.T.);
#7032=EDGE_CURVE('',#5785,#5785,#5193,.T.);
#7033=EDGE_CURVE('',#5785,#5786,#3413,.T.);
#7034=EDGE_CURVE('',#5786,#5786,#5194,.T.);
#7035=EDGE_CURVE('',#5787,#5787,#5195,.T.);
#7036=EDGE_CURVE('',#5787,#5788,#3414,.T.);
#7037=EDGE_CURVE('',#5788,#5788,#5196,.T.);
#7038=EDGE_CURVE('',#5789,#5789,#5197,.T.);
#7039=EDGE_CURVE('',#5789,#5790,#3415,.T.);
#7040=EDGE_CURVE('',#5790,#5790,#5198,.T.);
#7041=EDGE_CURVE('',#5791,#5791,#5199,.T.);
#7042=EDGE_CURVE('',#5791,#5792,#3416,.T.);
#7043=EDGE_CURVE('',#5792,#5792,#5200,.T.);
#7044=EDGE_CURVE('',#5793,#5793,#5201,.T.);
#7045=EDGE_CURVE('',#5793,#5794,#3417,.T.);
#7046=EDGE_CURVE('',#5794,#5794,#5202,.T.);
#7047=EDGE_CURVE('',#5795,#5795,#5203,.T.);
#7048=EDGE_CURVE('',#5795,#5796,#3418,.T.);
#7049=EDGE_CURVE('',#5796,#5796,#5204,.T.);
#7050=EDGE_CURVE('',#5797,#5797,#5205,.T.);
#7051=EDGE_CURVE('',#5797,#5798,#3419,.T.);
#7052=EDGE_CURVE('',#5798,#5798,#5206,.T.);
#7053=EDGE_CURVE('',#5799,#5799,#5207,.T.);
#7054=EDGE_CURVE('',#5799,#5800,#3420,.T.);
#7055=EDGE_CURVE('',#5800,#5800,#5208,.T.);
#7056=EDGE_CURVE('',#5801,#5801,#5209,.T.);
#7057=EDGE_CURVE('',#5801,#5802,#3421,.T.);
#7058=EDGE_CURVE('',#5802,#5802,#5210,.T.);
#7059=EDGE_CURVE('',#5803,#5803,#5211,.T.);
#7060=EDGE_CURVE('',#5803,#5804,#3422,.T.);
#7061=EDGE_CURVE('',#5804,#5804,#5212,.T.);
#7062=EDGE_CURVE('',#5805,#5806,#3423,.T.);
#7063=EDGE_CURVE('',#5806,#5807,#3424,.T.);
#7064=EDGE_CURVE('',#5808,#5807,#3425,.T.);
#7065=EDGE_CURVE('',#5805,#5808,#3426,.T.);
#7066=EDGE_CURVE('',#5809,#5805,#3427,.T.);
#7067=EDGE_CURVE('',#5810,#5808,#3428,.T.);
#7068=EDGE_CURVE('',#5809,#5810,#3429,.T.);
#7069=EDGE_CURVE('',#5811,#5809,#3430,.T.);
#7070=EDGE_CURVE('',#5812,#5810,#3431,.T.);
#7071=EDGE_CURVE('',#5811,#5812,#3432,.T.);
#7072=EDGE_CURVE('',#5806,#5811,#3433,.T.);
#7073=EDGE_CURVE('',#5807,#5812,#3434,.T.);
#7074=EDGE_CURVE('',#5813,#5814,#3435,.T.);
#7075=EDGE_CURVE('',#5814,#5815,#3436,.T.);
#7076=EDGE_CURVE('',#5816,#5815,#3437,.T.);
#7077=EDGE_CURVE('',#5813,#5816,#3438,.T.);
#7078=EDGE_CURVE('',#5817,#5813,#3439,.T.);
#7079=EDGE_CURVE('',#5818,#5816,#3440,.T.);
#7080=EDGE_CURVE('',#5817,#5818,#3441,.T.);
#7081=EDGE_CURVE('',#5819,#5817,#3442,.T.);
#7082=EDGE_CURVE('',#5820,#5818,#3443,.T.);
#7083=EDGE_CURVE('',#5819,#5820,#3444,.T.);
#7084=EDGE_CURVE('',#5814,#5819,#3445,.T.);
#7085=EDGE_CURVE('',#5815,#5820,#3446,.T.);
#7086=EDGE_CURVE('',#5821,#5822,#3447,.T.);
#7087=EDGE_CURVE('',#5822,#5823,#3448,.T.);
#7088=EDGE_CURVE('',#5824,#5823,#3449,.T.);
#7089=EDGE_CURVE('',#5821,#5824,#3450,.T.);
#7090=EDGE_CURVE('',#5825,#5821,#3451,.T.);
#7091=EDGE_CURVE('',#5826,#5824,#3452,.T.);
#7092=EDGE_CURVE('',#5825,#5826,#3453,.T.);
#7093=EDGE_CURVE('',#5827,#5825,#3454,.T.);
#7094=EDGE_CURVE('',#5828,#5826,#3455,.T.);
#7095=EDGE_CURVE('',#5827,#5828,#3456,.T.);
#7096=EDGE_CURVE('',#5822,#5827,#3457,.T.);
#7097=EDGE_CURVE('',#5823,#5828,#3458,.T.);
#7098=EDGE_CURVE('',#5829,#5830,#784,.T.);
#7099=EDGE_CURVE('',#5830,#5829,#785,.T.);
#7100=EDGE_CURVE('',#5830,#5831,#3459,.T.);
#7101=EDGE_CURVE('',#5832,#5831,#786,.T.);
#7102=EDGE_CURVE('',#5831,#5832,#787,.T.);
#7103=EDGE_CURVE('',#5833,#5833,#5213,.T.);
#7104=EDGE_CURVE('',#5833,#5834,#3460,.T.);
#7105=EDGE_CURVE('',#5834,#5834,#5214,.T.);
#7106=EDGE_CURVE('',#5835,#5835,#5215,.T.);
#7107=EDGE_CURVE('',#5835,#5836,#3461,.T.);
#7108=EDGE_CURVE('',#5836,#5836,#5216,.T.);
#7109=EDGE_CURVE('',#5837,#5837,#5217,.T.);
#7110=EDGE_CURVE('',#5837,#5838,#3462,.T.);
#7111=EDGE_CURVE('',#5838,#5838,#5218,.T.);
#7112=EDGE_CURVE('',#5839,#5839,#5219,.T.);
#7113=EDGE_CURVE('',#5839,#5840,#3463,.T.);
#7114=EDGE_CURVE('',#5840,#5840,#5220,.T.);
#7115=EDGE_CURVE('',#5841,#5842,#5221,.T.);
#7116=EDGE_CURVE('',#5842,#5841,#5222,.T.);
#7117=EDGE_CURVE('',#5843,#5841,#3464,.T.);
#7118=EDGE_CURVE('',#5844,#5843,#5223,.T.);
#7119=EDGE_CURVE('',#5842,#5844,#3465,.T.);
#7120=EDGE_CURVE('',#5845,#5846,#3466,.T.);
#7121=EDGE_CURVE('',#5845,#5847,#5224,.T.);
#7122=EDGE_CURVE('',#5848,#5847,#3467,.T.);
#7123=EDGE_CURVE('',#5846,#5848,#5225,.T.);
#7124=EDGE_CURVE('',#5847,#5845,#5226,.T.);
#7125=EDGE_CURVE('',#5849,#5850,#3468,.T.);
#7126=EDGE_CURVE('',#5849,#5851,#5227,.T.);
#7127=EDGE_CURVE('',#5852,#5851,#3469,.T.);
#7128=EDGE_CURVE('',#5850,#5852,#5228,.T.);
#7129=EDGE_CURVE('',#5851,#5849,#5229,.T.);
#7130=EDGE_CURVE('',#5853,#5854,#3470,.T.);
#7131=EDGE_CURVE('',#5853,#5855,#5230,.T.);
#7132=EDGE_CURVE('',#5856,#5855,#3471,.T.);
#7133=EDGE_CURVE('',#5854,#5856,#5231,.T.);
#7134=EDGE_CURVE('',#5855,#5853,#5232,.T.);
#7135=EDGE_CURVE('',#5857,#5857,#5233,.T.);
#7136=EDGE_CURVE('',#5857,#5858,#3472,.T.);
#7137=EDGE_CURVE('',#5858,#5843,#5234,.T.);
#7138=EDGE_CURVE('',#5844,#5856,#5235,.T.);
#7139=EDGE_CURVE('',#5854,#5852,#5236,.T.);
#7140=EDGE_CURVE('',#5850,#5848,#5237,.T.);
#7141=EDGE_CURVE('',#5846,#5858,#5238,.T.);
#7142=EDGE_CURVE('',#5859,#5859,#5239,.T.);
#7143=EDGE_CURVE('',#5860,#5860,#5240,.T.);
#7144=EDGE_CURVE('',#5861,#5861,#5241,.T.);
#7145=EDGE_CURVE('',#5862,#5862,#5242,.T.);
#7146=EDGE_CURVE('',#5863,#5863,#5243,.T.);
#7147=EDGE_CURVE('',#5864,#5864,#5244,.T.);
#7148=EDGE_CURVE('',#5864,#5860,#3473,.T.);
#7149=EDGE_CURVE('',#5865,#5865,#5245,.T.);
#7150=EDGE_CURVE('',#5865,#5863,#3474,.T.);
#7151=EDGE_CURVE('',#5866,#5866,#5246,.T.);
#7152=EDGE_CURVE('',#5866,#5861,#3475,.T.);
#7153=EDGE_CURVE('',#5867,#5867,#5247,.T.);
#7154=EDGE_CURVE('',#5867,#5862,#3476,.T.);
#7155=EDGE_CURVE('',#5868,#5868,#5248,.T.);
#7156=EDGE_CURVE('',#5868,#5869,#3477,.T.);
#7157=EDGE_CURVE('',#5869,#5869,#5249,.T.);
#7158=EDGE_CURVE('',#5870,#5870,#5250,.T.);
#7159=EDGE_CURVE('',#5859,#5871,#3478,.T.);
#7160=EDGE_CURVE('',#5871,#5871,#5251,.T.);
#7161=EDGE_CURVE('',#5870,#5872,#3479,.T.);
#7162=EDGE_CURVE('',#5872,#5872,#5252,.T.);
#7163=EDGE_CURVE('',#5873,#5873,#5253,.T.);
#7164=EDGE_CURVE('',#5873,#5874,#3480,.T.);
#7165=EDGE_CURVE('',#5874,#5874,#5254,.T.);
#7166=EDGE_CURVE('',#5875,#5875,#5255,.T.);
#7167=EDGE_CURVE('',#5875,#5876,#3481,.T.);
#7168=EDGE_CURVE('',#5876,#5876,#5256,.T.);
#7169=EDGE_CURVE('',#5877,#5878,#3482,.T.);
#7170=EDGE_CURVE('',#5879,#5877,#5257,.T.);
#7171=EDGE_CURVE('',#5880,#5879,#3483,.T.);
#7172=EDGE_CURVE('',#5878,#5880,#5258,.T.);
#7173=EDGE_CURVE('',#5881,#5882,#3484,.T.);
#7174=EDGE_CURVE('',#5883,#5881,#5259,.T.);
#7175=EDGE_CURVE('',#5884,#5883,#3485,.T.);
#7176=EDGE_CURVE('',#5882,#5884,#5260,.T.);
#7177=EDGE_CURVE('',#5885,#5886,#3486,.T.);
#7178=EDGE_CURVE('',#5887,#5885,#5261,.T.);
#7179=EDGE_CURVE('',#5888,#5887,#3487,.T.);
#7180=EDGE_CURVE('',#5886,#5888,#5262,.T.);
#7181=EDGE_CURVE('',#5889,#5890,#3488,.T.);
#7182=EDGE_CURVE('',#5891,#5889,#5263,.T.);
#7183=EDGE_CURVE('',#5892,#5891,#3489,.T.);
#7184=EDGE_CURVE('',#5890,#5892,#5264,.T.);
#7185=EDGE_CURVE('',#5883,#5877,#5265,.T.);
#7186=EDGE_CURVE('',#5887,#5881,#5266,.T.);
#7187=EDGE_CURVE('',#5891,#5885,#5267,.T.);
#7188=EDGE_CURVE('',#5879,#5889,#5268,.T.);
#7189=EDGE_CURVE('',#5893,#5893,#5269,.T.);
#7190=EDGE_CURVE('',#5892,#5886,#5270,.T.);
#7191=EDGE_CURVE('',#5888,#5882,#5271,.T.);
#7192=EDGE_CURVE('',#5884,#5878,#5272,.T.);
#7193=EDGE_CURVE('',#5880,#5890,#5273,.T.);
#7194=EDGE_CURVE('',#5893,#5894,#3490,.T.);
#7195=EDGE_CURVE('',#5894,#5894,#5274,.T.);
#7196=EDGE_CURVE('',#5895,#5895,#5275,.T.);
#7197=EDGE_CURVE('',#5896,#5896,#5276,.T.);
#7198=EDGE_CURVE('',#5896,#5895,#3491,.T.);
#7199=EDGE_CURVE('',#5897,#5897,#5277,.T.);
#7200=EDGE_CURVE('',#5897,#5898,#3492,.T.);
#7201=EDGE_CURVE('',#5898,#5898,#5278,.T.);
#7202=EDGE_CURVE('',#5899,#5899,#5279,.T.);
#7203=EDGE_CURVE('',#5899,#5900,#3493,.T.);
#7204=EDGE_CURVE('',#5900,#5900,#5280,.T.);
#7205=EDGE_CURVE('',#5901,#5901,#5281,.T.);
#7206=EDGE_CURVE('',#5901,#5902,#3494,.T.);
#7207=EDGE_CURVE('',#5902,#5902,#5282,.T.);
#7208=EDGE_CURVE('',#5903,#5903,#5283,.T.);
#7209=EDGE_CURVE('',#5903,#5904,#3495,.T.);
#7210=EDGE_CURVE('',#5904,#5904,#5284,.T.);
#7211=EDGE_CURVE('',#5905,#5905,#5285,.T.);
#7212=EDGE_CURVE('',#5905,#5906,#3496,.T.);
#7213=EDGE_CURVE('',#5906,#5906,#5286,.T.);
#7214=EDGE_CURVE('',#5907,#5907,#5287,.T.);
#7215=EDGE_CURVE('',#5907,#5908,#3497,.T.);
#7216=EDGE_CURVE('',#5908,#5908,#5288,.T.);
#7217=EDGE_CURVE('',#5909,#5910,#3498,.T.);
#7218=EDGE_CURVE('',#5909,#5910,#5289,.T.);
#7219=EDGE_CURVE('',#5911,#5909,#788,.T.);
#7220=EDGE_CURVE('',#5912,#5911,#5290,.T.);
#7221=EDGE_CURVE('',#5913,#5912,#789,.T.);
#7222=EDGE_CURVE('',#5913,#5914,#3499,.T.);
#7223=EDGE_CURVE('',#5914,#5914,#5291,.T.);
#7224=EDGE_CURVE('',#5910,#5913,#790,.T.);
#7225=EDGE_CURVE('',#5912,#5911,#3500,.T.);
#7226=EDGE_CURVE('',#5915,#5916,#3501,.T.);
#7227=EDGE_CURVE('',#5917,#5915,#5292,.T.);
#7228=EDGE_CURVE('',#5918,#5917,#3502,.T.);
#7229=EDGE_CURVE('',#5919,#5918,#5293,.T.);
#7230=EDGE_CURVE('',#5919,#5920,#3503,.T.);
#7231=EDGE_CURVE('',#5921,#5920,#5294,.T.);
#7232=EDGE_CURVE('',#5922,#5921,#3504,.T.);
#7233=EDGE_CURVE('',#5923,#5922,#5295,.T.);
#7234=EDGE_CURVE('',#5924,#5923,#3505,.T.);
#7235=EDGE_CURVE('',#5924,#5923,#3506,.T.);
#7236=EDGE_CURVE('',#5925,#5923,#5296,.T.);
#7237=EDGE_CURVE('',#5926,#5925,#3507,.T.);
#7238=EDGE_CURVE('',#5926,#5925,#3508,.T.);
#7239=EDGE_CURVE('',#5927,#5925,#5297,.T.);
#7240=EDGE_CURVE('',#5928,#5927,#3509,.T.);
#7241=EDGE_CURVE('',#5920,#5928,#5298,.T.);
#7242=EDGE_CURVE('',#5929,#5919,#5299,.T.);
#7243=EDGE_CURVE('',#5930,#5929,#3510,.T.);
#7244=EDGE_CURVE('',#5931,#5930,#5300,.T.);
#7245=EDGE_CURVE('',#5931,#5932,#3511,.T.);
#7246=EDGE_CURVE('',#5931,#5932,#3512,.T.);
#7247=EDGE_CURVE('',#5915,#5931,#5301,.T.);
#7248=EDGE_CURVE('',#5915,#5916,#3513,.T.);
#7249=EDGE_CURVE('',#5933,#5918,#3514,.T.);
#7250=EDGE_CURVE('',#5916,#5933,#3515,.T.);
#7251=EDGE_CURVE('',#5934,#5916,#3516,.T.);
#7252=EDGE_CURVE('',#5935,#5934,#5302,.T.);
#7253=EDGE_CURVE('',#5932,#5935,#3517,.T.);
#7254=EDGE_CURVE('',#5936,#5932,#3518,.T.);
#7255=EDGE_CURVE('',#5929,#5936,#3519,.T.);
#7256=EDGE_CURVE('',#5917,#5937,#3520,.T.);
#7257=EDGE_CURVE('',#5933,#5937,#3521,.T.);
#7258=EDGE_CURVE('',#5937,#5915,#3522,.T.);
#7259=EDGE_CURVE('',#5931,#5938,#3523,.T.);
#7260=EDGE_CURVE('',#5938,#5939,#3524,.T.);
#7261=EDGE_CURVE('',#5915,#5939,#3525,.T.);
#7262=EDGE_CURVE('',#5926,#5940,#3526,.T.);
#7263=EDGE_CURVE('',#5941,#5940,#3527,.T.);
#7264=EDGE_CURVE('',#5925,#5941,#3528,.T.);
#7265=EDGE_CURVE('',#5942,#5931,#3529,.T.);
#7266=EDGE_CURVE('',#5936,#5942,#3530,.T.);
#7267=EDGE_CURVE('',#5921,#5943,#3531,.T.);
#7268=EDGE_CURVE('',#5944,#5943,#3532,.T.);
#7269=EDGE_CURVE('',#5922,#5944,#3533,.T.);
#7270=EDGE_CURVE('',#5941,#5927,#3534,.T.);
#7271=EDGE_CURVE('',#5940,#5928,#3535,.T.);
#7272=EDGE_CURVE('',#5945,#5923,#3536,.T.);
#7273=EDGE_CURVE('',#5946,#5945,#3537,.T.);
#7274=EDGE_CURVE('',#5946,#5925,#3538,.T.);
#7275=EDGE_CURVE('',#5923,#5944,#3539,.T.);
#7276=EDGE_CURVE('',#5943,#5924,#3540,.T.);
#7277=EDGE_CURVE('',#5939,#5945,#3541,.T.);
#7278=EDGE_CURVE('',#5924,#5947,#3542,.T.);
#7279=EDGE_CURVE('',#5947,#5934,#3543,.T.);
#7280=EDGE_CURVE('',#5948,#5948,#5303,.T.);
#7281=EDGE_CURVE('',#5949,#5949,#5304,.T.);
#7282=EDGE_CURVE('',#5949,#5948,#3544,.T.);
#7283=EDGE_CURVE('',#5935,#5950,#3545,.T.);
#7284=EDGE_CURVE('',#5950,#5947,#5305,.T.);
#7285=EDGE_CURVE('',#5950,#5926,#3546,.T.);
#7286=EDGE_CURVE('',#5942,#5930,#3547,.T.);
#7287=EDGE_CURVE('',#5938,#5946,#3548,.T.);
#7288=EDGE_CURVE('',#5951,#5951,#5306,.T.);
#7289=EDGE_CURVE('',#5951,#5952,#3549,.T.);
#7290=EDGE_CURVE('',#5952,#5952,#5307,.T.);
#7291=EDGE_CURVE('',#5953,#5953,#5308,.T.);
#7292=EDGE_CURVE('',#5953,#5954,#3550,.T.);
#7293=EDGE_CURVE('',#5954,#5954,#5309,.T.);
#7294=EDGE_CURVE('',#5955,#5955,#5310,.T.);
#7295=EDGE_CURVE('',#5955,#5956,#3551,.T.);
#7296=EDGE_CURVE('',#5956,#5956,#5311,.T.);
#7297=EDGE_CURVE('',#5957,#5957,#5312,.T.);
#7298=EDGE_CURVE('',#5957,#5958,#3552,.T.);
#7299=EDGE_CURVE('',#5958,#5958,#5313,.T.);
#7300=EDGE_CURVE('',#5959,#5959,#5314,.T.);
#7301=EDGE_CURVE('',#5959,#5960,#3553,.T.);
#7302=EDGE_CURVE('',#5960,#5960,#5315,.T.);
#7303=EDGE_CURVE('',#5961,#5961,#5316,.T.);
#7304=EDGE_CURVE('',#5962,#5962,#5317,.T.);
#7305=EDGE_CURVE('',#5962,#5963,#3554,.T.);
#7306=EDGE_CURVE('',#5963,#5963,#5318,.T.);
#7307=EDGE_CURVE('',#5964,#5964,#5319,.T.);
#7308=EDGE_CURVE('',#5965,#5965,#5320,.T.);
#7309=EDGE_CURVE('',#5965,#5966,#3555,.T.);
#7310=EDGE_CURVE('',#5966,#5966,#5321,.T.);
#7311=EDGE_CURVE('',#5967,#5967,#5322,.T.);
#7312=EDGE_CURVE('',#5968,#5968,#5323,.T.);
#7313=EDGE_CURVE('',#5968,#5969,#3556,.T.);
#7314=EDGE_CURVE('',#5969,#5969,#5324,.T.);
#7315=EDGE_CURVE('',#5970,#5970,#5325,.T.);
#7316=EDGE_CURVE('',#5971,#5971,#5326,.T.);
#7317=EDGE_CURVE('',#5971,#5961,#3557,.T.);
#7318=EDGE_CURVE('',#5972,#5972,#5327,.T.);
#7319=EDGE_CURVE('',#5972,#5964,#3558,.T.);
#7320=EDGE_CURVE('',#5973,#5973,#5328,.T.);
#7321=EDGE_CURVE('',#5973,#5967,#3559,.T.);
#7322=EDGE_CURVE('',#5974,#5974,#5329,.T.);
#7323=EDGE_CURVE('',#5974,#5970,#3560,.T.);
#7324=EDGE_CURVE('',#5975,#5976,#3561,.T.);
#7325=EDGE_CURVE('',#5976,#5977,#3562,.T.);
#7326=EDGE_CURVE('',#5978,#5977,#3563,.T.);
#7327=EDGE_CURVE('',#5975,#5978,#3564,.T.);
#7328=EDGE_CURVE('',#5979,#5975,#3565,.T.);
#7329=EDGE_CURVE('',#5980,#5978,#3566,.T.);
#7330=EDGE_CURVE('',#5979,#5980,#3567,.T.);
#7331=EDGE_CURVE('',#5981,#5979,#3568,.T.);
#7332=EDGE_CURVE('',#5982,#5980,#3569,.T.);
#7333=EDGE_CURVE('',#5981,#5982,#3570,.T.);
#7334=EDGE_CURVE('',#5983,#5981,#3571,.T.);
#7335=EDGE_CURVE('',#5984,#5982,#3572,.T.);
#7336=EDGE_CURVE('',#5983,#5984,#3573,.T.);
#7337=EDGE_CURVE('',#5985,#5983,#3574,.T.);
#7338=EDGE_CURVE('',#5986,#5984,#3575,.T.);
#7339=EDGE_CURVE('',#5985,#5986,#3576,.T.);
#7340=EDGE_CURVE('',#5987,#5985,#3577,.T.);
#7341=EDGE_CURVE('',#5988,#5986,#3578,.T.);
#7342=EDGE_CURVE('',#5987,#5988,#3579,.T.);
#7343=EDGE_CURVE('',#5989,#5987,#3580,.T.);
#7344=EDGE_CURVE('',#5990,#5988,#3581,.T.);
#7345=EDGE_CURVE('',#5989,#5990,#3582,.T.);
#7346=EDGE_CURVE('',#5991,#5989,#3583,.T.);
#7347=EDGE_CURVE('',#5992,#5990,#3584,.T.);
#7348=EDGE_CURVE('',#5991,#5992,#3585,.T.);
#7349=EDGE_CURVE('',#5993,#5991,#3586,.T.);
#7350=EDGE_CURVE('',#5994,#5992,#3587,.T.);
#7351=EDGE_CURVE('',#5993,#5994,#3588,.T.);
#7352=EDGE_CURVE('',#5995,#5993,#3589,.T.);
#7353=EDGE_CURVE('',#5996,#5994,#3590,.T.);
#7354=EDGE_CURVE('',#5995,#5996,#3591,.T.);
#7355=EDGE_CURVE('',#5997,#5995,#3592,.T.);
#7356=EDGE_CURVE('',#5998,#5996,#3593,.T.);
#7357=EDGE_CURVE('',#5997,#5998,#3594,.T.);
#7358=EDGE_CURVE('',#5976,#5997,#3595,.T.);
#7359=EDGE_CURVE('',#5977,#5998,#3596,.T.);
#7360=EDGE_CURVE('',#5999,#6000,#5330,.T.);
#7361=EDGE_CURVE('',#6000,#5999,#5331,.T.);
#7362=EDGE_CURVE('',#6000,#6001,#5332,.T.);
#7363=EDGE_CURVE('',#6002,#6001,#5333,.T.);
#7364=EDGE_CURVE('',#6001,#6002,#5334,.T.);
#7365=EDGE_CURVE('',#6002,#6003,#3597,.T.);
#7366=EDGE_CURVE('',#6003,#6003,#5335,.T.);
#7367=EDGE_CURVE('',#6004,#6004,#5336,.T.);
#7368=EDGE_CURVE('',#6004,#6005,#3598,.T.);
#7369=EDGE_CURVE('',#6005,#6005,#5337,.T.);
#7370=EDGE_CURVE('',#6005,#6006,#3599,.T.);
#7371=EDGE_CURVE('',#6006,#6006,#5338,.T.);
#7372=EDGE_CURVE('',#6007,#6007,#5339,.T.);
#7373=EDGE_CURVE('',#6007,#5999,#3600,.T.);
#7374=EDGE_CURVE('',#6008,#6008,#5340,.T.);
#7375=EDGE_CURVE('',#6008,#6004,#3601,.T.);
#7376=EDGE_CURVE('',#6009,#6010,#5341,.T.);
#7377=EDGE_CURVE('',#6010,#6009,#5342,.T.);
#7378=EDGE_CURVE('',#6010,#6011,#5343,.T.);
#7379=EDGE_CURVE('',#6012,#6011,#5344,.T.);
#7380=EDGE_CURVE('',#6011,#6012,#5345,.T.);
#7381=EDGE_CURVE('',#6013,#6013,#5346,.T.);
#7382=EDGE_CURVE('',#6013,#6012,#3602,.T.);
#7383=EDGE_CURVE('',#6014,#6014,#5347,.T.);
#7384=EDGE_CURVE('',#6015,#6015,#5348,.T.);
#7385=EDGE_CURVE('',#6016,#6016,#5349,.T.);
#7386=EDGE_CURVE('',#6016,#6014,#3603,.T.);
#7387=EDGE_CURVE('',#6017,#6017,#5350,.T.);
#7388=EDGE_CURVE('',#6017,#6016,#3604,.T.);
#7389=EDGE_CURVE('',#6018,#6018,#5351,.T.);
#7390=EDGE_CURVE('',#6018,#6017,#3605,.T.);
#7391=EDGE_CURVE('',#6009,#6015,#3606,.T.);
#7392=EDGE_CURVE('',#6019,#6020,#5352,.T.);
#7393=EDGE_CURVE('',#6021,#6022,#5353,.T.);
#7394=EDGE_CURVE('',#6023,#6024,#5354,.T.);
#7395=EDGE_CURVE('',#6025,#6026,#5355,.T.);
#7396=EDGE_CURVE('',#6027,#6028,#5356,.T.);
#7397=EDGE_CURVE('',#6029,#6030,#5357,.T.);
#7398=EDGE_CURVE('',#6031,#6032,#5358,.T.);
#7399=EDGE_CURVE('',#6033,#6034,#791,.T.);
#7400=EDGE_CURVE('',#6035,#6033,#5359,.T.);
#7401=EDGE_CURVE('',#6036,#6035,#792,.T.);
#7402=EDGE_CURVE('',#6034,#6036,#5360,.T.);
#7403=EDGE_CURVE('',#6037,#6035,#5361,.T.);
#7404=EDGE_CURVE('',#6037,#6038,#793,.T.);
#7405=EDGE_CURVE('',#6039,#6038,#5362,.T.);
#7406=EDGE_CURVE('',#6039,#6040,#794,.T.);
#7407=EDGE_CURVE('',#6041,#6040,#5363,.T.);
#7408=EDGE_CURVE('',#6041,#6042,#3607,.T.);
#7409=EDGE_CURVE('',#6042,#6042,#5364,.T.);
#7410=EDGE_CURVE('',#6043,#6041,#5365,.T.);
#7411=EDGE_CURVE('',#6043,#6044,#795,.T.);
#7412=EDGE_CURVE('',#6045,#6044,#5366,.T.);
#7413=EDGE_CURVE('',#6045,#6046,#796,.T.);
#7414=EDGE_CURVE('',#6047,#6046,#5367,.T.);
#7415=EDGE_CURVE('',#6047,#6048,#797,.T.);
#7416=EDGE_CURVE('',#6049,#6048,#5368,.T.);
#7417=EDGE_CURVE('',#6049,#6050,#798,.T.);
#7418=EDGE_CURVE('',#6036,#6050,#5369,.T.);
#7419=EDGE_CURVE('',#6033,#6051,#5370,.T.);
#7420=EDGE_CURVE('',#6051,#6037,#5371,.T.);
#7421=EDGE_CURVE('',#6052,#6051,#799,.T.);
#7422=EDGE_CURVE('',#6038,#6052,#5372,.T.);
#7423=EDGE_CURVE('',#6052,#6053,#5373,.T.);
#7424=EDGE_CURVE('',#6053,#6039,#5374,.T.);
#7425=EDGE_CURVE('',#6054,#6053,#800,.T.);
#7426=EDGE_CURVE('',#6040,#6054,#5375,.T.);
#7427=EDGE_CURVE('',#6054,#6055,#5376,.T.);
#7428=EDGE_CURVE('',#6055,#6056,#5377,.T.);
#7429=EDGE_CURVE('',#6056,#6043,#5378,.T.);
#7430=EDGE_CURVE('',#6057,#6056,#801,.T.);
#7431=EDGE_CURVE('',#6044,#6057,#5379,.T.);
#7432=EDGE_CURVE('',#6057,#6058,#5380,.T.);
#7433=EDGE_CURVE('',#6058,#6045,#5381,.T.);
#7434=EDGE_CURVE('',#6059,#6058,#802,.T.);
#7435=EDGE_CURVE('',#6046,#6059,#5382,.T.);
#7436=EDGE_CURVE('',#6059,#6060,#5383,.T.);
#7437=EDGE_CURVE('',#6060,#6047,#5384,.T.);
#7438=EDGE_CURVE('',#6061,#6060,#803,.T.);
#7439=EDGE_CURVE('',#6048,#6061,#5385,.T.);
#7440=EDGE_CURVE('',#6062,#6062,#5386,.T.);
#7441=EDGE_CURVE('',#6062,#6055,#3608,.T.);
#7442=EDGE_CURVE('',#6063,#6034,#5387,.T.);
#7443=EDGE_CURVE('',#6063,#6064,#804,.T.);
#7444=EDGE_CURVE('',#6061,#6064,#5388,.T.);
#7445=EDGE_CURVE('',#6050,#6063,#5389,.T.);
#7446=EDGE_CURVE('',#6064,#6049,#5390,.T.);
#7447=EDGE_CURVE('',#6065,#6065,#5391,.T.);
#7448=EDGE_CURVE('',#6066,#6066,#5392,.T.);
#7449=EDGE_CURVE('',#6067,#6067,#5393,.T.);
#7450=EDGE_CURVE('',#6067,#6065,#3609,.T.);
#7451=EDGE_CURVE('',#6068,#6068,#5394,.T.);
#7452=EDGE_CURVE('',#6068,#6066,#3610,.T.);
#7453=EDGE_CURVE('',#6069,#6069,#5395,.T.);
#7454=EDGE_CURVE('',#6070,#6070,#5396,.T.);
#7455=EDGE_CURVE('',#6071,#6071,#5397,.T.);
#7456=EDGE_CURVE('',#6071,#6069,#3611,.T.);
#7457=EDGE_CURVE('',#6072,#6072,#5398,.T.);
#7458=EDGE_CURVE('',#6072,#6070,#3612,.T.);
#7459=EDGE_CURVE('',#6073,#6073,#5399,.T.);
#7460=EDGE_CURVE('',#6074,#6074,#5400,.T.);
#7461=EDGE_CURVE('',#6074,#6073,#3613,.T.);
#7462=EDGE_CURVE('',#6075,#6075,#5401,.T.);
#7463=EDGE_CURVE('',#6075,#6074,#3614,.T.);
#7464=EDGE_CURVE('',#6076,#6076,#5402,.T.);
#7465=EDGE_CURVE('',#6076,#6075,#3615,.T.);
#7466=EDGE_CURVE('',#6077,#6077,#5403,.T.);
#7467=EDGE_CURVE('',#6078,#6078,#5404,.F.);
#7468=EDGE_CURVE('',#6078,#6077,#3616,.T.);
#7469=EDGE_CURVE('',#6079,#6079,#5405,.F.);
#7470=EDGE_CURVE('',#6079,#6078,#3617,.T.);
#7471=EDGE_CURVE('',#6080,#6080,#5406,.T.);
#7472=EDGE_CURVE('',#6080,#6079,#3618,.T.);
#7473=EDGE_CURVE('',#6081,#6082,#3619,.T.);
#7474=EDGE_CURVE('',#6082,#6083,#3620,.T.);
#7475=EDGE_CURVE('',#6083,#6084,#3621,.T.);
#7476=EDGE_CURVE('',#6081,#6084,#3622,.T.);
#7477=EDGE_CURVE('',#6082,#6085,#3623,.T.);
#7478=EDGE_CURVE('',#6085,#6086,#3624,.T.);
#7479=EDGE_CURVE('',#6086,#6083,#3625,.T.);
#7480=EDGE_CURVE('',#6085,#6087,#3626,.T.);
#7481=EDGE_CURVE('',#6087,#6088,#3627,.T.);
#7482=EDGE_CURVE('',#6088,#6086,#3628,.T.);
#7483=EDGE_CURVE('',#6087,#6089,#3629,.T.);
#7484=EDGE_CURVE('',#6089,#6090,#3630,.T.);
#7485=EDGE_CURVE('',#6090,#6088,#3631,.T.);
#7486=EDGE_CURVE('',#6089,#6091,#3632,.T.);
#7487=EDGE_CURVE('',#6091,#6092,#3633,.T.);
#7488=EDGE_CURVE('',#6092,#6090,#3634,.T.);
#7489=EDGE_CURVE('',#6091,#6081,#3635,.T.);
#7490=EDGE_CURVE('',#6084,#6092,#3636,.T.);
#7491=EDGE_CURVE('',#6093,#6093,#5407,.T.);
#7492=EDGE_CURVE('',#6093,#6094,#3637,.T.);
#7493=EDGE_CURVE('',#6094,#6094,#5408,.T.);
#7494=EDGE_CURVE('',#6095,#6095,#5409,.T.);
#7495=EDGE_CURVE('',#6095,#6096,#3638,.T.);
#7496=EDGE_CURVE('',#6096,#6096,#5410,.T.);
#7497=EDGE_CURVE('',#6097,#6097,#5411,.T.);
#7498=EDGE_CURVE('',#6097,#6098,#3639,.T.);
#7499=EDGE_CURVE('',#6098,#6098,#5412,.T.);
#7500=EDGE_CURVE('',#6099,#6099,#5413,.T.);
#7501=EDGE_CURVE('',#6099,#6100,#3640,.T.);
#7502=EDGE_CURVE('',#6100,#6100,#5414,.T.);
#7503=EDGE_CURVE('',#6101,#6101,#5415,.T.);
#7504=EDGE_CURVE('',#6101,#6102,#3641,.T.);
#7505=EDGE_CURVE('',#6102,#6102,#5416,.T.);
#7506=EDGE_CURVE('',#6103,#6104,#3642,.T.);
#7507=EDGE_CURVE('',#6104,#6105,#3643,.T.);
#7508=EDGE_CURVE('',#6106,#6105,#3644,.T.);
#7509=EDGE_CURVE('',#6103,#6106,#3645,.T.);
#7510=EDGE_CURVE('',#6107,#6103,#3646,.T.);
#7511=EDGE_CURVE('',#6108,#6106,#3647,.T.);
#7512=EDGE_CURVE('',#6107,#6108,#3648,.T.);
#7513=EDGE_CURVE('',#6109,#6107,#3649,.T.);
#7514=EDGE_CURVE('',#6110,#6108,#3650,.T.);
#7515=EDGE_CURVE('',#6109,#6110,#3651,.T.);
#7516=EDGE_CURVE('',#6104,#6109,#3652,.T.);
#7517=EDGE_CURVE('',#6105,#6110,#3653,.T.);
#7518=EDGE_CURVE('',#6111,#6111,#5417,.T.);
#7519=EDGE_CURVE('',#6111,#6112,#3654,.T.);
#7520=EDGE_CURVE('',#6112,#6112,#5418,.T.);
#7521=EDGE_CURVE('',#6113,#6113,#5419,.T.);
#7522=EDGE_CURVE('',#6113,#6114,#3655,.T.);
#7523=EDGE_CURVE('',#6114,#6114,#5420,.T.);
#7524=EDGE_CURVE('',#6115,#6115,#5421,.T.);
#7525=EDGE_CURVE('',#6115,#6116,#3656,.T.);
#7526=EDGE_CURVE('',#6116,#6116,#5422,.T.);
#7527=EDGE_CURVE('',#6117,#6117,#5423,.T.);
#7528=EDGE_CURVE('',#6117,#6118,#3657,.T.);
#7529=EDGE_CURVE('',#6118,#6118,#5424,.T.);
#7530=EDGE_CURVE('',#6119,#6120,#3658,.T.);
#7531=EDGE_CURVE('',#6121,#6119,#5425,.T.);
#7532=EDGE_CURVE('',#6122,#6121,#3659,.T.);
#7533=EDGE_CURVE('',#6120,#6122,#5426,.T.);
#7534=EDGE_CURVE('',#6119,#6123,#3660,.T.);
#7535=EDGE_CURVE('',#6123,#6124,#3661,.T.);
#7536=EDGE_CURVE('',#6124,#6125,#3662,.T.);
#7537=EDGE_CURVE('',#6125,#6126,#3663,.T.);
#7538=EDGE_CURVE('',#6126,#6121,#3664,.T.);
#7539=EDGE_CURVE('',#6120,#6127,#3665,.T.);
#7540=EDGE_CURVE('',#6127,#6123,#3666,.T.);
#7541=EDGE_CURVE('',#6128,#6126,#3667,.T.);
#7542=EDGE_CURVE('',#6128,#6122,#3668,.T.);
#7543=EDGE_CURVE('',#6129,#6128,#3669,.T.);
#7544=EDGE_CURVE('',#6129,#6125,#3670,.T.);
#7545=EDGE_CURVE('',#6130,#6129,#3671,.T.);
#7546=EDGE_CURVE('',#6130,#6124,#3672,.T.);
#7547=EDGE_CURVE('',#6127,#6130,#3673,.T.);
#7548=EDGE_CURVE('',#6131,#6132,#3674,.T.);
#7549=EDGE_CURVE('',#6132,#6133,#3675,.T.);
#7550=EDGE_CURVE('',#6134,#6133,#3676,.T.);
#7551=EDGE_CURVE('',#6131,#6134,#3677,.T.);
#7552=EDGE_CURVE('',#6135,#6131,#3678,.T.);
#7553=EDGE_CURVE('',#6136,#6134,#3679,.T.);
#7554=EDGE_CURVE('',#6135,#6136,#3680,.T.);
#7555=EDGE_CURVE('',#6137,#6135,#3681,.T.);
#7556=EDGE_CURVE('',#6138,#6136,#3682,.T.);
#7557=EDGE_CURVE('',#6137,#6138,#3683,.T.);
#7558=EDGE_CURVE('',#6132,#6137,#3684,.T.);
#7559=EDGE_CURVE('',#6133,#6138,#3685,.T.);
#7560=EDGE_CURVE('',#6139,#6140,#805,.T.);
#7561=EDGE_CURVE('',#6140,#6139,#806,.T.);
#7562=EDGE_CURVE('',#6140,#6141,#3686,.T.);
#7563=EDGE_CURVE('',#6142,#6141,#807,.T.);
#7564=EDGE_CURVE('',#6141,#6142,#808,.T.);
#7565=EDGE_CURVE('',#6143,#6143,#5427,.T.);
#7566=EDGE_CURVE('',#6143,#6144,#3687,.T.);
#7567=EDGE_CURVE('',#6144,#6144,#5428,.T.);
#7568=EDGE_CURVE('',#6145,#6145,#5429,.T.);
#7569=EDGE_CURVE('',#6145,#6146,#3688,.T.);
#7570=EDGE_CURVE('',#6146,#6146,#5430,.T.);
#7571=EDGE_CURVE('',#6147,#6147,#5431,.T.);
#7572=EDGE_CURVE('',#6147,#6148,#3689,.T.);
#7573=EDGE_CURVE('',#6148,#6148,#5432,.T.);
#7574=EDGE_CURVE('',#6149,#6149,#5433,.T.);
#7575=EDGE_CURVE('',#6149,#6150,#3690,.T.);
#7576=EDGE_CURVE('',#6150,#6150,#5434,.T.);
#7577=EDGE_CURVE('',#6151,#6152,#3691,.T.);
#7578=EDGE_CURVE('',#6151,#6153,#5435,.T.);
#7579=EDGE_CURVE('',#6154,#6153,#3692,.T.);
#7580=EDGE_CURVE('',#6152,#6154,#5436,.T.);
#7581=EDGE_CURVE('',#6153,#6151,#5437,.T.);
#7582=EDGE_CURVE('',#6155,#6156,#3693,.T.);
#7583=EDGE_CURVE('',#6155,#6157,#5438,.T.);
#7584=EDGE_CURVE('',#6158,#6157,#3694,.T.);
#7585=EDGE_CURVE('',#6156,#6158,#5439,.T.);
#7586=EDGE_CURVE('',#6157,#6155,#5440,.T.);
#7587=EDGE_CURVE('',#6159,#6160,#3695,.T.);
#7588=EDGE_CURVE('',#6159,#6161,#5441,.T.);
#7589=EDGE_CURVE('',#6162,#6161,#3696,.T.);
#7590=EDGE_CURVE('',#6160,#6162,#5442,.T.);
#7591=EDGE_CURVE('',#6161,#6159,#5443,.T.);
#7592=EDGE_CURVE('',#6163,#6164,#3697,.T.);
#7593=EDGE_CURVE('',#6163,#6165,#5444,.T.);
#7594=EDGE_CURVE('',#6166,#6165,#3698,.T.);
#7595=EDGE_CURVE('',#6164,#6166,#5445,.T.);
#7596=EDGE_CURVE('',#6165,#6163,#5446,.T.);
#7597=EDGE_CURVE('',#6167,#6167,#5447,.T.);
#7598=EDGE_CURVE('',#6167,#6168,#3699,.T.);
#7599=EDGE_CURVE('',#6168,#6168,#5448,.T.);
#7600=EDGE_CURVE('',#6169,#6169,#5449,.T.);
#7601=EDGE_CURVE('',#6156,#6170,#5450,.T.);
#7602=EDGE_CURVE('',#6160,#6158,#5451,.T.);
#7603=EDGE_CURVE('',#6164,#6162,#5452,.T.);
#7604=EDGE_CURVE('',#6152,#6166,#5453,.T.);
#7605=EDGE_CURVE('',#6170,#6154,#5454,.T.);
#7606=EDGE_CURVE('',#6171,#6171,#5455,.T.);
#7607=EDGE_CURVE('',#6172,#6172,#5456,.T.);
#7608=EDGE_CURVE('',#6173,#6173,#5457,.T.);
#7609=EDGE_CURVE('',#6174,#6174,#5458,.T.);
#7610=EDGE_CURVE('',#6174,#6172,#3700,.T.);
#7611=EDGE_CURVE('',#6175,#6175,#5459,.T.);
#7612=EDGE_CURVE('',#6175,#6171,#3701,.T.);
#7613=EDGE_CURVE('',#6176,#6176,#5460,.T.);
#7614=EDGE_CURVE('',#6176,#6173,#3702,.T.);
#7615=EDGE_CURVE('',#6177,#6177,#5461,.T.);
#7616=EDGE_CURVE('',#6177,#6170,#3703,.T.);
#7617=EDGE_CURVE('',#6178,#6178,#5462,.T.);
#7618=EDGE_CURVE('',#6178,#6179,#3704,.T.);
#7619=EDGE_CURVE('',#6179,#6179,#5463,.T.);
#7620=EDGE_CURVE('',#6180,#6180,#5464,.T.);
#7621=EDGE_CURVE('',#6169,#6181,#3705,.T.);
#7622=EDGE_CURVE('',#6181,#6181,#5465,.T.);
#7623=EDGE_CURVE('',#6180,#6182,#3706,.T.);
#7624=EDGE_CURVE('',#6182,#6182,#5466,.T.);
#7625=EDGE_CURVE('',#6183,#6183,#5467,.T.);
#7626=EDGE_CURVE('',#6183,#6184,#3707,.T.);
#7627=EDGE_CURVE('',#6184,#6184,#5468,.T.);
#7628=EDGE_CURVE('',#6185,#6185,#5469,.T.);
#7629=EDGE_CURVE('',#6185,#6186,#3708,.T.);
#7630=EDGE_CURVE('',#6186,#6186,#5470,.T.);
#7631=EDGE_CURVE('',#6187,#6187,#5471,.T.);
#7632=EDGE_CURVE('',#6187,#6188,#3709,.T.);
#7633=EDGE_CURVE('',#6188,#6188,#5472,.T.);
#7634=EDGE_CURVE('',#6189,#6189,#5473,.T.);
#7635=EDGE_CURVE('',#6189,#6190,#3710,.T.);
#7636=EDGE_CURVE('',#6190,#6190,#5474,.T.);
#7637=EDGE_CURVE('',#6191,#6191,#5475,.T.);
#7638=EDGE_CURVE('',#6191,#6192,#3711,.T.);
#7639=EDGE_CURVE('',#6192,#6192,#5476,.T.);
#7640=EDGE_CURVE('',#6193,#6193,#5477,.T.);
#7641=EDGE_CURVE('',#6193,#6194,#3712,.T.);
#7642=EDGE_CURVE('',#6194,#6194,#5478,.T.);
#7643=EDGE_CURVE('',#6195,#6195,#5479,.T.);
#7644=EDGE_CURVE('',#6195,#6196,#3713,.T.);
#7645=EDGE_CURVE('',#6196,#6196,#5480,.T.);
#7646=EDGE_CURVE('',#6197,#6197,#5481,.T.);
#7647=EDGE_CURVE('',#6197,#6198,#3714,.T.);
#7648=EDGE_CURVE('',#6198,#6198,#5482,.T.);
#7649=EDGE_CURVE('',#6199,#6200,#3715,.T.);
#7650=EDGE_CURVE('',#6199,#6200,#5483,.T.);
#7651=EDGE_CURVE('',#6201,#6199,#3716,.T.);
#7652=EDGE_CURVE('',#6202,#6201,#5484,.T.);
#7653=EDGE_CURVE('',#6202,#6203,#3717,.T.);
#7654=EDGE_CURVE('',#6203,#6203,#5485,.T.);
#7655=EDGE_CURVE('',#6204,#6202,#5486,.T.);
#7656=EDGE_CURVE('',#6200,#6204,#3718,.T.);
#7657=EDGE_CURVE('',#6205,#6206,#3719,.T.);
#7658=EDGE_CURVE('',#6205,#6206,#5487,.T.);
#7659=EDGE_CURVE('',#6207,#6205,#3720,.T.);
#7660=EDGE_CURVE('',#6208,#6207,#5488,.T.);
#7661=EDGE_CURVE('',#6208,#6209,#3721,.T.);
#7662=EDGE_CURVE('',#6209,#6209,#5489,.T.);
#7663=EDGE_CURVE('',#6210,#6208,#5490,.T.);
#7664=EDGE_CURVE('',#6206,#6210,#3722,.T.);
#7665=EDGE_CURVE('',#6211,#6212,#3723,.T.);
#7666=EDGE_CURVE('',#6211,#6212,#5491,.T.);
#7667=EDGE_CURVE('',#6213,#6211,#3724,.T.);
#7668=EDGE_CURVE('',#6214,#6213,#5492,.T.);
#7669=EDGE_CURVE('',#6214,#6215,#3725,.T.);
#7670=EDGE_CURVE('',#6215,#6215,#5493,.T.);
#7671=EDGE_CURVE('',#6216,#6214,#5494,.T.);
#7672=EDGE_CURVE('',#6212,#6216,#3726,.T.);
#7673=EDGE_CURVE('',#6217,#6218,#3727,.T.);
#7674=EDGE_CURVE('',#6217,#6218,#5495,.T.);
#7675=EDGE_CURVE('',#6219,#6217,#3728,.T.);
#7676=EDGE_CURVE('',#6220,#6219,#5496,.T.);
#7677=EDGE_CURVE('',#6220,#6221,#3729,.T.);
#7678=EDGE_CURVE('',#6221,#6221,#5497,.T.);
#7679=EDGE_CURVE('',#6222,#6220,#5498,.T.);
#7680=EDGE_CURVE('',#6218,#6222,#3730,.T.);
#7681=EDGE_CURVE('',#6204,#6213,#3731,.T.);
#7682=EDGE_CURVE('',#6216,#6223,#3732,.T.);
#7683=EDGE_CURVE('',#6224,#6223,#3733,.T.);
#7684=EDGE_CURVE('',#6224,#6225,#3734,.T.);
#7685=EDGE_CURVE('',#6226,#6225,#3735,.T.);
#7686=EDGE_CURVE('',#6226,#6201,#3736,.T.);
#7687=EDGE_CURVE('',#6210,#6219,#3737,.T.);
#7688=EDGE_CURVE('',#6222,#6227,#3738,.T.);
#7689=EDGE_CURVE('',#6228,#6227,#3739,.T.);
#7690=EDGE_CURVE('',#6229,#6228,#3740,.T.);
#7691=EDGE_CURVE('',#6230,#6229,#3741,.T.);
#7692=EDGE_CURVE('',#6230,#6207,#3742,.T.);
#7693=EDGE_CURVE('',#6223,#6231,#3743,.T.);
#7694=EDGE_CURVE('',#6231,#6232,#3744,.T.);
#7695=EDGE_CURVE('',#6232,#6233,#3745,.T.);
#7696=EDGE_CURVE('',#6233,#6234,#3746,.T.);
#7697=EDGE_CURVE('',#6234,#6230,#3747,.T.);
#7698=EDGE_CURVE('',#6229,#6235,#3748,.T.);
#7699=EDGE_CURVE('',#6235,#6236,#3749,.T.);
#7700=EDGE_CURVE('',#6236,#6237,#3750,.T.);
#7701=EDGE_CURVE('',#6237,#6238,#3751,.T.);
#7702=EDGE_CURVE('',#6238,#6224,#3752,.T.);
#7703=EDGE_CURVE('',#6239,#6226,#3753,.T.);
#7704=EDGE_CURVE('',#6231,#6239,#3754,.T.);
#7705=EDGE_CURVE('',#6240,#6239,#3755,.T.);
#7706=EDGE_CURVE('',#6232,#6240,#3756,.T.);
#7707=EDGE_CURVE('',#6241,#6240,#3757,.T.);
#7708=EDGE_CURVE('',#6233,#6241,#3758,.T.);
#7709=EDGE_CURVE('',#6242,#6241,#3759,.T.);
#7710=EDGE_CURVE('',#6234,#6242,#3760,.T.);
#7711=EDGE_CURVE('',#6227,#6242,#3761,.T.);
#7712=EDGE_CURVE('',#6243,#6228,#3762,.T.);
#7713=EDGE_CURVE('',#6235,#6243,#3763,.T.);
#7714=EDGE_CURVE('',#6244,#6243,#3764,.T.);
#7715=EDGE_CURVE('',#6236,#6244,#3765,.T.);
#7716=EDGE_CURVE('',#6245,#6244,#3766,.T.);
#7717=EDGE_CURVE('',#6237,#6245,#3767,.T.);
#7718=EDGE_CURVE('',#6246,#6245,#3768,.T.);
#7719=EDGE_CURVE('',#6238,#6246,#3769,.T.);
#7720=EDGE_CURVE('',#6225,#6246,#3770,.T.);
#7721=EDGE_CURVE('',#6247,#6248,#3771,.T.);
#7722=EDGE_CURVE('',#6248,#6249,#3772,.T.);
#7723=EDGE_CURVE('',#6250,#6249,#3773,.T.);
#7724=EDGE_CURVE('',#6247,#6250,#3774,.T.);
#7725=EDGE_CURVE('',#6251,#6247,#3775,.T.);
#7726=EDGE_CURVE('',#6252,#6250,#3776,.T.);
#7727=EDGE_CURVE('',#6251,#6252,#3777,.T.);
#7728=EDGE_CURVE('',#6253,#6251,#3778,.T.);
#7729=EDGE_CURVE('',#6254,#6252,#3779,.T.);
#7730=EDGE_CURVE('',#6253,#6254,#3780,.T.);
#7731=EDGE_CURVE('',#6255,#6253,#3781,.T.);
#7732=EDGE_CURVE('',#6256,#6254,#3782,.T.);
#7733=EDGE_CURVE('',#6255,#6256,#3783,.T.);
#7734=EDGE_CURVE('',#6257,#6255,#3784,.T.);
#7735=EDGE_CURVE('',#6258,#6256,#3785,.T.);
#7736=EDGE_CURVE('',#6257,#6258,#3786,.T.);
#7737=EDGE_CURVE('',#6259,#6257,#3787,.T.);
#7738=EDGE_CURVE('',#6260,#6258,#3788,.T.);
#7739=EDGE_CURVE('',#6259,#6260,#3789,.T.);
#7740=EDGE_CURVE('',#6261,#6259,#3790,.T.);
#7741=EDGE_CURVE('',#6262,#6260,#3791,.T.);
#7742=EDGE_CURVE('',#6261,#6262,#3792,.T.);
#7743=EDGE_CURVE('',#6248,#6261,#3793,.T.);
#7744=EDGE_CURVE('',#6249,#6262,#3794,.T.);
#7745=EDGE_CURVE('',#6263,#6264,#3795,.T.);
#7746=EDGE_CURVE('',#6263,#6265,#3796,.T.);
#7747=EDGE_CURVE('',#6266,#6265,#3797,.T.);
#7748=EDGE_CURVE('',#6264,#6266,#3798,.T.);
#7749=EDGE_CURVE('',#6264,#6267,#3799,.T.);
#7750=EDGE_CURVE('',#6268,#6266,#3800,.T.);
#7751=EDGE_CURVE('',#6267,#6268,#3801,.T.);
#7752=EDGE_CURVE('',#6267,#6269,#3802,.T.);
#7753=EDGE_CURVE('',#6270,#6268,#3803,.T.);
#7754=EDGE_CURVE('',#6269,#6270,#3804,.T.);
#7755=EDGE_CURVE('',#6269,#6271,#3805,.T.);
#7756=EDGE_CURVE('',#6272,#6270,#3806,.T.);
#7757=EDGE_CURVE('',#6271,#6272,#3807,.T.);
#7758=EDGE_CURVE('',#6271,#6273,#3808,.T.);
#7759=EDGE_CURVE('',#6274,#6272,#3809,.T.);
#7760=EDGE_CURVE('',#6273,#6274,#3810,.T.);
#7761=EDGE_CURVE('',#6273,#6275,#3811,.T.);
#7762=EDGE_CURVE('',#6276,#6274,#3812,.T.);
#7763=EDGE_CURVE('',#6275,#6276,#3813,.T.);
#7764=EDGE_CURVE('',#6275,#6277,#3814,.T.);
#7765=EDGE_CURVE('',#6278,#6276,#3815,.T.);
#7766=EDGE_CURVE('',#6277,#6278,#3816,.T.);
#7767=EDGE_CURVE('',#6277,#6263,#3817,.T.);
#7768=EDGE_CURVE('',#6265,#6278,#3818,.T.);
#7769=EDGE_CURVE('',#6279,#6280,#3819,.T.);
#7770=EDGE_CURVE('',#6279,#6281,#3820,.T.);
#7771=EDGE_CURVE('',#6281,#6282,#3821,.T.);
#7772=EDGE_CURVE('',#6280,#6282,#3822,.T.);
#7773=EDGE_CURVE('',#6283,#6279,#3823,.T.);
#7774=EDGE_CURVE('',#6283,#6284,#3824,.T.);
#7775=EDGE_CURVE('',#6284,#6281,#3825,.T.);
#7776=EDGE_CURVE('',#6285,#6283,#3826,.T.);
#7777=EDGE_CURVE('',#6285,#6286,#3827,.T.);
#7778=EDGE_CURVE('',#6286,#6284,#3828,.T.);
#7779=EDGE_CURVE('',#6287,#6285,#3829,.T.);
#7780=EDGE_CURVE('',#6287,#6288,#3830,.T.);
#7781=EDGE_CURVE('',#6288,#6286,#3831,.T.);
#7782=EDGE_CURVE('',#6289,#6287,#3832,.T.);
#7783=EDGE_CURVE('',#6289,#6290,#3833,.T.);
#7784=EDGE_CURVE('',#6290,#6288,#3834,.T.);
#7785=EDGE_CURVE('',#6280,#6289,#3835,.T.);
#7786=EDGE_CURVE('',#6282,#6290,#3836,.T.);
#7787=EDGE_CURVE('',#6291,#6291,#5499,.T.);
#7788=EDGE_CURVE('',#6292,#6292,#5500,.T.);
#7789=EDGE_CURVE('',#6292,#6291,#3837,.T.);
#7790=EDGE_CURVE('',#6293,#6293,#5501,.F.);
#7791=EDGE_CURVE('',#6293,#6292,#3838,.T.);
#7792=EDGE_CURVE('',#6294,#6294,#5502,.T.);
#7793=EDGE_CURVE('',#6294,#6293,#3839,.T.);
#7794=EDGE_CURVE('',#6295,#6296,#3840,.T.);
#7795=EDGE_CURVE('',#6296,#6297,#3841,.T.);
#7796=EDGE_CURVE('',#6297,#6298,#3842,.T.);
#7797=EDGE_CURVE('',#6295,#6298,#3843,.T.);
#7798=EDGE_CURVE('',#6296,#6299,#3844,.T.);
#7799=EDGE_CURVE('',#6299,#6300,#3845,.T.);
#7800=EDGE_CURVE('',#6300,#6297,#3846,.T.);
#7801=EDGE_CURVE('',#6299,#6301,#3847,.T.);
#7802=EDGE_CURVE('',#6301,#6302,#3848,.T.);
#7803=EDGE_CURVE('',#6302,#6300,#3849,.T.);
#7804=EDGE_CURVE('',#6301,#6303,#3850,.T.);
#7805=EDGE_CURVE('',#6303,#6304,#3851,.T.);
#7806=EDGE_CURVE('',#6304,#6302,#3852,.T.);
#7807=EDGE_CURVE('',#6303,#6305,#3853,.T.);
#7808=EDGE_CURVE('',#6305,#6306,#3854,.T.);
#7809=EDGE_CURVE('',#6306,#6304,#3855,.T.);
#7810=EDGE_CURVE('',#6305,#6295,#3856,.T.);
#7811=EDGE_CURVE('',#6298,#6306,#3857,.T.);
#7812=EDGE_CURVE('',#6307,#6307,#5503,.T.);
#7813=EDGE_CURVE('',#6308,#6308,#5504,.T.);
#7814=EDGE_CURVE('',#6309,#6309,#5505,.T.);
#7815=EDGE_CURVE('',#6309,#6308,#3858,.T.);
#7816=EDGE_CURVE('',#6310,#6310,#5506,.T.);
#7817=EDGE_CURVE('',#6310,#6309,#3859,.T.);
#7818=EDGE_CURVE('',#6311,#6311,#5507,.T.);
#7819=EDGE_CURVE('',#6311,#6310,#3860,.T.);
#7820=EDGE_CURVE('',#6312,#6312,#5508,.T.);
#7821=EDGE_CURVE('',#6313,#6313,#5509,.F.);
#7822=EDGE_CURVE('',#6313,#6312,#3861,.T.);
#7823=EDGE_CURVE('',#6307,#6313,#3862,.T.);
#7824=EDGE_CURVE('',#6314,#6315,#5510,.T.);
#7825=EDGE_CURVE('',#6315,#6314,#5511,.T.);
#7826=EDGE_CURVE('',#6315,#6316,#5512,.T.);
#7827=EDGE_CURVE('',#6317,#6316,#5513,.T.);
#7828=EDGE_CURVE('',#6316,#6317,#5514,.T.);
#7829=EDGE_CURVE('',#6317,#6318,#3863,.T.);
#7830=EDGE_CURVE('',#6318,#6318,#5515,.T.);
#7831=EDGE_CURVE('',#6319,#6319,#5516,.T.);
#7832=EDGE_CURVE('',#6319,#6320,#3864,.T.);
#7833=EDGE_CURVE('',#6320,#6320,#5517,.T.);
#7834=EDGE_CURVE('',#6320,#6321,#3865,.T.);
#7835=EDGE_CURVE('',#6321,#6321,#5518,.T.);
#7836=EDGE_CURVE('',#6322,#6322,#5519,.T.);
#7837=EDGE_CURVE('',#6322,#6314,#3866,.T.);
#7838=EDGE_CURVE('',#6323,#6323,#5520,.T.);
#7839=EDGE_CURVE('',#6323,#6319,#3867,.T.);
#7840=EDGE_CURVE('',#6324,#6325,#5521,.T.);
#7841=EDGE_CURVE('',#6325,#6324,#5522,.T.);
#7842=EDGE_CURVE('',#6325,#6326,#5523,.T.);
#7843=EDGE_CURVE('',#6327,#6326,#5524,.T.);
#7844=EDGE_CURVE('',#6326,#6327,#5525,.T.);
#7845=EDGE_CURVE('',#6328,#6328,#5526,.T.);
#7846=EDGE_CURVE('',#6328,#6327,#3868,.T.);
#7847=EDGE_CURVE('',#6329,#6329,#5527,.T.);
#7848=EDGE_CURVE('',#6330,#6330,#5528,.T.);
#7849=EDGE_CURVE('',#6331,#6331,#5529,.T.);
#7850=EDGE_CURVE('',#6331,#6329,#3869,.T.);
#7851=EDGE_CURVE('',#6332,#6332,#5530,.T.);
#7852=EDGE_CURVE('',#6332,#6331,#3870,.T.);
#7853=EDGE_CURVE('',#6333,#6333,#5531,.T.);
#7854=EDGE_CURVE('',#6333,#6332,#3871,.T.);
#7855=EDGE_CURVE('',#6324,#6330,#3872,.T.);
#7856=EDGE_CURVE('',#6334,#6335,#5532,.T.);
#7857=EDGE_CURVE('',#6336,#6337,#5533,.T.);
#7858=EDGE_CURVE('',#6338,#6339,#5534,.T.);
#7859=EDGE_CURVE('',#6340,#6341,#5535,.T.);
#7860=EDGE_CURVE('',#6342,#6343,#5536,.T.);
#7861=EDGE_CURVE('',#6344,#6345,#5537,.T.);
#7862=EDGE_CURVE('',#6346,#6347,#5538,.T.);
#7863=EDGE_CURVE('',#6348,#6349,#5539,.T.);
#7864=EDGE_CURVE('',#6350,#6351,#809,.T.);
#7865=EDGE_CURVE('',#6352,#6350,#5540,.T.);
#7866=EDGE_CURVE('',#6353,#6352,#810,.T.);
#7867=EDGE_CURVE('',#6351,#6353,#5541,.T.);
#7868=EDGE_CURVE('',#6354,#6352,#5542,.T.);
#7869=EDGE_CURVE('',#6354,#6355,#811,.T.);
#7870=EDGE_CURVE('',#6356,#6355,#5543,.T.);
#7871=EDGE_CURVE('',#6356,#6357,#812,.T.);
#7872=EDGE_CURVE('',#6358,#6357,#5544,.T.);
#7873=EDGE_CURVE('',#6358,#6359,#813,.T.);
#7874=EDGE_CURVE('',#6359,#6360,#3873,.T.);
#7875=EDGE_CURVE('',#6360,#6360,#5545,.T.);
#7876=EDGE_CURVE('',#6359,#6361,#814,.T.);
#7877=EDGE_CURVE('',#6362,#6361,#5546,.T.);
#7878=EDGE_CURVE('',#6362,#6363,#815,.T.);
#7879=EDGE_CURVE('',#6364,#6363,#5547,.T.);
#7880=EDGE_CURVE('',#6364,#6365,#816,.T.);
#7881=EDGE_CURVE('',#6366,#6365,#5548,.T.);
#7882=EDGE_CURVE('',#6366,#6367,#817,.T.);
#7883=EDGE_CURVE('',#6368,#6367,#5549,.T.);
#7884=EDGE_CURVE('',#6368,#6369,#818,.T.);
#7885=EDGE_CURVE('',#6353,#6369,#5550,.T.);
#7886=EDGE_CURVE('',#6350,#6370,#5551,.T.);
#7887=EDGE_CURVE('',#6370,#6354,#5552,.T.);
#7888=EDGE_CURVE('',#6371,#6370,#819,.T.);
#7889=EDGE_CURVE('',#6355,#6371,#5553,.T.);
#7890=EDGE_CURVE('',#6371,#6372,#5554,.T.);
#7891=EDGE_CURVE('',#6372,#6356,#5555,.T.);
#7892=EDGE_CURVE('',#6373,#6372,#820,.T.);
#7893=EDGE_CURVE('',#6357,#6373,#5556,.T.);
#7894=EDGE_CURVE('',#6373,#6374,#5557,.T.);
#7895=EDGE_CURVE('',#6374,#6358,#5558,.T.);
#7896=EDGE_CURVE('',#6375,#6376,#821,.T.);
#7897=EDGE_CURVE('',#6361,#6375,#5559,.T.);
#7898=EDGE_CURVE('',#6376,#6374,#822,.T.);
#7899=EDGE_CURVE('',#6375,#6377,#5560,.T.);
#7900=EDGE_CURVE('',#6377,#6362,#5561,.T.);
#7901=EDGE_CURVE('',#6378,#6377,#823,.T.);
#7902=EDGE_CURVE('',#6363,#6378,#5562,.T.);
#7903=EDGE_CURVE('',#6378,#6379,#5563,.T.);
#7904=EDGE_CURVE('',#6379,#6364,#5564,.T.);
#7905=EDGE_CURVE('',#6380,#6379,#824,.T.);
#7906=EDGE_CURVE('',#6365,#6380,#5565,.T.);
#7907=EDGE_CURVE('',#6380,#6381,#5566,.T.);
#7908=EDGE_CURVE('',#6381,#6366,#5567,.T.);
#7909=EDGE_CURVE('',#6382,#6381,#825,.T.);
#7910=EDGE_CURVE('',#6367,#6382,#5568,.T.);
#7911=EDGE_CURVE('',#6383,#6383,#5569,.T.);
#7912=EDGE_CURVE('',#6383,#6376,#3874,.T.);
#7913=EDGE_CURVE('',#6384,#6351,#5570,.T.);
#7914=EDGE_CURVE('',#6384,#6385,#826,.T.);
#7915=EDGE_CURVE('',#6382,#6385,#5571,.T.);
#7916=EDGE_CURVE('',#6369,#6384,#5572,.T.);
#7917=EDGE_CURVE('',#6385,#6368,#5573,.T.);
#7918=EDGE_CURVE('',#6386,#6386,#5574,.T.);
#7919=EDGE_CURVE('',#6387,#6387,#5575,.T.);
#7920=EDGE_CURVE('',#6388,#6388,#5576,.T.);
#7921=EDGE_CURVE('',#6388,#6386,#3875,.T.);
#7922=EDGE_CURVE('',#6389,#6389,#5577,.T.);
#7923=EDGE_CURVE('',#6389,#6387,#3876,.T.);
#7924=EDGE_CURVE('',#6390,#6390,#5578,.T.);
#7925=EDGE_CURVE('',#6391,#6391,#5579,.T.);
#7926=EDGE_CURVE('',#6392,#6392,#5580,.T.);
#7927=EDGE_CURVE('',#6392,#6390,#3877,.T.);
#7928=EDGE_CURVE('',#6393,#6393,#5581,.T.);
#7929=EDGE_CURVE('',#6393,#6391,#3878,.T.);
#7930=EDGE_CURVE('',#6394,#6394,#5582,.T.);
#7931=EDGE_CURVE('',#6394,#6395,#3879,.T.);
#7932=EDGE_CURVE('',#6395,#6395,#5583,.T.);
#7933=EDGE_CURVE('',#6396,#6397,#3880,.T.);
#7934=EDGE_CURVE('',#6396,#6398,#3881,.T.);
#7935=EDGE_CURVE('',#6399,#6398,#3882,.T.);
#7936=EDGE_CURVE('',#6399,#6397,#3883,.T.);
#7937=EDGE_CURVE('',#6397,#6400,#5584,.T.);
#7938=EDGE_CURVE('',#6401,#6399,#3884,.T.);
#7939=EDGE_CURVE('',#6400,#6401,#3885,.T.);
#7940=EDGE_CURVE('',#6398,#6402,#3886,.T.);
#7941=EDGE_CURVE('',#6401,#6402,#3887,.T.);
#7942=EDGE_CURVE('',#6400,#6403,#3888,.T.);
#7943=EDGE_CURVE('',#6402,#6403,#3889,.T.);
#7944=EDGE_CURVE('',#6403,#6396,#5585,.T.);
#7945=EDGE_CURVE('',#6404,#6404,#5586,.T.);
#7946=EDGE_CURVE('',#6405,#6405,#5587,.T.);
#7947=EDGE_CURVE('',#6406,#6406,#5588,.T.);
#7948=EDGE_CURVE('',#6407,#6407,#5589,.T.);
#7949=EDGE_CURVE('',#6404,#6406,#3890,.T.);
#7950=EDGE_CURVE('',#6407,#6408,#3891,.T.);
#7951=EDGE_CURVE('',#6408,#6408,#5590,.T.);
#7952=EDGE_CURVE('',#6409,#6409,#5591,.T.);
#7953=EDGE_CURVE('',#6409,#6405,#3892,.T.);
#7954=EDGE_CURVE('',#6410,#6410,#5592,.T.);
#7955=EDGE_CURVE('',#6410,#6411,#3893,.T.);
#7956=EDGE_CURVE('',#6411,#6411,#5593,.T.);
#7957=EDGE_CURVE('',#6412,#6412,#5594,.T.);
#7958=EDGE_CURVE('',#6412,#6413,#3894,.T.);
#7959=EDGE_CURVE('',#6413,#6413,#5595,.T.);
#7960=EDGE_CURVE('',#6414,#6414,#5596,.T.);
#7961=EDGE_CURVE('',#6414,#6415,#3895,.T.);
#7962=EDGE_CURVE('',#6415,#6415,#5597,.T.);
#7963=EDGE_CURVE('',#6416,#6416,#5598,.T.);
#7964=EDGE_CURVE('',#6416,#6417,#3896,.T.);
#7965=EDGE_CURVE('',#6417,#6417,#5599,.T.);
#7966=EDGE_CURVE('',#6418,#6418,#5600,.T.);
#7967=EDGE_CURVE('',#6418,#6419,#3897,.T.);
#7968=EDGE_CURVE('',#6419,#6419,#5601,.T.);
#7969=EDGE_CURVE('',#6420,#6420,#5602,.T.);
#7970=EDGE_CURVE('',#6420,#6421,#3898,.T.);
#7971=EDGE_CURVE('',#6421,#6421,#5603,.T.);
#7972=EDGE_CURVE('',#6422,#6423,#3899,.T.);
#7973=EDGE_CURVE('',#6422,#6423,#5604,.T.);
#7974=EDGE_CURVE('',#6424,#6425,#3900,.T.);
#7975=EDGE_CURVE('',#6426,#6424,#5605,.T.);
#7976=EDGE_CURVE('',#6427,#6426,#5606,.T.);
#7977=EDGE_CURVE('',#6428,#6427,#3901,.T.);
#7978=EDGE_CURVE('',#6425,#6428,#5607,.T.);
#7979=EDGE_CURVE('',#6429,#6422,#827,.T.);
#7980=EDGE_CURVE('',#6430,#6429,#5608,.T.);
#7981=EDGE_CURVE('',#6431,#6430,#828,.T.);
#7982=EDGE_CURVE('',#6431,#6426,#3902,.T.);
#7983=EDGE_CURVE('',#6425,#6424,#829,.T.);
#7984=EDGE_CURVE('',#6427,#6428,#830,.T.);
#7985=EDGE_CURVE('',#6423,#6431,#831,.T.);
#7986=EDGE_CURVE('',#6430,#6429,#3903,.T.);
#7987=EDGE_CURVE('',#6432,#6432,#5609,.T.);
#7988=EDGE_CURVE('',#6432,#6433,#3904,.T.);
#7989=EDGE_CURVE('',#6433,#6433,#5610,.T.);
#7990=EDGE_CURVE('',#6434,#6434,#5611,.T.);
#7991=EDGE_CURVE('',#6434,#6435,#3905,.T.);
#7992=EDGE_CURVE('',#6435,#6435,#5612,.T.);
#7993=EDGE_CURVE('',#6436,#6437,#3906,.T.);
#7994=EDGE_CURVE('',#6436,#6438,#3907,.T.);
#7995=EDGE_CURVE('',#6439,#6438,#3908,.T.);
#7996=EDGE_CURVE('',#6437,#6439,#3909,.T.);
#7997=EDGE_CURVE('',#6437,#6440,#3910,.T.);
#7998=EDGE_CURVE('',#6441,#6439,#3911,.T.);
#7999=EDGE_CURVE('',#6440,#6441,#3912,.T.);
#8000=EDGE_CURVE('',#6440,#6442,#3913,.T.);
#8001=EDGE_CURVE('',#6443,#6441,#3914,.T.);
#8002=EDGE_CURVE('',#6442,#6443,#3915,.T.);
#8003=EDGE_CURVE('',#6442,#6436,#3916,.T.);
#8004=EDGE_CURVE('',#6438,#6443,#3917,.T.);
#8005=EDGE_CURVE('',#6444,#6444,#5613,.T.);
#8006=EDGE_CURVE('',#6444,#6445,#3918,.T.);
#8007=EDGE_CURVE('',#6445,#6445,#5614,.T.);
#8008=EDGE_CURVE('',#6446,#6446,#5615,.T.);
#8009=EDGE_CURVE('',#6446,#6447,#3919,.T.);
#8010=EDGE_CURVE('',#6447,#6447,#5616,.T.);
#8011=EDGE_CURVE('',#6448,#6449,#3920,.T.);
#8012=EDGE_CURVE('',#6450,#6448,#3921,.T.);
#8013=EDGE_CURVE('',#6451,#6450,#3922,.T.);
#8014=EDGE_CURVE('',#6449,#6451,#3923,.T.);
#8015=EDGE_CURVE('',#6452,#6448,#3924,.T.);
#8016=EDGE_CURVE('',#6452,#6453,#3925,.T.);
#8017=EDGE_CURVE('',#6450,#6453,#3926,.T.);
#8018=EDGE_CURVE('',#6454,#6452,#3927,.T.);
#8019=EDGE_CURVE('',#6455,#6454,#3928,.T.);
#8020=EDGE_CURVE('',#6453,#6455,#3929,.T.);
#8021=EDGE_CURVE('',#6456,#6457,#5617,.T.);
#8022=EDGE_CURVE('',#6457,#6458,#131,.T.);
#8023=EDGE_CURVE('',#6458,#6459,#3930,.T.);
#8024=EDGE_CURVE('',#6459,#6460,#132,.T.);
#8025=EDGE_CURVE('',#6460,#6461,#5618,.T.);
#8026=EDGE_CURVE('',#6461,#6462,#133,.T.);
#8027=EDGE_CURVE('',#6462,#6463,#3931,.T.);
#8028=EDGE_CURVE('',#6463,#6464,#134,.T.);
#8029=EDGE_CURVE('',#6464,#6465,#5619,.T.);
#8030=EDGE_CURVE('',#6465,#6466,#135,.T.);
#8031=EDGE_CURVE('',#6466,#6467,#3932,.T.);
#8032=EDGE_CURVE('',#6467,#6468,#136,.T.);
#8033=EDGE_CURVE('',#6468,#6469,#5620,.T.);
#8034=EDGE_CURVE('',#6469,#6470,#137,.T.);
#8035=EDGE_CURVE('',#6470,#6471,#3933,.T.);
#8036=EDGE_CURVE('',#6471,#6472,#138,.T.);
#8037=EDGE_CURVE('',#6472,#6473,#5621,.T.);
#8038=EDGE_CURVE('',#6473,#6474,#139,.T.);
#8039=EDGE_CURVE('',#6474,#6475,#3934,.T.);
#8040=EDGE_CURVE('',#6475,#6476,#140,.T.);
#8041=EDGE_CURVE('',#6476,#6477,#5622,.T.);
#8042=EDGE_CURVE('',#6477,#6478,#141,.T.);
#8043=EDGE_CURVE('',#6478,#6479,#3935,.T.);
#8044=EDGE_CURVE('',#6479,#6480,#142,.T.);
#8045=EDGE_CURVE('',#6480,#6481,#5623,.T.);
#8046=EDGE_CURVE('',#6481,#6482,#143,.T.);
#8047=EDGE_CURVE('',#6482,#6483,#3936,.T.);
#8048=EDGE_CURVE('',#6483,#6484,#144,.T.);
#8049=EDGE_CURVE('',#6484,#6485,#5624,.T.);
#8050=EDGE_CURVE('',#6485,#6486,#145,.T.);
#8051=EDGE_CURVE('',#6486,#6487,#3937,.T.);
#8052=EDGE_CURVE('',#6487,#6488,#146,.T.);
#8053=EDGE_CURVE('',#6488,#6489,#5625,.T.);
#8054=EDGE_CURVE('',#6489,#6490,#147,.T.);
#8055=EDGE_CURVE('',#6490,#6491,#3938,.T.);
#8056=EDGE_CURVE('',#6491,#6492,#148,.T.);
#8057=EDGE_CURVE('',#6492,#6493,#5626,.T.);
#8058=EDGE_CURVE('',#6493,#6494,#149,.T.);
#8059=EDGE_CURVE('',#6494,#6495,#3939,.T.);
#8060=EDGE_CURVE('',#6495,#6496,#150,.T.);
#8061=EDGE_CURVE('',#6496,#6497,#5627,.T.);
#8062=EDGE_CURVE('',#6497,#6498,#151,.T.);
#8063=EDGE_CURVE('',#6498,#6499,#3940,.T.);
#8064=EDGE_CURVE('',#6499,#6500,#152,.T.);
#8065=EDGE_CURVE('',#6500,#6501,#5628,.T.);
#8066=EDGE_CURVE('',#6501,#6502,#153,.T.);
#8067=EDGE_CURVE('',#6502,#6503,#3941,.T.);
#8068=EDGE_CURVE('',#6503,#6504,#154,.T.);
#8069=EDGE_CURVE('',#6504,#6505,#5629,.T.);
#8070=EDGE_CURVE('',#6505,#6506,#155,.T.);
#8071=EDGE_CURVE('',#6506,#6507,#3942,.T.);
#8072=EDGE_CURVE('',#6507,#6508,#156,.T.);
#8073=EDGE_CURVE('',#6508,#6509,#5630,.T.);
#8074=EDGE_CURVE('',#6509,#6510,#157,.T.);
#8075=EDGE_CURVE('',#6510,#6511,#3943,.T.);
#8076=EDGE_CURVE('',#6511,#6512,#158,.T.);
#8077=EDGE_CURVE('',#6512,#6513,#5631,.T.);
#8078=EDGE_CURVE('',#6513,#6514,#159,.T.);
#8079=EDGE_CURVE('',#6514,#6515,#3944,.T.);
#8080=EDGE_CURVE('',#6515,#6516,#160,.T.);
#8081=EDGE_CURVE('',#6516,#6517,#5632,.T.);
#8082=EDGE_CURVE('',#6517,#6518,#161,.T.);
#8083=EDGE_CURVE('',#6518,#6519,#3945,.T.);
#8084=EDGE_CURVE('',#6519,#6520,#162,.T.);
#8085=EDGE_CURVE('',#6520,#6521,#5633,.T.);
#8086=EDGE_CURVE('',#6521,#6522,#163,.T.);
#8087=EDGE_CURVE('',#6522,#6523,#3946,.T.);
#8088=EDGE_CURVE('',#6523,#6524,#164,.T.);
#8089=EDGE_CURVE('',#6524,#6525,#5634,.T.);
#8090=EDGE_CURVE('',#6525,#6526,#165,.T.);
#8091=EDGE_CURVE('',#6526,#6527,#3947,.T.);
#8092=EDGE_CURVE('',#6527,#6528,#166,.T.);
#8093=EDGE_CURVE('',#6528,#6529,#5635,.T.);
#8094=EDGE_CURVE('',#6529,#6530,#167,.T.);
#8095=EDGE_CURVE('',#6530,#6531,#3948,.T.);
#8096=EDGE_CURVE('',#6531,#6532,#168,.T.);
#8097=EDGE_CURVE('',#6532,#6533,#5636,.T.);
#8098=EDGE_CURVE('',#6533,#6534,#169,.T.);
#8099=EDGE_CURVE('',#6534,#6535,#3949,.T.);
#8100=EDGE_CURVE('',#6535,#6456,#170,.T.);
#8101=EDGE_CURVE('',#6455,#6451,#5637,.T.);
#8102=EDGE_CURVE('',#6449,#6454,#5638,.T.);
#8103=EDGE_CURVE('',#6536,#6536,#5639,.T.);
#8104=EDGE_CURVE('',#6536,#6537,#3950,.T.);
#8105=EDGE_CURVE('',#6537,#6537,#5640,.T.);
#8106=EDGE_CURVE('',#6538,#6533,#3951,.T.);
#8107=EDGE_CURVE('',#6539,#6538,#171,.T.);
#8108=EDGE_CURVE('',#6534,#6539,#3952,.T.);
#8109=EDGE_CURVE('',#6540,#6539,#3953,.T.);
#8110=EDGE_CURVE('',#6535,#6540,#3954,.T.);
#8111=EDGE_CURVE('',#6541,#6540,#172,.T.);
#8112=EDGE_CURVE('',#6456,#6541,#3955,.T.);
#8113=EDGE_CURVE('',#6542,#6541,#5641,.T.);
#8114=EDGE_CURVE('',#6542,#6457,#3956,.T.);
#8115=EDGE_CURVE('',#6543,#6542,#173,.T.);
#8116=EDGE_CURVE('',#6458,#6543,#3957,.T.);
#8117=EDGE_CURVE('',#6544,#6543,#3958,.T.);
#8118=EDGE_CURVE('',#6459,#6544,#3959,.T.);
#8119=EDGE_CURVE('',#6545,#6544,#174,.T.);
#8120=EDGE_CURVE('',#6460,#6545,#3960,.T.);
#8121=EDGE_CURVE('',#6546,#6545,#5642,.T.);
#8122=EDGE_CURVE('',#6546,#6461,#3961,.T.);
#8123=EDGE_CURVE('',#6547,#6546,#175,.T.);
#8124=EDGE_CURVE('',#6462,#6547,#3962,.T.);
#8125=EDGE_CURVE('',#6548,#6547,#3963,.T.);
#8126=EDGE_CURVE('',#6463,#6548,#3964,.T.);
#8127=EDGE_CURVE('',#6549,#6548,#176,.T.);
#8128=EDGE_CURVE('',#6464,#6549,#3965,.T.);
#8129=EDGE_CURVE('',#6550,#6549,#5643,.T.);
#8130=EDGE_CURVE('',#6550,#6465,#3966,.T.);
#8131=EDGE_CURVE('',#6551,#6550,#177,.T.);
#8132=EDGE_CURVE('',#6466,#6551,#3967,.T.);
#8133=EDGE_CURVE('',#6552,#6551,#3968,.T.);
#8134=EDGE_CURVE('',#6467,#6552,#3969,.T.);
#8135=EDGE_CURVE('',#6553,#6552,#178,.T.);
#8136=EDGE_CURVE('',#6468,#6553,#3970,.T.);
#8137=EDGE_CURVE('',#6554,#6553,#5644,.T.);
#8138=EDGE_CURVE('',#6554,#6469,#3971,.T.);
#8139=EDGE_CURVE('',#6555,#6554,#179,.T.);
#8140=EDGE_CURVE('',#6470,#6555,#3972,.T.);
#8141=EDGE_CURVE('',#6556,#6555,#3973,.T.);
#8142=EDGE_CURVE('',#6471,#6556,#3974,.T.);
#8143=EDGE_CURVE('',#6557,#6556,#180,.T.);
#8144=EDGE_CURVE('',#6472,#6557,#3975,.T.);
#8145=EDGE_CURVE('',#6558,#6557,#5645,.T.);
#8146=EDGE_CURVE('',#6558,#6473,#3976,.T.);
#8147=EDGE_CURVE('',#6559,#6558,#181,.T.);
#8148=EDGE_CURVE('',#6474,#6559,#3977,.T.);
#8149=EDGE_CURVE('',#6560,#6559,#3978,.T.);
#8150=EDGE_CURVE('',#6475,#6560,#3979,.T.);
#8151=EDGE_CURVE('',#6561,#6560,#182,.T.);
#8152=EDGE_CURVE('',#6476,#6561,#3980,.T.);
#8153=EDGE_CURVE('',#6562,#6561,#5646,.T.);
#8154=EDGE_CURVE('',#6562,#6477,#3981,.T.);
#8155=EDGE_CURVE('',#6563,#6562,#183,.T.);
#8156=EDGE_CURVE('',#6478,#6563,#3982,.T.);
#8157=EDGE_CURVE('',#6564,#6563,#3983,.T.);
#8158=EDGE_CURVE('',#6479,#6564,#3984,.T.);
#8159=EDGE_CURVE('',#6565,#6564,#184,.T.);
#8160=EDGE_CURVE('',#6480,#6565,#3985,.T.);
#8161=EDGE_CURVE('',#6566,#6565,#5647,.T.);
#8162=EDGE_CURVE('',#6566,#6481,#3986,.T.);
#8163=EDGE_CURVE('',#6567,#6566,#185,.T.);
#8164=EDGE_CURVE('',#6482,#6567,#3987,.T.);
#8165=EDGE_CURVE('',#6568,#6567,#3988,.T.);
#8166=EDGE_CURVE('',#6483,#6568,#3989,.T.);
#8167=EDGE_CURVE('',#6569,#6568,#186,.T.);
#8168=EDGE_CURVE('',#6484,#6569,#3990,.T.);
#8169=EDGE_CURVE('',#6570,#6569,#5648,.T.);
#8170=EDGE_CURVE('',#6570,#6485,#3991,.T.);
#8171=EDGE_CURVE('',#6571,#6570,#187,.T.);
#8172=EDGE_CURVE('',#6486,#6571,#3992,.T.);
#8173=EDGE_CURVE('',#6572,#6571,#3993,.T.);
#8174=EDGE_CURVE('',#6487,#6572,#3994,.T.);
#8175=EDGE_CURVE('',#6573,#6572,#188,.T.);
#8176=EDGE_CURVE('',#6488,#6573,#3995,.T.);
#8177=EDGE_CURVE('',#6574,#6573,#5649,.T.);
#8178=EDGE_CURVE('',#6574,#6489,#3996,.T.);
#8179=EDGE_CURVE('',#6575,#6574,#189,.T.);
#8180=EDGE_CURVE('',#6490,#6575,#3997,.T.);
#8181=EDGE_CURVE('',#6576,#6575,#3998,.T.);
#8182=EDGE_CURVE('',#6491,#6576,#3999,.T.);
#8183=EDGE_CURVE('',#6577,#6576,#190,.T.);
#8184=EDGE_CURVE('',#6492,#6577,#4000,.T.);
#8185=EDGE_CURVE('',#6578,#6577,#5650,.T.);
#8186=EDGE_CURVE('',#6578,#6493,#4001,.T.);
#8187=EDGE_CURVE('',#6579,#6578,#191,.T.);
#8188=EDGE_CURVE('',#6494,#6579,#4002,.T.);
#8189=EDGE_CURVE('',#6580,#6579,#4003,.T.);
#8190=EDGE_CURVE('',#6495,#6580,#4004,.T.);
#8191=EDGE_CURVE('',#6581,#6580,#192,.T.);
#8192=EDGE_CURVE('',#6496,#6581,#4005,.T.);
#8193=EDGE_CURVE('',#6582,#6581,#5651,.T.);
#8194=EDGE_CURVE('',#6582,#6497,#4006,.T.);
#8195=EDGE_CURVE('',#6583,#6582,#193,.T.);
#8196=EDGE_CURVE('',#6498,#6583,#4007,.T.);
#8197=EDGE_CURVE('',#6584,#6583,#4008,.T.);
#8198=EDGE_CURVE('',#6499,#6584,#4009,.T.);
#8199=EDGE_CURVE('',#6585,#6584,#194,.T.);
#8200=EDGE_CURVE('',#6500,#6585,#4010,.T.);
#8201=EDGE_CURVE('',#6586,#6585,#5652,.T.);
#8202=EDGE_CURVE('',#6586,#6501,#4011,.T.);
#8203=EDGE_CURVE('',#6587,#6586,#195,.T.);
#8204=EDGE_CURVE('',#6502,#6587,#4012,.T.);
#8205=EDGE_CURVE('',#6588,#6587,#4013,.T.);
#8206=EDGE_CURVE('',#6503,#6588,#4014,.T.);
#8207=EDGE_CURVE('',#6589,#6588,#196,.T.);
#8208=EDGE_CURVE('',#6504,#6589,#4015,.T.);
#8209=EDGE_CURVE('',#6590,#6589,#5653,.T.);
#8210=EDGE_CURVE('',#6590,#6505,#4016,.T.);
#8211=EDGE_CURVE('',#6591,#6590,#197,.T.);
#8212=EDGE_CURVE('',#6506,#6591,#4017,.T.);
#8213=EDGE_CURVE('',#6592,#6591,#4018,.T.);
#8214=EDGE_CURVE('',#6507,#6592,#4019,.T.);
#8215=EDGE_CURVE('',#6593,#6592,#198,.T.);
#8216=EDGE_CURVE('',#6508,#6593,#4020,.T.);
#8217=EDGE_CURVE('',#6594,#6593,#5654,.T.);
#8218=EDGE_CURVE('',#6594,#6509,#4021,.T.);
#8219=EDGE_CURVE('',#6595,#6594,#199,.T.);
#8220=EDGE_CURVE('',#6510,#6595,#4022,.T.);
#8221=EDGE_CURVE('',#6596,#6595,#4023,.T.);
#8222=EDGE_CURVE('',#6511,#6596,#4024,.T.);
#8223=EDGE_CURVE('',#6597,#6596,#200,.T.);
#8224=EDGE_CURVE('',#6512,#6597,#4025,.T.);
#8225=EDGE_CURVE('',#6598,#6597,#5655,.T.);
#8226=EDGE_CURVE('',#6598,#6513,#4026,.T.);
#8227=EDGE_CURVE('',#6599,#6598,#201,.T.);
#8228=EDGE_CURVE('',#6514,#6599,#4027,.T.);
#8229=EDGE_CURVE('',#6600,#6599,#4028,.T.);
#8230=EDGE_CURVE('',#6515,#6600,#4029,.T.);
#8231=EDGE_CURVE('',#6601,#6600,#202,.T.);
#8232=EDGE_CURVE('',#6516,#6601,#4030,.T.);
#8233=EDGE_CURVE('',#6602,#6601,#5656,.T.);
#8234=EDGE_CURVE('',#6602,#6517,#4031,.T.);
#8235=EDGE_CURVE('',#6603,#6602,#203,.T.);
#8236=EDGE_CURVE('',#6518,#6603,#4032,.T.);
#8237=EDGE_CURVE('',#6604,#6603,#4033,.T.);
#8238=EDGE_CURVE('',#6519,#6604,#4034,.T.);
#8239=EDGE_CURVE('',#6605,#6604,#204,.T.);
#8240=EDGE_CURVE('',#6520,#6605,#4035,.T.);
#8241=EDGE_CURVE('',#6606,#6605,#5657,.T.);
#8242=EDGE_CURVE('',#6606,#6521,#4036,.T.);
#8243=EDGE_CURVE('',#6607,#6606,#205,.T.);
#8244=EDGE_CURVE('',#6522,#6607,#4037,.T.);
#8245=EDGE_CURVE('',#6608,#6607,#4038,.T.);
#8246=EDGE_CURVE('',#6523,#6608,#4039,.T.);
#8247=EDGE_CURVE('',#6609,#6608,#206,.T.);
#8248=EDGE_CURVE('',#6524,#6609,#4040,.T.);
#8249=EDGE_CURVE('',#6610,#6609,#5658,.T.);
#8250=EDGE_CURVE('',#6610,#6525,#4041,.T.);
#8251=EDGE_CURVE('',#6611,#6610,#207,.T.);
#8252=EDGE_CURVE('',#6526,#6611,#4042,.T.);
#8253=EDGE_CURVE('',#6612,#6611,#4043,.T.);
#8254=EDGE_CURVE('',#6527,#6612,#4044,.T.);
#8255=EDGE_CURVE('',#6613,#6612,#208,.T.);
#8256=EDGE_CURVE('',#6528,#6613,#4045,.T.);
#8257=EDGE_CURVE('',#6614,#6613,#5659,.T.);
#8258=EDGE_CURVE('',#6614,#6529,#4046,.T.);
#8259=EDGE_CURVE('',#6615,#6614,#209,.T.);
#8260=EDGE_CURVE('',#6530,#6615,#4047,.T.);
#8261=EDGE_CURVE('',#6616,#6615,#4048,.T.);
#8262=EDGE_CURVE('',#6531,#6616,#4049,.T.);
#8263=EDGE_CURVE('',#6617,#6616,#210,.T.);
#8264=EDGE_CURVE('',#6532,#6617,#4050,.T.);
#8265=EDGE_CURVE('',#6538,#6617,#5660,.T.);
#8266=EDGE_CURVE('',#6618,#6618,#5661,.T.);
#8267=EDGE_CURVE('',#6618,#6619,#4051,.T.);
#8268=EDGE_CURVE('',#6619,#6619,#5662,.T.);
#8269=EDGE_CURVE('',#6620,#6621,#4052,.T.);
#8270=EDGE_CURVE('',#6620,#6622,#4053,.T.);
#8271=EDGE_CURVE('',#6623,#6622,#4054,.T.);
#8272=EDGE_CURVE('',#6623,#6621,#4055,.T.);
#8273=EDGE_CURVE('',#6621,#6624,#5663,.T.);
#8274=EDGE_CURVE('',#6625,#6623,#4056,.T.);
#8275=EDGE_CURVE('',#6624,#6625,#4057,.T.);
#8276=EDGE_CURVE('',#6622,#6626,#4058,.T.);
#8277=EDGE_CURVE('',#6625,#6626,#4059,.T.);
#8278=EDGE_CURVE('',#6624,#6627,#4060,.T.);
#8279=EDGE_CURVE('',#6626,#6627,#4061,.T.);
#8280=EDGE_CURVE('',#6627,#6620,#5664,.T.);
#8281=EDGE_CURVE('',#6628,#6628,#5665,.T.);
#8282=EDGE_CURVE('',#6629,#6629,#5666,.T.);
#8283=EDGE_CURVE('',#6630,#6630,#5667,.T.);
#8284=EDGE_CURVE('',#6631,#6631,#5668,.T.);
#8285=EDGE_CURVE('',#6628,#6630,#4062,.T.);
#8286=EDGE_CURVE('',#6631,#6632,#4063,.T.);
#8287=EDGE_CURVE('',#6632,#6632,#5669,.T.);
#8288=EDGE_CURVE('',#6633,#6633,#5670,.T.);
#8289=EDGE_CURVE('',#6633,#6629,#4064,.T.);
#8290=EDGE_CURVE('',#6634,#6634,#5671,.T.);
#8291=EDGE_CURVE('',#6634,#6635,#4065,.T.);
#8292=EDGE_CURVE('',#6635,#6635,#5672,.T.);
#8293=EDGE_CURVE('',#6636,#6636,#5673,.T.);
#8294=EDGE_CURVE('',#6636,#6637,#4066,.T.);
#8295=EDGE_CURVE('',#6637,#6637,#5674,.T.);
#8296=EDGE_CURVE('',#6638,#6638,#5675,.T.);
#8297=EDGE_CURVE('',#6638,#6639,#4067,.T.);
#8298=EDGE_CURVE('',#6639,#6639,#5676,.T.);
#8299=EDGE_CURVE('',#6640,#6640,#5677,.T.);
#8300=EDGE_CURVE('',#6640,#6641,#4068,.T.);
#8301=EDGE_CURVE('',#6641,#6641,#5678,.T.);
#8302=EDGE_CURVE('',#6642,#6643,#832,.T.);
#8303=EDGE_CURVE('',#6643,#6642,#833,.T.);
#8304=EDGE_CURVE('',#6643,#6644,#4069,.T.);
#8305=EDGE_CURVE('',#6645,#6644,#834,.T.);
#8306=EDGE_CURVE('',#6644,#6645,#835,.T.);
#8307=EDGE_CURVE('',#6646,#6646,#5679,.T.);
#8308=EDGE_CURVE('',#6646,#6647,#4070,.T.);
#8309=EDGE_CURVE('',#6647,#6647,#5680,.T.);
#8310=EDGE_CURVE('',#6648,#6648,#5681,.T.);
#8311=EDGE_CURVE('',#6648,#6649,#4071,.T.);
#8312=EDGE_CURVE('',#6649,#6649,#5682,.T.);
#8313=EDGE_CURVE('',#6650,#6651,#4072,.T.);
#8314=EDGE_CURVE('',#6650,#6652,#4073,.T.);
#8315=EDGE_CURVE('',#6653,#6652,#4074,.T.);
#8316=EDGE_CURVE('',#6651,#6653,#4075,.T.);
#8317=EDGE_CURVE('',#6651,#6654,#4076,.T.);
#8318=EDGE_CURVE('',#6655,#6653,#4077,.T.);
#8319=EDGE_CURVE('',#6654,#6655,#4078,.T.);
#8320=EDGE_CURVE('',#6654,#6656,#4079,.T.);
#8321=EDGE_CURVE('',#6657,#6655,#4080,.T.);
#8322=EDGE_CURVE('',#6656,#6657,#4081,.T.);
#8323=EDGE_CURVE('',#6656,#6650,#4082,.T.);
#8324=EDGE_CURVE('',#6652,#6657,#4083,.T.);
#8325=EDGE_CURVE('',#6658,#6658,#5683,.T.);
#8326=EDGE_CURVE('',#6658,#6659,#4084,.T.);
#8327=EDGE_CURVE('',#6659,#6659,#5684,.T.);
#8328=EDGE_CURVE('',#6660,#6660,#5685,.T.);
#8329=EDGE_CURVE('',#6660,#6661,#4085,.T.);
#8330=EDGE_CURVE('',#6661,#6661,#5686,.T.);
#8331=EDGE_CURVE('',#6662,#6662,#5687,.T.);
#8332=EDGE_CURVE('',#6663,#6664,#4086,.T.);
#8333=EDGE_CURVE('',#6663,#6665,#4087,.T.);
#8334=EDGE_CURVE('',#6665,#6666,#4088,.T.);
#8335=EDGE_CURVE('',#6664,#6666,#4089,.T.);
#8336=EDGE_CURVE('',#6667,#6663,#4090,.T.);
#8337=EDGE_CURVE('',#6667,#6668,#4091,.T.);
#8338=EDGE_CURVE('',#6668,#6665,#4092,.T.);
#8339=EDGE_CURVE('',#6669,#6667,#4093,.T.);
#8340=EDGE_CURVE('',#6669,#6670,#4094,.T.);
#8341=EDGE_CURVE('',#6670,#6668,#4095,.T.);
#8342=EDGE_CURVE('',#6671,#6669,#4096,.T.);
#8343=EDGE_CURVE('',#6671,#6672,#4097,.T.);
#8344=EDGE_CURVE('',#6672,#6670,#4098,.T.);
#8345=EDGE_CURVE('',#6673,#6671,#4099,.T.);
#8346=EDGE_CURVE('',#6673,#6674,#4100,.T.);
#8347=EDGE_CURVE('',#6674,#6672,#4101,.T.);
#8348=EDGE_CURVE('',#6664,#6673,#4102,.T.);
#8349=EDGE_CURVE('',#6666,#6674,#4103,.T.);
#8350=EDGE_CURVE('',#6675,#6675,#5688,.T.);
#8351=EDGE_CURVE('',#6676,#6676,#5689,.T.);
#8352=EDGE_CURVE('',#6676,#6675,#4104,.T.);
#8353=EDGE_CURVE('',#6662,#6676,#4105,.T.);
#8354=EDGE_CURVE('',#6677,#6678,#4106,.T.);
#8355=EDGE_CURVE('',#6679,#6677,#4107,.T.);
#8356=EDGE_CURVE('',#6680,#6679,#4108,.T.);
#8357=EDGE_CURVE('',#6678,#6680,#4109,.T.);
#8358=EDGE_CURVE('',#6681,#6677,#4110,.T.);
#8359=EDGE_CURVE('',#6681,#6682,#4111,.T.);
#8360=EDGE_CURVE('',#6679,#6682,#4112,.T.);
#8361=EDGE_CURVE('',#6683,#6681,#4113,.T.);
#8362=EDGE_CURVE('',#6684,#6683,#4114,.T.);
#8363=EDGE_CURVE('',#6682,#6684,#4115,.T.);
#8364=EDGE_CURVE('',#6685,#6686,#5690,.T.);
#8365=EDGE_CURVE('',#6686,#6687,#211,.T.);
#8366=EDGE_CURVE('',#6687,#6688,#4116,.T.);
#8367=EDGE_CURVE('',#6688,#6689,#212,.T.);
#8368=EDGE_CURVE('',#6689,#6690,#5691,.T.);
#8369=EDGE_CURVE('',#6690,#6691,#213,.T.);
#8370=EDGE_CURVE('',#6691,#6692,#4117,.T.);
#8371=EDGE_CURVE('',#6692,#6693,#214,.T.);
#8372=EDGE_CURVE('',#6693,#6694,#5692,.T.);
#8373=EDGE_CURVE('',#6694,#6695,#215,.T.);
#8374=EDGE_CURVE('',#6695,#6696,#4118,.T.);
#8375=EDGE_CURVE('',#6696,#6697,#216,.T.);
#8376=EDGE_CURVE('',#6697,#6698,#5693,.T.);
#8377=EDGE_CURVE('',#6698,#6699,#217,.T.);
#8378=EDGE_CURVE('',#6699,#6700,#4119,.T.);
#8379=EDGE_CURVE('',#6700,#6701,#218,.T.);
#8380=EDGE_CURVE('',#6701,#6702,#5694,.T.);
#8381=EDGE_CURVE('',#6702,#6703,#219,.T.);
#8382=EDGE_CURVE('',#6703,#6704,#4120,.T.);
#8383=EDGE_CURVE('',#6704,#6705,#220,.T.);
#8384=EDGE_CURVE('',#6705,#6706,#5695,.T.);
#8385=EDGE_CURVE('',#6706,#6707,#221,.T.);
#8386=EDGE_CURVE('',#6707,#6708,#4121,.T.);
#8387=EDGE_CURVE('',#6708,#6709,#222,.T.);
#8388=EDGE_CURVE('',#6709,#6710,#5696,.T.);
#8389=EDGE_CURVE('',#6710,#6711,#223,.T.);
#8390=EDGE_CURVE('',#6711,#6712,#4122,.T.);
#8391=EDGE_CURVE('',#6712,#6713,#224,.T.);
#8392=EDGE_CURVE('',#6713,#6714,#5697,.T.);
#8393=EDGE_CURVE('',#6714,#6715,#225,.T.);
#8394=EDGE_CURVE('',#6715,#6716,#4123,.T.);
#8395=EDGE_CURVE('',#6716,#6717,#226,.T.);
#8396=EDGE_CURVE('',#6717,#6718,#5698,.T.);
#8397=EDGE_CURVE('',#6718,#6719,#227,.T.);
#8398=EDGE_CURVE('',#6719,#6720,#4124,.T.);
#8399=EDGE_CURVE('',#6720,#6721,#228,.T.);
#8400=EDGE_CURVE('',#6721,#6722,#5699,.T.);
#8401=EDGE_CURVE('',#6722,#6723,#229,.T.);
#8402=EDGE_CURVE('',#6723,#6724,#4125,.T.);
#8403=EDGE_CURVE('',#6724,#6725,#230,.T.);
#8404=EDGE_CURVE('',#6725,#6726,#5700,.T.);
#8405=EDGE_CURVE('',#6726,#6727,#231,.T.);
#8406=EDGE_CURVE('',#6727,#6728,#4126,.T.);
#8407=EDGE_CURVE('',#6728,#6729,#232,.T.);
#8408=EDGE_CURVE('',#6729,#6730,#5701,.T.);
#8409=EDGE_CURVE('',#6730,#6731,#233,.T.);
#8410=EDGE_CURVE('',#6731,#6732,#4127,.T.);
#8411=EDGE_CURVE('',#6732,#6733,#234,.T.);
#8412=EDGE_CURVE('',#6733,#6734,#5702,.T.);
#8413=EDGE_CURVE('',#6734,#6735,#235,.T.);
#8414=EDGE_CURVE('',#6735,#6736,#4128,.T.);
#8415=EDGE_CURVE('',#6736,#6737,#236,.T.);
#8416=EDGE_CURVE('',#6737,#6738,#5703,.T.);
#8417=EDGE_CURVE('',#6738,#6739,#237,.T.);
#8418=EDGE_CURVE('',#6739,#6740,#4129,.T.);
#8419=EDGE_CURVE('',#6740,#6741,#238,.T.);
#8420=EDGE_CURVE('',#6741,#6742,#5704,.T.);
#8421=EDGE_CURVE('',#6742,#6743,#239,.T.);
#8422=EDGE_CURVE('',#6743,#6744,#4130,.T.);
#8423=EDGE_CURVE('',#6744,#6745,#240,.T.);
#8424=EDGE_CURVE('',#6745,#6746,#5705,.T.);
#8425=EDGE_CURVE('',#6746,#6747,#241,.T.);
#8426=EDGE_CURVE('',#6747,#6748,#4131,.T.);
#8427=EDGE_CURVE('',#6748,#6749,#242,.T.);
#8428=EDGE_CURVE('',#6749,#6750,#5706,.T.);
#8429=EDGE_CURVE('',#6750,#6751,#243,.T.);
#8430=EDGE_CURVE('',#6751,#6752,#4132,.T.);
#8431=EDGE_CURVE('',#6752,#6753,#244,.T.);
#8432=EDGE_CURVE('',#6753,#6754,#5707,.T.);
#8433=EDGE_CURVE('',#6754,#6755,#245,.T.);
#8434=EDGE_CURVE('',#6755,#6756,#4133,.T.);
#8435=EDGE_CURVE('',#6756,#6757,#246,.T.);
#8436=EDGE_CURVE('',#6757,#6758,#5708,.T.);
#8437=EDGE_CURVE('',#6758,#6759,#247,.T.);
#8438=EDGE_CURVE('',#6759,#6760,#4134,.T.);
#8439=EDGE_CURVE('',#6760,#6761,#248,.T.);
#8440=EDGE_CURVE('',#6761,#6762,#5709,.T.);
#8441=EDGE_CURVE('',#6762,#6763,#249,.T.);
#8442=EDGE_CURVE('',#6763,#6764,#4135,.T.);
#8443=EDGE_CURVE('',#6764,#6765,#250,.T.);
#8444=EDGE_CURVE('',#6765,#6766,#5710,.T.);
#8445=EDGE_CURVE('',#6766,#6767,#251,.T.);
#8446=EDGE_CURVE('',#6767,#6768,#4136,.T.);
#8447=EDGE_CURVE('',#6768,#6769,#252,.T.);
#8448=EDGE_CURVE('',#6769,#6770,#5711,.T.);
#8449=EDGE_CURVE('',#6770,#6771,#253,.T.);
#8450=EDGE_CURVE('',#6771,#6772,#4137,.T.);
#8451=EDGE_CURVE('',#6772,#6773,#254,.T.);
#8452=EDGE_CURVE('',#6773,#6774,#5712,.T.);
#8453=EDGE_CURVE('',#6774,#6775,#255,.T.);
#8454=EDGE_CURVE('',#6775,#6776,#4138,.T.);
#8455=EDGE_CURVE('',#6776,#6777,#256,.T.);
#8456=EDGE_CURVE('',#6777,#6778,#5713,.T.);
#8457=EDGE_CURVE('',#6778,#6779,#257,.T.);
#8458=EDGE_CURVE('',#6779,#6780,#4139,.T.);
#8459=EDGE_CURVE('',#6780,#6781,#258,.T.);
#8460=EDGE_CURVE('',#6781,#6782,#5714,.T.);
#8461=EDGE_CURVE('',#6782,#6783,#259,.T.);
#8462=EDGE_CURVE('',#6783,#6784,#4140,.T.);
#8463=EDGE_CURVE('',#6784,#6785,#260,.T.);
#8464=EDGE_CURVE('',#6785,#6786,#5715,.T.);
#8465=EDGE_CURVE('',#6786,#6787,#261,.T.);
#8466=EDGE_CURVE('',#6787,#6788,#4141,.T.);
#8467=EDGE_CURVE('',#6788,#6789,#262,.T.);
#8468=EDGE_CURVE('',#6789,#6790,#5716,.T.);
#8469=EDGE_CURVE('',#6790,#6791,#263,.T.);
#8470=EDGE_CURVE('',#6791,#6792,#4142,.T.);
#8471=EDGE_CURVE('',#6792,#6793,#264,.T.);
#8472=EDGE_CURVE('',#6793,#6794,#5717,.T.);
#8473=EDGE_CURVE('',#6794,#6795,#265,.T.);
#8474=EDGE_CURVE('',#6795,#6796,#4143,.T.);
#8475=EDGE_CURVE('',#6796,#6797,#266,.T.);
#8476=EDGE_CURVE('',#6797,#6798,#5718,.T.);
#8477=EDGE_CURVE('',#6798,#6799,#267,.T.);
#8478=EDGE_CURVE('',#6799,#6800,#4144,.T.);
#8479=EDGE_CURVE('',#6800,#6801,#268,.T.);
#8480=EDGE_CURVE('',#6801,#6802,#5719,.T.);
#8481=EDGE_CURVE('',#6802,#6803,#269,.T.);
#8482=EDGE_CURVE('',#6803,#6804,#4145,.T.);
#8483=EDGE_CURVE('',#6804,#6805,#270,.T.);
#8484=EDGE_CURVE('',#6805,#6806,#5720,.T.);
#8485=EDGE_CURVE('',#6806,#6807,#271,.T.);
#8486=EDGE_CURVE('',#6807,#6808,#4146,.T.);
#8487=EDGE_CURVE('',#6808,#6809,#272,.T.);
#8488=EDGE_CURVE('',#6809,#6810,#5721,.T.);
#8489=EDGE_CURVE('',#6810,#6811,#273,.T.);
#8490=EDGE_CURVE('',#6811,#6812,#4147,.T.);
#8491=EDGE_CURVE('',#6812,#6813,#274,.T.);
#8492=EDGE_CURVE('',#6813,#6814,#5722,.T.);
#8493=EDGE_CURVE('',#6814,#6815,#275,.T.);
#8494=EDGE_CURVE('',#6815,#6816,#4148,.T.);
#8495=EDGE_CURVE('',#6816,#6817,#276,.T.);
#8496=EDGE_CURVE('',#6817,#6818,#5723,.T.);
#8497=EDGE_CURVE('',#6818,#6819,#277,.T.);
#8498=EDGE_CURVE('',#6819,#6820,#4149,.T.);
#8499=EDGE_CURVE('',#6820,#6821,#278,.T.);
#8500=EDGE_CURVE('',#6821,#6822,#5724,.T.);
#8501=EDGE_CURVE('',#6822,#6823,#279,.T.);
#8502=EDGE_CURVE('',#6823,#6824,#4150,.T.);
#8503=EDGE_CURVE('',#6824,#6825,#280,.T.);
#8504=EDGE_CURVE('',#6825,#6826,#5725,.T.);
#8505=EDGE_CURVE('',#6826,#6827,#281,.T.);
#8506=EDGE_CURVE('',#6827,#6828,#4151,.T.);
#8507=EDGE_CURVE('',#6828,#6829,#282,.T.);
#8508=EDGE_CURVE('',#6829,#6830,#5726,.T.);
#8509=EDGE_CURVE('',#6830,#6831,#283,.T.);
#8510=EDGE_CURVE('',#6831,#6832,#4152,.T.);
#8511=EDGE_CURVE('',#6832,#6833,#284,.T.);
#8512=EDGE_CURVE('',#6833,#6834,#5727,.T.);
#8513=EDGE_CURVE('',#6834,#6835,#285,.T.);
#8514=EDGE_CURVE('',#6835,#6836,#4153,.T.);
#8515=EDGE_CURVE('',#6836,#6837,#286,.T.);
#8516=EDGE_CURVE('',#6837,#6838,#5728,.T.);
#8517=EDGE_CURVE('',#6838,#6839,#287,.T.);
#8518=EDGE_CURVE('',#6839,#6840,#4154,.T.);
#8519=EDGE_CURVE('',#6840,#6841,#288,.T.);
#8520=EDGE_CURVE('',#6841,#6842,#5729,.T.);
#8521=EDGE_CURVE('',#6842,#6843,#289,.T.);
#8522=EDGE_CURVE('',#6843,#6844,#4155,.T.);
#8523=EDGE_CURVE('',#6844,#6685,#290,.T.);
#8524=EDGE_CURVE('',#6684,#6680,#5730,.T.);
#8525=EDGE_CURVE('',#6678,#6683,#5731,.T.);
#8526=EDGE_CURVE('',#6845,#6845,#5732,.T.);
#8527=EDGE_CURVE('',#6845,#6846,#4156,.T.);
#8528=EDGE_CURVE('',#6846,#6846,#5733,.T.);
#8529=EDGE_CURVE('',#6847,#6842,#836,.T.);
#8530=EDGE_CURVE('',#6848,#6847,#291,.T.);
#8531=EDGE_CURVE('',#6843,#6848,#4157,.T.);
#8532=EDGE_CURVE('',#6685,#6849,#837,.T.);
#8533=EDGE_CURVE('',#6844,#6850,#4158,.T.);
#8534=EDGE_CURVE('',#6849,#6850,#292,.T.);
#8535=EDGE_CURVE('',#6850,#6848,#4159,.T.);
#8536=EDGE_CURVE('',#6851,#6849,#5734,.T.);
#8537=EDGE_CURVE('',#6851,#6686,#838,.T.);
#8538=EDGE_CURVE('',#6852,#6851,#293,.T.);
#8539=EDGE_CURVE('',#6687,#6852,#4160,.T.);
#8540=EDGE_CURVE('',#6689,#6853,#839,.T.);
#8541=EDGE_CURVE('',#6688,#6854,#4161,.T.);
#8542=EDGE_CURVE('',#6853,#6854,#294,.T.);
#8543=EDGE_CURVE('',#6854,#6852,#4162,.T.);
#8544=EDGE_CURVE('',#6855,#6853,#5735,.T.);
#8545=EDGE_CURVE('',#6855,#6690,#840,.T.);
#8546=EDGE_CURVE('',#6856,#6855,#295,.T.);
#8547=EDGE_CURVE('',#6691,#6856,#4163,.T.);
#8548=EDGE_CURVE('',#6693,#6857,#841,.T.);
#8549=EDGE_CURVE('',#6692,#6858,#4164,.T.);
#8550=EDGE_CURVE('',#6857,#6858,#296,.T.);
#8551=EDGE_CURVE('',#6858,#6856,#4165,.T.);
#8552=EDGE_CURVE('',#6859,#6857,#5736,.T.);
#8553=EDGE_CURVE('',#6859,#6694,#842,.T.);
#8554=EDGE_CURVE('',#6860,#6859,#297,.T.);
#8555=EDGE_CURVE('',#6695,#6860,#4166,.T.);
#8556=EDGE_CURVE('',#6697,#6861,#843,.T.);
#8557=EDGE_CURVE('',#6696,#6862,#4167,.T.);
#8558=EDGE_CURVE('',#6861,#6862,#298,.T.);
#8559=EDGE_CURVE('',#6862,#6860,#4168,.T.);
#8560=EDGE_CURVE('',#6863,#6861,#5737,.T.);
#8561=EDGE_CURVE('',#6863,#6698,#844,.T.);
#8562=EDGE_CURVE('',#6864,#6863,#299,.T.);
#8563=EDGE_CURVE('',#6699,#6864,#4169,.T.);
#8564=EDGE_CURVE('',#6701,#6865,#845,.T.);
#8565=EDGE_CURVE('',#6700,#6866,#4170,.T.);
#8566=EDGE_CURVE('',#6865,#6866,#300,.T.);
#8567=EDGE_CURVE('',#6866,#6864,#4171,.T.);
#8568=EDGE_CURVE('',#6867,#6865,#5738,.T.);
#8569=EDGE_CURVE('',#6867,#6702,#846,.T.);
#8570=EDGE_CURVE('',#6868,#6867,#301,.T.);
#8571=EDGE_CURVE('',#6703,#6868,#4172,.T.);
#8572=EDGE_CURVE('',#6705,#6869,#847,.T.);
#8573=EDGE_CURVE('',#6704,#6870,#4173,.T.);
#8574=EDGE_CURVE('',#6869,#6870,#302,.T.);
#8575=EDGE_CURVE('',#6870,#6868,#4174,.T.);
#8576=EDGE_CURVE('',#6871,#6869,#5739,.T.);
#8577=EDGE_CURVE('',#6871,#6706,#848,.T.);
#8578=EDGE_CURVE('',#6872,#6871,#303,.T.);
#8579=EDGE_CURVE('',#6707,#6872,#4175,.T.);
#8580=EDGE_CURVE('',#6709,#6873,#849,.T.);
#8581=EDGE_CURVE('',#6708,#6874,#4176,.T.);
#8582=EDGE_CURVE('',#6873,#6874,#304,.T.);
#8583=EDGE_CURVE('',#6874,#6872,#4177,.T.);
#8584=EDGE_CURVE('',#6875,#6873,#5740,.T.);
#8585=EDGE_CURVE('',#6875,#6710,#850,.T.);
#8586=EDGE_CURVE('',#6876,#6875,#305,.T.);
#8587=EDGE_CURVE('',#6711,#6876,#4178,.T.);
#8588=EDGE_CURVE('',#6713,#6877,#851,.T.);
#8589=EDGE_CURVE('',#6712,#6878,#4179,.T.);
#8590=EDGE_CURVE('',#6877,#6878,#306,.T.);
#8591=EDGE_CURVE('',#6878,#6876,#4180,.T.);
#8592=EDGE_CURVE('',#6879,#6877,#5741,.T.);
#8593=EDGE_CURVE('',#6879,#6714,#852,.T.);
#8594=EDGE_CURVE('',#6880,#6879,#307,.T.);
#8595=EDGE_CURVE('',#6715,#6880,#4181,.T.);
#8596=EDGE_CURVE('',#6717,#6881,#853,.T.);
#8597=EDGE_CURVE('',#6716,#6882,#4182,.T.);
#8598=EDGE_CURVE('',#6881,#6882,#308,.T.);
#8599=EDGE_CURVE('',#6882,#6880,#4183,.T.);
#8600=EDGE_CURVE('',#6883,#6881,#5742,.T.);
#8601=EDGE_CURVE('',#6883,#6718,#854,.T.);
#8602=EDGE_CURVE('',#6884,#6883,#309,.T.);
#8603=EDGE_CURVE('',#6719,#6884,#4184,.T.);
#8604=EDGE_CURVE('',#6721,#6885,#855,.T.);
#8605=EDGE_CURVE('',#6720,#6886,#4185,.T.);
#8606=EDGE_CURVE('',#6885,#6886,#310,.T.);
#8607=EDGE_CURVE('',#6886,#6884,#4186,.T.);
#8608=EDGE_CURVE('',#6887,#6885,#5743,.T.);
#8609=EDGE_CURVE('',#6887,#6722,#856,.T.);
#8610=EDGE_CURVE('',#6888,#6887,#311,.T.);
#8611=EDGE_CURVE('',#6723,#6888,#4187,.T.);
#8612=EDGE_CURVE('',#6725,#6889,#857,.T.);
#8613=EDGE_CURVE('',#6724,#6890,#4188,.T.);
#8614=EDGE_CURVE('',#6889,#6890,#312,.T.);
#8615=EDGE_CURVE('',#6890,#6888,#4189,.T.);
#8616=EDGE_CURVE('',#6891,#6889,#5744,.T.);
#8617=EDGE_CURVE('',#6891,#6726,#858,.T.);
#8618=EDGE_CURVE('',#6892,#6891,#313,.T.);
#8619=EDGE_CURVE('',#6727,#6892,#4190,.T.);
#8620=EDGE_CURVE('',#6729,#6893,#859,.T.);
#8621=EDGE_CURVE('',#6728,#6894,#4191,.T.);
#8622=EDGE_CURVE('',#6893,#6894,#314,.T.);
#8623=EDGE_CURVE('',#6894,#6892,#4192,.T.);
#8624=EDGE_CURVE('',#6895,#6893,#5745,.T.);
#8625=EDGE_CURVE('',#6895,#6730,#860,.T.);
#8626=EDGE_CURVE('',#6896,#6895,#315,.T.);
#8627=EDGE_CURVE('',#6731,#6896,#4193,.T.);
#8628=EDGE_CURVE('',#6733,#6897,#861,.T.);
#8629=EDGE_CURVE('',#6732,#6898,#4194,.T.);
#8630=EDGE_CURVE('',#6897,#6898,#316,.T.);
#8631=EDGE_CURVE('',#6898,#6896,#4195,.T.);
#8632=EDGE_CURVE('',#6899,#6897,#5746,.T.);
#8633=EDGE_CURVE('',#6899,#6734,#862,.T.);
#8634=EDGE_CURVE('',#6900,#6899,#317,.T.);
#8635=EDGE_CURVE('',#6735,#6900,#4196,.T.);
#8636=EDGE_CURVE('',#6737,#6901,#863,.T.);
#8637=EDGE_CURVE('',#6736,#6902,#4197,.T.);
#8638=EDGE_CURVE('',#6901,#6902,#318,.T.);
#8639=EDGE_CURVE('',#6902,#6900,#4198,.T.);
#8640=EDGE_CURVE('',#6903,#6901,#5747,.T.);
#8641=EDGE_CURVE('',#6903,#6738,#864,.T.);
#8642=EDGE_CURVE('',#6904,#6903,#319,.T.);
#8643=EDGE_CURVE('',#6739,#6904,#4199,.T.);
#8644=EDGE_CURVE('',#6741,#6905,#865,.T.);
#8645=EDGE_CURVE('',#6740,#6906,#4200,.T.);
#8646=EDGE_CURVE('',#6905,#6906,#320,.T.);
#8647=EDGE_CURVE('',#6906,#6904,#4201,.T.);
#8648=EDGE_CURVE('',#6907,#6905,#5748,.T.);
#8649=EDGE_CURVE('',#6907,#6742,#866,.T.);
#8650=EDGE_CURVE('',#6908,#6907,#321,.T.);
#8651=EDGE_CURVE('',#6743,#6908,#4202,.T.);
#8652=EDGE_CURVE('',#6745,#6909,#867,.T.);
#8653=EDGE_CURVE('',#6744,#6910,#4203,.T.);
#8654=EDGE_CURVE('',#6909,#6910,#322,.T.);
#8655=EDGE_CURVE('',#6910,#6908,#4204,.T.);
#8656=EDGE_CURVE('',#6911,#6909,#5749,.T.);
#8657=EDGE_CURVE('',#6911,#6746,#868,.T.);
#8658=EDGE_CURVE('',#6912,#6911,#323,.T.);
#8659=EDGE_CURVE('',#6747,#6912,#4205,.T.);
#8660=EDGE_CURVE('',#6749,#6913,#869,.T.);
#8661=EDGE_CURVE('',#6748,#6914,#4206,.T.);
#8662=EDGE_CURVE('',#6913,#6914,#324,.T.);
#8663=EDGE_CURVE('',#6914,#6912,#4207,.T.);
#8664=EDGE_CURVE('',#6915,#6913,#5750,.T.);
#8665=EDGE_CURVE('',#6915,#6750,#870,.T.);
#8666=EDGE_CURVE('',#6916,#6915,#325,.T.);
#8667=EDGE_CURVE('',#6751,#6916,#4208,.T.);
#8668=EDGE_CURVE('',#6753,#6917,#871,.T.);
#8669=EDGE_CURVE('',#6752,#6918,#4209,.T.);
#8670=EDGE_CURVE('',#6917,#6918,#326,.T.);
#8671=EDGE_CURVE('',#6918,#6916,#4210,.T.);
#8672=EDGE_CURVE('',#6919,#6917,#5751,.T.);
#8673=EDGE_CURVE('',#6919,#6754,#872,.T.);
#8674=EDGE_CURVE('',#6920,#6919,#327,.T.);
#8675=EDGE_CURVE('',#6755,#6920,#4211,.T.);
#8676=EDGE_CURVE('',#6757,#6921,#873,.T.);
#8677=EDGE_CURVE('',#6756,#6922,#4212,.T.);
#8678=EDGE_CURVE('',#6921,#6922,#328,.T.);
#8679=EDGE_CURVE('',#6922,#6920,#4213,.T.);
#8680=EDGE_CURVE('',#6923,#6921,#5752,.T.);
#8681=EDGE_CURVE('',#6923,#6758,#874,.T.);
#8682=EDGE_CURVE('',#6924,#6923,#329,.T.);
#8683=EDGE_CURVE('',#6759,#6924,#4214,.T.);
#8684=EDGE_CURVE('',#6761,#6925,#875,.T.);
#8685=EDGE_CURVE('',#6760,#6926,#4215,.T.);
#8686=EDGE_CURVE('',#6925,#6926,#330,.T.);
#8687=EDGE_CURVE('',#6926,#6924,#4216,.T.);
#8688=EDGE_CURVE('',#6927,#6925,#5753,.T.);
#8689=EDGE_CURVE('',#6927,#6762,#876,.T.);
#8690=EDGE_CURVE('',#6928,#6927,#331,.T.);
#8691=EDGE_CURVE('',#6763,#6928,#4217,.T.);
#8692=EDGE_CURVE('',#6765,#6929,#877,.T.);
#8693=EDGE_CURVE('',#6764,#6930,#4218,.T.);
#8694=EDGE_CURVE('',#6929,#6930,#332,.T.);
#8695=EDGE_CURVE('',#6930,#6928,#4219,.T.);
#8696=EDGE_CURVE('',#6931,#6929,#5754,.T.);
#8697=EDGE_CURVE('',#6931,#6766,#878,.T.);
#8698=EDGE_CURVE('',#6932,#6931,#333,.T.);
#8699=EDGE_CURVE('',#6767,#6932,#4220,.T.);
#8700=EDGE_CURVE('',#6769,#6933,#879,.T.);
#8701=EDGE_CURVE('',#6768,#6934,#4221,.T.);
#8702=EDGE_CURVE('',#6933,#6934,#334,.T.);
#8703=EDGE_CURVE('',#6934,#6932,#4222,.T.);
#8704=EDGE_CURVE('',#6935,#6933,#5755,.T.);
#8705=EDGE_CURVE('',#6935,#6770,#880,.T.);
#8706=EDGE_CURVE('',#6936,#6935,#335,.T.);
#8707=EDGE_CURVE('',#6771,#6936,#4223,.T.);
#8708=EDGE_CURVE('',#6773,#6937,#881,.T.);
#8709=EDGE_CURVE('',#6772,#6938,#4224,.T.);
#8710=EDGE_CURVE('',#6937,#6938,#336,.T.);
#8711=EDGE_CURVE('',#6938,#6936,#4225,.T.);
#8712=EDGE_CURVE('',#6939,#6937,#5756,.T.);
#8713=EDGE_CURVE('',#6939,#6774,#882,.T.);
#8714=EDGE_CURVE('',#6940,#6939,#337,.T.);
#8715=EDGE_CURVE('',#6775,#6940,#4226,.T.);
#8716=EDGE_CURVE('',#6777,#6941,#883,.T.);
#8717=EDGE_CURVE('',#6776,#6942,#4227,.T.);
#8718=EDGE_CURVE('',#6941,#6942,#338,.T.);
#8719=EDGE_CURVE('',#6942,#6940,#4228,.T.);
#8720=EDGE_CURVE('',#6943,#6941,#5757,.T.);
#8721=EDGE_CURVE('',#6943,#6778,#884,.T.);
#8722=EDGE_CURVE('',#6944,#6943,#339,.T.);
#8723=EDGE_CURVE('',#6779,#6944,#4229,.T.);
#8724=EDGE_CURVE('',#6781,#6945,#885,.T.);
#8725=EDGE_CURVE('',#6780,#6946,#4230,.T.);
#8726=EDGE_CURVE('',#6945,#6946,#340,.T.);
#8727=EDGE_CURVE('',#6946,#6944,#4231,.T.);
#8728=EDGE_CURVE('',#6947,#6945,#5758,.T.);
#8729=EDGE_CURVE('',#6947,#6782,#886,.T.);
#8730=EDGE_CURVE('',#6948,#6947,#341,.T.);
#8731=EDGE_CURVE('',#6783,#6948,#4232,.T.);
#8732=EDGE_CURVE('',#6785,#6949,#887,.T.);
#8733=EDGE_CURVE('',#6784,#6950,#4233,.T.);
#8734=EDGE_CURVE('',#6949,#6950,#342,.T.);
#8735=EDGE_CURVE('',#6950,#6948,#4234,.T.);
#8736=EDGE_CURVE('',#6951,#6949,#5759,.T.);
#8737=EDGE_CURVE('',#6951,#6786,#888,.T.);
#8738=EDGE_CURVE('',#6952,#6951,#343,.T.);
#8739=EDGE_CURVE('',#6787,#6952,#4235,.T.);
#8740=EDGE_CURVE('',#6789,#6953,#889,.T.);
#8741=EDGE_CURVE('',#6788,#6954,#4236,.T.);
#8742=EDGE_CURVE('',#6953,#6954,#344,.T.);
#8743=EDGE_CURVE('',#6954,#6952,#4237,.T.);
#8744=EDGE_CURVE('',#6955,#6953,#5760,.T.);
#8745=EDGE_CURVE('',#6955,#6790,#890,.T.);
#8746=EDGE_CURVE('',#6956,#6955,#345,.T.);
#8747=EDGE_CURVE('',#6791,#6956,#4238,.T.);
#8748=EDGE_CURVE('',#6793,#6957,#891,.T.);
#8749=EDGE_CURVE('',#6792,#6958,#4239,.T.);
#8750=EDGE_CURVE('',#6957,#6958,#346,.T.);
#8751=EDGE_CURVE('',#6958,#6956,#4240,.T.);
#8752=EDGE_CURVE('',#6959,#6957,#5761,.T.);
#8753=EDGE_CURVE('',#6959,#6794,#892,.T.);
#8754=EDGE_CURVE('',#6960,#6959,#347,.T.);
#8755=EDGE_CURVE('',#6795,#6960,#4241,.T.);
#8756=EDGE_CURVE('',#6797,#6961,#893,.T.);
#8757=EDGE_CURVE('',#6796,#6962,#4242,.T.);
#8758=EDGE_CURVE('',#6961,#6962,#348,.T.);
#8759=EDGE_CURVE('',#6962,#6960,#4243,.T.);
#8760=EDGE_CURVE('',#6963,#6961,#5762,.T.);
#8761=EDGE_CURVE('',#6963,#6798,#894,.T.);
#8762=EDGE_CURVE('',#6964,#6963,#349,.T.);
#8763=EDGE_CURVE('',#6799,#6964,#4244,.T.);
#8764=EDGE_CURVE('',#6801,#6965,#895,.T.);
#8765=EDGE_CURVE('',#6800,#6966,#4245,.T.);
#8766=EDGE_CURVE('',#6965,#6966,#350,.T.);
#8767=EDGE_CURVE('',#6966,#6964,#4246,.T.);
#8768=EDGE_CURVE('',#6967,#6965,#5763,.T.);
#8769=EDGE_CURVE('',#6967,#6802,#896,.T.);
#8770=EDGE_CURVE('',#6968,#6967,#351,.T.);
#8771=EDGE_CURVE('',#6803,#6968,#4247,.T.);
#8772=EDGE_CURVE('',#6805,#6969,#897,.T.);
#8773=EDGE_CURVE('',#6804,#6970,#4248,.T.);
#8774=EDGE_CURVE('',#6969,#6970,#352,.T.);
#8775=EDGE_CURVE('',#6970,#6968,#4249,.T.);
#8776=EDGE_CURVE('',#6971,#6969,#5764,.T.);
#8777=EDGE_CURVE('',#6971,#6806,#898,.T.);
#8778=EDGE_CURVE('',#6972,#6971,#353,.T.);
#8779=EDGE_CURVE('',#6807,#6972,#4250,.T.);
#8780=EDGE_CURVE('',#6809,#6973,#899,.T.);
#8781=EDGE_CURVE('',#6808,#6974,#4251,.T.);
#8782=EDGE_CURVE('',#6973,#6974,#354,.T.);
#8783=EDGE_CURVE('',#6974,#6972,#4252,.T.);
#8784=EDGE_CURVE('',#6975,#6973,#5765,.T.);
#8785=EDGE_CURVE('',#6975,#6810,#900,.T.);
#8786=EDGE_CURVE('',#6976,#6975,#355,.T.);
#8787=EDGE_CURVE('',#6811,#6976,#4253,.T.);
#8788=EDGE_CURVE('',#6813,#6977,#901,.T.);
#8789=EDGE_CURVE('',#6812,#6978,#4254,.T.);
#8790=EDGE_CURVE('',#6977,#6978,#356,.T.);
#8791=EDGE_CURVE('',#6978,#6976,#4255,.T.);
#8792=EDGE_CURVE('',#6979,#6977,#5766,.T.);
#8793=EDGE_CURVE('',#6979,#6814,#902,.T.);
#8794=EDGE_CURVE('',#6980,#6979,#357,.T.);
#8795=EDGE_CURVE('',#6815,#6980,#4256,.T.);
#8796=EDGE_CURVE('',#6817,#6981,#903,.T.);
#8797=EDGE_CURVE('',#6816,#6982,#4257,.T.);
#8798=EDGE_CURVE('',#6981,#6982,#358,.T.);
#8799=EDGE_CURVE('',#6982,#6980,#4258,.T.);
#8800=EDGE_CURVE('',#6983,#6981,#5767,.T.);
#8801=EDGE_CURVE('',#6983,#6818,#904,.T.);
#8802=EDGE_CURVE('',#6984,#6983,#359,.T.);
#8803=EDGE_CURVE('',#6819,#6984,#4259,.T.);
#8804=EDGE_CURVE('',#6821,#6985,#905,.T.);
#8805=EDGE_CURVE('',#6820,#6986,#4260,.T.);
#8806=EDGE_CURVE('',#6985,#6986,#360,.T.);
#8807=EDGE_CURVE('',#6986,#6984,#4261,.T.);
#8808=EDGE_CURVE('',#6987,#6985,#5768,.T.);
#8809=EDGE_CURVE('',#6987,#6822,#906,.T.);
#8810=EDGE_CURVE('',#6988,#6987,#361,.T.);
#8811=EDGE_CURVE('',#6823,#6988,#4262,.T.);
#8812=EDGE_CURVE('',#6825,#6989,#907,.T.);
#8813=EDGE_CURVE('',#6824,#6990,#4263,.T.);
#8814=EDGE_CURVE('',#6989,#6990,#362,.T.);
#8815=EDGE_CURVE('',#6990,#6988,#4264,.T.);
#8816=EDGE_CURVE('',#6991,#6989,#5769,.T.);
#8817=EDGE_CURVE('',#6991,#6826,#908,.T.);
#8818=EDGE_CURVE('',#6992,#6991,#363,.T.);
#8819=EDGE_CURVE('',#6827,#6992,#4265,.T.);
#8820=EDGE_CURVE('',#6829,#6993,#909,.T.);
#8821=EDGE_CURVE('',#6828,#6994,#4266,.T.);
#8822=EDGE_CURVE('',#6993,#6994,#364,.T.);
#8823=EDGE_CURVE('',#6994,#6992,#4267,.T.);
#8824=EDGE_CURVE('',#6995,#6993,#5770,.T.);
#8825=EDGE_CURVE('',#6995,#6830,#910,.T.);
#8826=EDGE_CURVE('',#6996,#6995,#365,.T.);
#8827=EDGE_CURVE('',#6831,#6996,#4268,.T.);
#8828=EDGE_CURVE('',#6833,#6997,#911,.T.);
#8829=EDGE_CURVE('',#6832,#6998,#4269,.T.);
#8830=EDGE_CURVE('',#6997,#6998,#366,.T.);
#8831=EDGE_CURVE('',#6998,#6996,#4270,.T.);
#8832=EDGE_CURVE('',#6999,#6997,#5771,.T.);
#8833=EDGE_CURVE('',#6999,#6834,#912,.T.);
#8834=EDGE_CURVE('',#7000,#6999,#367,.T.);
#8835=EDGE_CURVE('',#6835,#7000,#4271,.T.);
#8836=EDGE_CURVE('',#7001,#7000,#4272,.T.);
#8837=EDGE_CURVE('',#6836,#7001,#4273,.T.);
#8838=EDGE_CURVE('',#6837,#7002,#913,.T.);
#8839=EDGE_CURVE('',#7002,#7001,#368,.T.);
#8840=EDGE_CURVE('',#7003,#7002,#5772,.T.);
#8841=EDGE_CURVE('',#7003,#6838,#914,.T.);
#8842=EDGE_CURVE('',#6841,#7004,#915,.T.);
#8843=EDGE_CURVE('',#6840,#7005,#4274,.T.);
#8844=EDGE_CURVE('',#7004,#7005,#369,.T.);
#8845=EDGE_CURVE('',#7006,#7003,#370,.T.);
#8846=EDGE_CURVE('',#6839,#7006,#4275,.T.);
#8847=EDGE_CURVE('',#7005,#7006,#4276,.T.);
#8848=EDGE_CURVE('',#6847,#7004,#5773,.T.);
#8849=EDGE_CURVE('',#7007,#7008,#4277,.T.);
#8850=EDGE_CURVE('',#7008,#7009,#4278,.T.);
#8851=EDGE_CURVE('',#7009,#7010,#4279,.T.);
#8852=EDGE_CURVE('',#7007,#7010,#4280,.T.);
#8853=EDGE_CURVE('',#7008,#7011,#4281,.T.);
#8854=EDGE_CURVE('',#7011,#7012,#4282,.T.);
#8855=EDGE_CURVE('',#7012,#7009,#4283,.T.);
#8856=EDGE_CURVE('',#7011,#7013,#4284,.T.);
#8857=EDGE_CURVE('',#7013,#7014,#4285,.T.);
#8858=EDGE_CURVE('',#7014,#7012,#4286,.T.);
#8859=EDGE_CURVE('',#7013,#7015,#4287,.T.);
#8860=EDGE_CURVE('',#7015,#7016,#4288,.T.);
#8861=EDGE_CURVE('',#7016,#7014,#4289,.T.);
#8862=EDGE_CURVE('',#7015,#7017,#4290,.T.);
#8863=EDGE_CURVE('',#7017,#7018,#4291,.T.);
#8864=EDGE_CURVE('',#7018,#7016,#4292,.T.);
#8865=EDGE_CURVE('',#7017,#7007,#4293,.T.);
#8866=EDGE_CURVE('',#7010,#7018,#4294,.T.);
#8867=EDGE_CURVE('',#7019,#7019,#5774,.T.);
#8868=EDGE_CURVE('',#7020,#7020,#5775,.T.);
#8869=EDGE_CURVE('',#7021,#7021,#5776,.T.);
#8870=EDGE_CURVE('',#7021,#7020,#4295,.T.);
#8871=EDGE_CURVE('',#7022,#7022,#5777,.T.);
#8872=EDGE_CURVE('',#7022,#7021,#4296,.T.);
#8873=EDGE_CURVE('',#7023,#7023,#5778,.T.);
#8874=EDGE_CURVE('',#7023,#7022,#4297,.T.);
#8875=EDGE_CURVE('',#7024,#7024,#5779,.T.);
#8876=EDGE_CURVE('',#7025,#7025,#5780,.F.);
#8877=EDGE_CURVE('',#7025,#7024,#4298,.T.);
#8878=EDGE_CURVE('',#7019,#7025,#4299,.T.);
#8879=ORIENTED_EDGE('',*,*,#7026,.F.);
#8880=ORIENTED_EDGE('',*,*,#7027,.T.);
#8881=ORIENTED_EDGE('',*,*,#7028,.F.);
#8882=ORIENTED_EDGE('',*,*,#7027,.F.);
#8883=ORIENTED_EDGE('',*,*,#7029,.F.);
#8884=ORIENTED_EDGE('',*,*,#7030,.T.);
#8885=ORIENTED_EDGE('',*,*,#7031,.F.);
#8886=ORIENTED_EDGE('',*,*,#7030,.F.);
#8887=ORIENTED_EDGE('',*,*,#7032,.F.);
#8888=ORIENTED_EDGE('',*,*,#7033,.T.);
#8889=ORIENTED_EDGE('',*,*,#7034,.F.);
#8890=ORIENTED_EDGE('',*,*,#7033,.F.);
#8891=ORIENTED_EDGE('',*,*,#7035,.F.);
#8892=ORIENTED_EDGE('',*,*,#7036,.T.);
#8893=ORIENTED_EDGE('',*,*,#7037,.F.);
#8894=ORIENTED_EDGE('',*,*,#7036,.F.);
#8895=ORIENTED_EDGE('',*,*,#7038,.F.);
#8896=ORIENTED_EDGE('',*,*,#7039,.T.);
#8897=ORIENTED_EDGE('',*,*,#7040,.F.);
#8898=ORIENTED_EDGE('',*,*,#7039,.F.);
#8899=ORIENTED_EDGE('',*,*,#7041,.F.);
#8900=ORIENTED_EDGE('',*,*,#7042,.T.);
#8901=ORIENTED_EDGE('',*,*,#7043,.F.);
#8902=ORIENTED_EDGE('',*,*,#7042,.F.);
#8903=ORIENTED_EDGE('',*,*,#7044,.F.);
#8904=ORIENTED_EDGE('',*,*,#7045,.T.);
#8905=ORIENTED_EDGE('',*,*,#7046,.F.);
#8906=ORIENTED_EDGE('',*,*,#7045,.F.);
#8907=ORIENTED_EDGE('',*,*,#7047,.F.);
#8908=ORIENTED_EDGE('',*,*,#7048,.T.);
#8909=ORIENTED_EDGE('',*,*,#7049,.F.);
#8910=ORIENTED_EDGE('',*,*,#7048,.F.);
#8911=ORIENTED_EDGE('',*,*,#7050,.F.);
#8912=ORIENTED_EDGE('',*,*,#7051,.T.);
#8913=ORIENTED_EDGE('',*,*,#7052,.F.);
#8914=ORIENTED_EDGE('',*,*,#7051,.F.);
#8915=ORIENTED_EDGE('',*,*,#7053,.F.);
#8916=ORIENTED_EDGE('',*,*,#7054,.T.);
#8917=ORIENTED_EDGE('',*,*,#7055,.F.);
#8918=ORIENTED_EDGE('',*,*,#7054,.F.);
#8919=ORIENTED_EDGE('',*,*,#7056,.F.);
#8920=ORIENTED_EDGE('',*,*,#7057,.T.);
#8921=ORIENTED_EDGE('',*,*,#7058,.F.);
#8922=ORIENTED_EDGE('',*,*,#7057,.F.);
#8923=ORIENTED_EDGE('',*,*,#7059,.F.);
#8924=ORIENTED_EDGE('',*,*,#7060,.T.);
#8925=ORIENTED_EDGE('',*,*,#7061,.F.);
#8926=ORIENTED_EDGE('',*,*,#7060,.F.);
#8927=ORIENTED_EDGE('',*,*,#7062,.T.);
#8928=ORIENTED_EDGE('',*,*,#7063,.T.);
#8929=ORIENTED_EDGE('',*,*,#7064,.F.);
#8930=ORIENTED_EDGE('',*,*,#7065,.F.);
#8931=ORIENTED_EDGE('',*,*,#7066,.T.);
#8932=ORIENTED_EDGE('',*,*,#7065,.T.);
#8933=ORIENTED_EDGE('',*,*,#7067,.F.);
#8934=ORIENTED_EDGE('',*,*,#7068,.F.);
#8935=ORIENTED_EDGE('',*,*,#7069,.T.);
#8936=ORIENTED_EDGE('',*,*,#7068,.T.);
#8937=ORIENTED_EDGE('',*,*,#7070,.F.);
#8938=ORIENTED_EDGE('',*,*,#7071,.F.);
#8939=ORIENTED_EDGE('',*,*,#7072,.T.);
#8940=ORIENTED_EDGE('',*,*,#7071,.T.);
#8941=ORIENTED_EDGE('',*,*,#7073,.F.);
#8942=ORIENTED_EDGE('',*,*,#7063,.F.);
#8943=ORIENTED_EDGE('',*,*,#7073,.T.);
#8944=ORIENTED_EDGE('',*,*,#7070,.T.);
#8945=ORIENTED_EDGE('',*,*,#7067,.T.);
#8946=ORIENTED_EDGE('',*,*,#7064,.T.);
#8947=ORIENTED_EDGE('',*,*,#7040,.T.);
#8948=ORIENTED_EDGE('',*,*,#7043,.T.);
#8949=ORIENTED_EDGE('',*,*,#7046,.T.);
#8950=ORIENTED_EDGE('',*,*,#7049,.T.);
#8951=ORIENTED_EDGE('',*,*,#7052,.T.);
#8952=ORIENTED_EDGE('',*,*,#7055,.T.);
#8953=ORIENTED_EDGE('',*,*,#7058,.T.);
#8954=ORIENTED_EDGE('',*,*,#7061,.T.);
#8955=ORIENTED_EDGE('',*,*,#7037,.T.);
#8956=ORIENTED_EDGE('',*,*,#7034,.T.);
#8957=ORIENTED_EDGE('',*,*,#7031,.T.);
#8958=ORIENTED_EDGE('',*,*,#7028,.T.);
#8959=ORIENTED_EDGE('',*,*,#7072,.F.);
#8960=ORIENTED_EDGE('',*,*,#7062,.F.);
#8961=ORIENTED_EDGE('',*,*,#7066,.F.);
#8962=ORIENTED_EDGE('',*,*,#7069,.F.);
#8963=ORIENTED_EDGE('',*,*,#7038,.T.);
#8964=ORIENTED_EDGE('',*,*,#7041,.T.);
#8965=ORIENTED_EDGE('',*,*,#7044,.T.);
#8966=ORIENTED_EDGE('',*,*,#7047,.T.);
#8967=ORIENTED_EDGE('',*,*,#7050,.T.);
#8968=ORIENTED_EDGE('',*,*,#7053,.T.);
#8969=ORIENTED_EDGE('',*,*,#7056,.T.);
#8970=ORIENTED_EDGE('',*,*,#7059,.T.);
#8971=ORIENTED_EDGE('',*,*,#7035,.T.);
#8972=ORIENTED_EDGE('',*,*,#7032,.T.);
#8973=ORIENTED_EDGE('',*,*,#7029,.T.);
#8974=ORIENTED_EDGE('',*,*,#7026,.T.);
#8975=ORIENTED_EDGE('',*,*,#7074,.T.);
#8976=ORIENTED_EDGE('',*,*,#7075,.T.);
#8977=ORIENTED_EDGE('',*,*,#7076,.F.);
#8978=ORIENTED_EDGE('',*,*,#7077,.F.);
#8979=ORIENTED_EDGE('',*,*,#7078,.T.);
#8980=ORIENTED_EDGE('',*,*,#7077,.T.);
#8981=ORIENTED_EDGE('',*,*,#7079,.F.);
#8982=ORIENTED_EDGE('',*,*,#7080,.F.);
#8983=ORIENTED_EDGE('',*,*,#7081,.T.);
#8984=ORIENTED_EDGE('',*,*,#7080,.T.);
#8985=ORIENTED_EDGE('',*,*,#7082,.F.);
#8986=ORIENTED_EDGE('',*,*,#7083,.F.);
#8987=ORIENTED_EDGE('',*,*,#7084,.T.);
#8988=ORIENTED_EDGE('',*,*,#7083,.T.);
#8989=ORIENTED_EDGE('',*,*,#7085,.F.);
#8990=ORIENTED_EDGE('',*,*,#7075,.F.);
#8991=ORIENTED_EDGE('',*,*,#7085,.T.);
#8992=ORIENTED_EDGE('',*,*,#7082,.T.);
#8993=ORIENTED_EDGE('',*,*,#7079,.T.);
#8994=ORIENTED_EDGE('',*,*,#7076,.T.);
#8995=ORIENTED_EDGE('',*,*,#7084,.F.);
#8996=ORIENTED_EDGE('',*,*,#7074,.F.);
#8997=ORIENTED_EDGE('',*,*,#7078,.F.);
#8998=ORIENTED_EDGE('',*,*,#7081,.F.);
#8999=ORIENTED_EDGE('',*,*,#7086,.T.);
#9000=ORIENTED_EDGE('',*,*,#7087,.T.);
#9001=ORIENTED_EDGE('',*,*,#7088,.F.);
#9002=ORIENTED_EDGE('',*,*,#7089,.F.);
#9003=ORIENTED_EDGE('',*,*,#7090,.T.);
#9004=ORIENTED_EDGE('',*,*,#7089,.T.);
#9005=ORIENTED_EDGE('',*,*,#7091,.F.);
#9006=ORIENTED_EDGE('',*,*,#7092,.F.);
#9007=ORIENTED_EDGE('',*,*,#7093,.T.);
#9008=ORIENTED_EDGE('',*,*,#7092,.T.);
#9009=ORIENTED_EDGE('',*,*,#7094,.F.);
#9010=ORIENTED_EDGE('',*,*,#7095,.F.);
#9011=ORIENTED_EDGE('',*,*,#7096,.T.);
#9012=ORIENTED_EDGE('',*,*,#7095,.T.);
#9013=ORIENTED_EDGE('',*,*,#7097,.F.);
#9014=ORIENTED_EDGE('',*,*,#7087,.F.);
#9015=ORIENTED_EDGE('',*,*,#7097,.T.);
#9016=ORIENTED_EDGE('',*,*,#7094,.T.);
#9017=ORIENTED_EDGE('',*,*,#7091,.T.);
#9018=ORIENTED_EDGE('',*,*,#7088,.T.);
#9019=ORIENTED_EDGE('',*,*,#7096,.F.);
#9020=ORIENTED_EDGE('',*,*,#7086,.F.);
#9021=ORIENTED_EDGE('',*,*,#7090,.F.);
#9022=ORIENTED_EDGE('',*,*,#7093,.F.);
#9023=ORIENTED_EDGE('',*,*,#7098,.F.);
#9024=ORIENTED_EDGE('',*,*,#7099,.F.);
#9025=ORIENTED_EDGE('',*,*,#7100,.T.);
#9026=ORIENTED_EDGE('',*,*,#7101,.F.);
#9027=ORIENTED_EDGE('',*,*,#7102,.F.);
#9028=ORIENTED_EDGE('',*,*,#7100,.F.);
#9029=ORIENTED_EDGE('',*,*,#7103,.F.);
#9030=ORIENTED_EDGE('',*,*,#7104,.T.);
#9031=ORIENTED_EDGE('',*,*,#7105,.F.);
#9032=ORIENTED_EDGE('',*,*,#7104,.F.);
#9033=ORIENTED_EDGE('',*,*,#7103,.T.);
#9034=ORIENTED_EDGE('',*,*,#7106,.F.);
#9035=ORIENTED_EDGE('',*,*,#7107,.T.);
#9036=ORIENTED_EDGE('',*,*,#7108,.F.);
#9037=ORIENTED_EDGE('',*,*,#7107,.F.);
#9038=ORIENTED_EDGE('',*,*,#7106,.T.);
#9039=ORIENTED_EDGE('',*,*,#7109,.F.);
#9040=ORIENTED_EDGE('',*,*,#7110,.T.);
#9041=ORIENTED_EDGE('',*,*,#7111,.F.);
#9042=ORIENTED_EDGE('',*,*,#7110,.F.);
#9043=ORIENTED_EDGE('',*,*,#7109,.T.);
#9044=ORIENTED_EDGE('',*,*,#7112,.F.);
#9045=ORIENTED_EDGE('',*,*,#7113,.T.);
#9046=ORIENTED_EDGE('',*,*,#7114,.F.);
#9047=ORIENTED_EDGE('',*,*,#7113,.F.);
#9048=ORIENTED_EDGE('',*,*,#7112,.T.);
#9049=ORIENTED_EDGE('',*,*,#7115,.F.);
#9050=ORIENTED_EDGE('',*,*,#7116,.F.);
#9051=ORIENTED_EDGE('',*,*,#7117,.F.);
#9052=ORIENTED_EDGE('',*,*,#7118,.F.);
#9053=ORIENTED_EDGE('',*,*,#7119,.F.);
#9054=ORIENTED_EDGE('',*,*,#7116,.T.);
#9055=ORIENTED_EDGE('',*,*,#7120,.F.);
#9056=ORIENTED_EDGE('',*,*,#7121,.T.);
#9057=ORIENTED_EDGE('',*,*,#7122,.F.);
#9058=ORIENTED_EDGE('',*,*,#7123,.F.);
#9059=ORIENTED_EDGE('',*,*,#7124,.F.);
#9060=ORIENTED_EDGE('',*,*,#7121,.F.);
#9061=ORIENTED_EDGE('',*,*,#7125,.F.);
#9062=ORIENTED_EDGE('',*,*,#7126,.T.);
#9063=ORIENTED_EDGE('',*,*,#7127,.F.);
#9064=ORIENTED_EDGE('',*,*,#7128,.F.);
#9065=ORIENTED_EDGE('',*,*,#7129,.F.);
#9066=ORIENTED_EDGE('',*,*,#7126,.F.);
#9067=ORIENTED_EDGE('',*,*,#7130,.F.);
#9068=ORIENTED_EDGE('',*,*,#7131,.T.);
#9069=ORIENTED_EDGE('',*,*,#7132,.F.);
#9070=ORIENTED_EDGE('',*,*,#7133,.F.);
#9071=ORIENTED_EDGE('',*,*,#7134,.F.);
#9072=ORIENTED_EDGE('',*,*,#7131,.F.);
#9073=ORIENTED_EDGE('',*,*,#7135,.F.);
#9074=ORIENTED_EDGE('',*,*,#7136,.T.);
#9075=ORIENTED_EDGE('',*,*,#7137,.T.);
#9076=ORIENTED_EDGE('',*,*,#7117,.T.);
#9077=ORIENTED_EDGE('',*,*,#7115,.T.);
#9078=ORIENTED_EDGE('',*,*,#7119,.T.);
#9079=ORIENTED_EDGE('',*,*,#7138,.T.);
#9080=ORIENTED_EDGE('',*,*,#7132,.T.);
#9081=ORIENTED_EDGE('',*,*,#7134,.T.);
#9082=ORIENTED_EDGE('',*,*,#7130,.T.);
#9083=ORIENTED_EDGE('',*,*,#7139,.T.);
#9084=ORIENTED_EDGE('',*,*,#7127,.T.);
#9085=ORIENTED_EDGE('',*,*,#7129,.T.);
#9086=ORIENTED_EDGE('',*,*,#7125,.T.);
#9087=ORIENTED_EDGE('',*,*,#7140,.T.);
#9088=ORIENTED_EDGE('',*,*,#7122,.T.);
#9089=ORIENTED_EDGE('',*,*,#7124,.T.);
#9090=ORIENTED_EDGE('',*,*,#7120,.T.);
#9091=ORIENTED_EDGE('',*,*,#7141,.T.);
#9092=ORIENTED_EDGE('',*,*,#7136,.F.);
#9093=ORIENTED_EDGE('',*,*,#7101,.T.);
#9094=ORIENTED_EDGE('',*,*,#7102,.T.);
#9095=ORIENTED_EDGE('',*,*,#7142,.T.);
#9096=ORIENTED_EDGE('',*,*,#7141,.F.);
#9097=ORIENTED_EDGE('',*,*,#7123,.T.);
#9098=ORIENTED_EDGE('',*,*,#7140,.F.);
#9099=ORIENTED_EDGE('',*,*,#7128,.T.);
#9100=ORIENTED_EDGE('',*,*,#7139,.F.);
#9101=ORIENTED_EDGE('',*,*,#7133,.T.);
#9102=ORIENTED_EDGE('',*,*,#7138,.F.);
#9103=ORIENTED_EDGE('',*,*,#7118,.T.);
#9104=ORIENTED_EDGE('',*,*,#7137,.F.);
#9105=ORIENTED_EDGE('',*,*,#7143,.T.);
#9106=ORIENTED_EDGE('',*,*,#7144,.T.);
#9107=ORIENTED_EDGE('',*,*,#7145,.T.);
#9108=ORIENTED_EDGE('',*,*,#7146,.T.);
#9109=ORIENTED_EDGE('',*,*,#7147,.F.);
#9110=ORIENTED_EDGE('',*,*,#7148,.T.);
#9111=ORIENTED_EDGE('',*,*,#7143,.F.);
#9112=ORIENTED_EDGE('',*,*,#7148,.F.);
#9113=ORIENTED_EDGE('',*,*,#7149,.F.);
#9114=ORIENTED_EDGE('',*,*,#7150,.T.);
#9115=ORIENTED_EDGE('',*,*,#7146,.F.);
#9116=ORIENTED_EDGE('',*,*,#7150,.F.);
#9117=ORIENTED_EDGE('',*,*,#7151,.F.);
#9118=ORIENTED_EDGE('',*,*,#7152,.T.);
#9119=ORIENTED_EDGE('',*,*,#7144,.F.);
#9120=ORIENTED_EDGE('',*,*,#7152,.F.);
#9121=ORIENTED_EDGE('',*,*,#7153,.F.);
#9122=ORIENTED_EDGE('',*,*,#7154,.T.);
#9123=ORIENTED_EDGE('',*,*,#7145,.F.);
#9124=ORIENTED_EDGE('',*,*,#7154,.F.);
#9125=ORIENTED_EDGE('',*,*,#7155,.F.);
#9126=ORIENTED_EDGE('',*,*,#7156,.T.);
#9127=ORIENTED_EDGE('',*,*,#7157,.F.);
#9128=ORIENTED_EDGE('',*,*,#7156,.F.);
#9129=ORIENTED_EDGE('',*,*,#7155,.T.);
#9130=ORIENTED_EDGE('',*,*,#7158,.F.);
#9131=ORIENTED_EDGE('',*,*,#7142,.F.);
#9132=ORIENTED_EDGE('',*,*,#7159,.T.);
#9133=ORIENTED_EDGE('',*,*,#7160,.T.);
#9134=ORIENTED_EDGE('',*,*,#7159,.F.);
#9135=ORIENTED_EDGE('',*,*,#7158,.T.);
#9136=ORIENTED_EDGE('',*,*,#7161,.T.);
#9137=ORIENTED_EDGE('',*,*,#7162,.T.);
#9138=ORIENTED_EDGE('',*,*,#7161,.F.);
#9139=ORIENTED_EDGE('',*,*,#7098,.T.);
#9140=ORIENTED_EDGE('',*,*,#7099,.T.);
#9141=ORIENTED_EDGE('',*,*,#7135,.T.);
#9142=ORIENTED_EDGE('',*,*,#7157,.T.);
#9143=ORIENTED_EDGE('',*,*,#7114,.T.);
#9144=ORIENTED_EDGE('',*,*,#7111,.T.);
#9145=ORIENTED_EDGE('',*,*,#7108,.T.);
#9146=ORIENTED_EDGE('',*,*,#7105,.T.);
#9147=ORIENTED_EDGE('',*,*,#7160,.F.);
#9148=ORIENTED_EDGE('',*,*,#7162,.F.);
#9149=ORIENTED_EDGE('',*,*,#7153,.T.);
#9150=ORIENTED_EDGE('',*,*,#7151,.T.);
#9151=ORIENTED_EDGE('',*,*,#7149,.T.);
#9152=ORIENTED_EDGE('',*,*,#7147,.T.);
#9153=ORIENTED_EDGE('',*,*,#7163,.F.);
#9154=ORIENTED_EDGE('',*,*,#7164,.T.);
#9155=ORIENTED_EDGE('',*,*,#7165,.T.);
#9156=ORIENTED_EDGE('',*,*,#7164,.F.);
#9157=ORIENTED_EDGE('',*,*,#7166,.F.);
#9158=ORIENTED_EDGE('',*,*,#7167,.T.);
#9159=ORIENTED_EDGE('',*,*,#7168,.T.);
#9160=ORIENTED_EDGE('',*,*,#7167,.F.);
#9161=ORIENTED_EDGE('',*,*,#7166,.T.);
#9162=ORIENTED_EDGE('',*,*,#7163,.T.);
#9163=ORIENTED_EDGE('',*,*,#7168,.F.);
#9164=ORIENTED_EDGE('',*,*,#7165,.F.);
#9165=ORIENTED_EDGE('',*,*,#7169,.F.);
#9166=ORIENTED_EDGE('',*,*,#7170,.F.);
#9167=ORIENTED_EDGE('',*,*,#7171,.F.);
#9168=ORIENTED_EDGE('',*,*,#7172,.F.);
#9169=ORIENTED_EDGE('',*,*,#7173,.F.);
#9170=ORIENTED_EDGE('',*,*,#7174,.F.);
#9171=ORIENTED_EDGE('',*,*,#7175,.F.);
#9172=ORIENTED_EDGE('',*,*,#7176,.F.);
#9173=ORIENTED_EDGE('',*,*,#7177,.F.);
#9174=ORIENTED_EDGE('',*,*,#7178,.F.);
#9175=ORIENTED_EDGE('',*,*,#7179,.F.);
#9176=ORIENTED_EDGE('',*,*,#7180,.F.);
#9177=ORIENTED_EDGE('',*,*,#7181,.F.);
#9178=ORIENTED_EDGE('',*,*,#7182,.F.);
#9179=ORIENTED_EDGE('',*,*,#7183,.F.);
#9180=ORIENTED_EDGE('',*,*,#7184,.F.);
#9181=ORIENTED_EDGE('',*,*,#7170,.T.);
#9182=ORIENTED_EDGE('',*,*,#7185,.F.);
#9183=ORIENTED_EDGE('',*,*,#7174,.T.);
#9184=ORIENTED_EDGE('',*,*,#7186,.F.);
#9185=ORIENTED_EDGE('',*,*,#7178,.T.);
#9186=ORIENTED_EDGE('',*,*,#7187,.F.);
#9187=ORIENTED_EDGE('',*,*,#7182,.T.);
#9188=ORIENTED_EDGE('',*,*,#7188,.F.);
#9189=ORIENTED_EDGE('',*,*,#7189,.T.);
#9190=ORIENTED_EDGE('',*,*,#7177,.T.);
#9191=ORIENTED_EDGE('',*,*,#7190,.F.);
#9192=ORIENTED_EDGE('',*,*,#7183,.T.);
#9193=ORIENTED_EDGE('',*,*,#7187,.T.);
#9194=ORIENTED_EDGE('',*,*,#7173,.T.);
#9195=ORIENTED_EDGE('',*,*,#7191,.F.);
#9196=ORIENTED_EDGE('',*,*,#7179,.T.);
#9197=ORIENTED_EDGE('',*,*,#7186,.T.);
#9198=ORIENTED_EDGE('',*,*,#7169,.T.);
#9199=ORIENTED_EDGE('',*,*,#7192,.F.);
#9200=ORIENTED_EDGE('',*,*,#7175,.T.);
#9201=ORIENTED_EDGE('',*,*,#7185,.T.);
#9202=ORIENTED_EDGE('',*,*,#7171,.T.);
#9203=ORIENTED_EDGE('',*,*,#7188,.T.);
#9204=ORIENTED_EDGE('',*,*,#7181,.T.);
#9205=ORIENTED_EDGE('',*,*,#7193,.F.);
#9206=ORIENTED_EDGE('',*,*,#7189,.F.);
#9207=ORIENTED_EDGE('',*,*,#7194,.T.);
#9208=ORIENTED_EDGE('',*,*,#7195,.T.);
#9209=ORIENTED_EDGE('',*,*,#7194,.F.);
#9210=ORIENTED_EDGE('',*,*,#7195,.F.);
#9211=ORIENTED_EDGE('',*,*,#7196,.F.);
#9212=ORIENTED_EDGE('',*,*,#7197,.F.);
#9213=ORIENTED_EDGE('',*,*,#7198,.T.);
#9214=ORIENTED_EDGE('',*,*,#7196,.T.);
#9215=ORIENTED_EDGE('',*,*,#7198,.F.);
#9216=ORIENTED_EDGE('',*,*,#7172,.T.);
#9217=ORIENTED_EDGE('',*,*,#7193,.T.);
#9218=ORIENTED_EDGE('',*,*,#7184,.T.);
#9219=ORIENTED_EDGE('',*,*,#7190,.T.);
#9220=ORIENTED_EDGE('',*,*,#7180,.T.);
#9221=ORIENTED_EDGE('',*,*,#7191,.T.);
#9222=ORIENTED_EDGE('',*,*,#7176,.T.);
#9223=ORIENTED_EDGE('',*,*,#7192,.T.);
#9224=ORIENTED_EDGE('',*,*,#7197,.T.);
#9225=ORIENTED_EDGE('',*,*,#7199,.F.);
#9226=ORIENTED_EDGE('',*,*,#7200,.T.);
#9227=ORIENTED_EDGE('',*,*,#7201,.F.);
#9228=ORIENTED_EDGE('',*,*,#7200,.F.);
#9229=ORIENTED_EDGE('',*,*,#7202,.F.);
#9230=ORIENTED_EDGE('',*,*,#7203,.T.);
#9231=ORIENTED_EDGE('',*,*,#7204,.F.);
#9232=ORIENTED_EDGE('',*,*,#7203,.F.);
#9233=ORIENTED_EDGE('',*,*,#7205,.F.);
#9234=ORIENTED_EDGE('',*,*,#7206,.T.);
#9235=ORIENTED_EDGE('',*,*,#7207,.F.);
#9236=ORIENTED_EDGE('',*,*,#7206,.F.);
#9237=ORIENTED_EDGE('',*,*,#7208,.F.);
#9238=ORIENTED_EDGE('',*,*,#7209,.T.);
#9239=ORIENTED_EDGE('',*,*,#7210,.F.);
#9240=ORIENTED_EDGE('',*,*,#7209,.F.);
#9241=ORIENTED_EDGE('',*,*,#7211,.F.);
#9242=ORIENTED_EDGE('',*,*,#7212,.T.);
#9243=ORIENTED_EDGE('',*,*,#7213,.F.);
#9244=ORIENTED_EDGE('',*,*,#7212,.F.);
#9245=ORIENTED_EDGE('',*,*,#7211,.T.);
#9246=ORIENTED_EDGE('',*,*,#7214,.F.);
#9247=ORIENTED_EDGE('',*,*,#7215,.T.);
#9248=ORIENTED_EDGE('',*,*,#7216,.T.);
#9249=ORIENTED_EDGE('',*,*,#7215,.F.);
#9250=ORIENTED_EDGE('',*,*,#7214,.T.);
#9251=ORIENTED_EDGE('',*,*,#7213,.T.);
#9252=ORIENTED_EDGE('',*,*,#7210,.T.);
#9253=ORIENTED_EDGE('',*,*,#7207,.T.);
#9254=ORIENTED_EDGE('',*,*,#7204,.T.);
#9255=ORIENTED_EDGE('',*,*,#7201,.T.);
#9256=ORIENTED_EDGE('',*,*,#7216,.F.);
#9257=ORIENTED_EDGE('',*,*,#7199,.T.);
#9258=ORIENTED_EDGE('',*,*,#7202,.T.);
#9259=ORIENTED_EDGE('',*,*,#7205,.T.);
#9260=ORIENTED_EDGE('',*,*,#7208,.T.);
#9261=ORIENTED_EDGE('',*,*,#7217,.F.);
#9262=ORIENTED_EDGE('',*,*,#7218,.T.);
#9263=ORIENTED_EDGE('',*,*,#7219,.F.);
#9264=ORIENTED_EDGE('',*,*,#7220,.F.);
#9265=ORIENTED_EDGE('',*,*,#7221,.F.);
#9266=ORIENTED_EDGE('',*,*,#7222,.T.);
#9267=ORIENTED_EDGE('',*,*,#7223,.F.);
#9268=ORIENTED_EDGE('',*,*,#7222,.F.);
#9269=ORIENTED_EDGE('',*,*,#7224,.F.);
#9270=ORIENTED_EDGE('',*,*,#7218,.F.);
#9271=ORIENTED_EDGE('',*,*,#7225,.F.);
#9272=ORIENTED_EDGE('',*,*,#7220,.T.);
#9273=ORIENTED_EDGE('',*,*,#7226,.F.);
#9274=ORIENTED_EDGE('',*,*,#7227,.F.);
#9275=ORIENTED_EDGE('',*,*,#7228,.F.);
#9276=ORIENTED_EDGE('',*,*,#7229,.F.);
#9277=ORIENTED_EDGE('',*,*,#7230,.T.);
#9278=ORIENTED_EDGE('',*,*,#7231,.F.);
#9279=ORIENTED_EDGE('',*,*,#7232,.F.);
#9280=ORIENTED_EDGE('',*,*,#7233,.F.);
#9281=ORIENTED_EDGE('',*,*,#7234,.F.);
#9282=ORIENTED_EDGE('',*,*,#7235,.T.);
#9283=ORIENTED_EDGE('',*,*,#7236,.F.);
#9284=ORIENTED_EDGE('',*,*,#7237,.F.);
#9285=ORIENTED_EDGE('',*,*,#7238,.T.);
#9286=ORIENTED_EDGE('',*,*,#7239,.F.);
#9287=ORIENTED_EDGE('',*,*,#7240,.F.);
#9288=ORIENTED_EDGE('',*,*,#7241,.F.);
#9289=ORIENTED_EDGE('',*,*,#7230,.F.);
#9290=ORIENTED_EDGE('',*,*,#7242,.F.);
#9291=ORIENTED_EDGE('',*,*,#7243,.F.);
#9292=ORIENTED_EDGE('',*,*,#7244,.F.);
#9293=ORIENTED_EDGE('',*,*,#7245,.T.);
#9294=ORIENTED_EDGE('',*,*,#7246,.F.);
#9295=ORIENTED_EDGE('',*,*,#7247,.F.);
#9296=ORIENTED_EDGE('',*,*,#7248,.T.);
#9297=ORIENTED_EDGE('',*,*,#7242,.T.);
#9298=ORIENTED_EDGE('',*,*,#7229,.T.);
#9299=ORIENTED_EDGE('',*,*,#7249,.F.);
#9300=ORIENTED_EDGE('',*,*,#7250,.F.);
#9301=ORIENTED_EDGE('',*,*,#7251,.F.);
#9302=ORIENTED_EDGE('',*,*,#7252,.F.);
#9303=ORIENTED_EDGE('',*,*,#7253,.F.);
#9304=ORIENTED_EDGE('',*,*,#7254,.F.);
#9305=ORIENTED_EDGE('',*,*,#7255,.F.);
#9306=ORIENTED_EDGE('',*,*,#7228,.T.);
#9307=ORIENTED_EDGE('',*,*,#7256,.T.);
#9308=ORIENTED_EDGE('',*,*,#7257,.F.);
#9309=ORIENTED_EDGE('',*,*,#7249,.T.);
#9310=ORIENTED_EDGE('',*,*,#7227,.T.);
#9311=ORIENTED_EDGE('',*,*,#7258,.F.);
#9312=ORIENTED_EDGE('',*,*,#7256,.F.);
#9313=ORIENTED_EDGE('',*,*,#7247,.T.);
#9314=ORIENTED_EDGE('',*,*,#7259,.T.);
#9315=ORIENTED_EDGE('',*,*,#7260,.T.);
#9316=ORIENTED_EDGE('',*,*,#7261,.F.);
#9317=ORIENTED_EDGE('',*,*,#7238,.F.);
#9318=ORIENTED_EDGE('',*,*,#7262,.T.);
#9319=ORIENTED_EDGE('',*,*,#7263,.F.);
#9320=ORIENTED_EDGE('',*,*,#7264,.F.);
#9321=ORIENTED_EDGE('',*,*,#7245,.F.);
#9322=ORIENTED_EDGE('',*,*,#7265,.F.);
#9323=ORIENTED_EDGE('',*,*,#7266,.F.);
#9324=ORIENTED_EDGE('',*,*,#7254,.T.);
#9325=ORIENTED_EDGE('',*,*,#7232,.T.);
#9326=ORIENTED_EDGE('',*,*,#7267,.T.);
#9327=ORIENTED_EDGE('',*,*,#7268,.F.);
#9328=ORIENTED_EDGE('',*,*,#7269,.F.);
#9329=ORIENTED_EDGE('',*,*,#7240,.T.);
#9330=ORIENTED_EDGE('',*,*,#7270,.F.);
#9331=ORIENTED_EDGE('',*,*,#7263,.T.);
#9332=ORIENTED_EDGE('',*,*,#7271,.T.);
#9333=ORIENTED_EDGE('',*,*,#7236,.T.);
#9334=ORIENTED_EDGE('',*,*,#7272,.F.);
#9335=ORIENTED_EDGE('',*,*,#7273,.F.);
#9336=ORIENTED_EDGE('',*,*,#7274,.T.);
#9337=ORIENTED_EDGE('',*,*,#7233,.T.);
#9338=ORIENTED_EDGE('',*,*,#7269,.T.);
#9339=ORIENTED_EDGE('',*,*,#7275,.F.);
#9340=ORIENTED_EDGE('',*,*,#7239,.T.);
#9341=ORIENTED_EDGE('',*,*,#7264,.T.);
#9342=ORIENTED_EDGE('',*,*,#7270,.T.);
#9343=ORIENTED_EDGE('',*,*,#7234,.T.);
#9344=ORIENTED_EDGE('',*,*,#7275,.T.);
#9345=ORIENTED_EDGE('',*,*,#7268,.T.);
#9346=ORIENTED_EDGE('',*,*,#7276,.T.);
#9347=ORIENTED_EDGE('',*,*,#7248,.F.);
#9348=ORIENTED_EDGE('',*,*,#7261,.T.);
#9349=ORIENTED_EDGE('',*,*,#7277,.T.);
#9350=ORIENTED_EDGE('',*,*,#7272,.T.);
#9351=ORIENTED_EDGE('',*,*,#7235,.F.);
#9352=ORIENTED_EDGE('',*,*,#7278,.T.);
#9353=ORIENTED_EDGE('',*,*,#7279,.T.);
#9354=ORIENTED_EDGE('',*,*,#7251,.T.);
#9355=ORIENTED_EDGE('',*,*,#7280,.T.);
#9356=ORIENTED_EDGE('',*,*,#7281,.F.);
#9357=ORIENTED_EDGE('',*,*,#7282,.T.);
#9358=ORIENTED_EDGE('',*,*,#7280,.F.);
#9359=ORIENTED_EDGE('',*,*,#7282,.F.);
#9360=ORIENTED_EDGE('',*,*,#7224,.T.);
#9361=ORIENTED_EDGE('',*,*,#7221,.T.);
#9362=ORIENTED_EDGE('',*,*,#7225,.T.);
#9363=ORIENTED_EDGE('',*,*,#7219,.T.);
#9364=ORIENTED_EDGE('',*,*,#7217,.T.);
#9365=ORIENTED_EDGE('',*,*,#7283,.F.);
#9366=ORIENTED_EDGE('',*,*,#7252,.T.);
#9367=ORIENTED_EDGE('',*,*,#7279,.F.);
#9368=ORIENTED_EDGE('',*,*,#7284,.F.);
#9369=ORIENTED_EDGE('',*,*,#7231,.T.);
#9370=ORIENTED_EDGE('',*,*,#7241,.T.);
#9371=ORIENTED_EDGE('',*,*,#7271,.F.);
#9372=ORIENTED_EDGE('',*,*,#7262,.F.);
#9373=ORIENTED_EDGE('',*,*,#7285,.F.);
#9374=ORIENTED_EDGE('',*,*,#7284,.T.);
#9375=ORIENTED_EDGE('',*,*,#7278,.F.);
#9376=ORIENTED_EDGE('',*,*,#7276,.F.);
#9377=ORIENTED_EDGE('',*,*,#7267,.F.);
#9378=ORIENTED_EDGE('',*,*,#7226,.T.);
#9379=ORIENTED_EDGE('',*,*,#7250,.T.);
#9380=ORIENTED_EDGE('',*,*,#7257,.T.);
#9381=ORIENTED_EDGE('',*,*,#7258,.T.);
#9382=ORIENTED_EDGE('',*,*,#7243,.T.);
#9383=ORIENTED_EDGE('',*,*,#7255,.T.);
#9384=ORIENTED_EDGE('',*,*,#7266,.T.);
#9385=ORIENTED_EDGE('',*,*,#7286,.T.);
#9386=ORIENTED_EDGE('',*,*,#7287,.T.);
#9387=ORIENTED_EDGE('',*,*,#7273,.T.);
#9388=ORIENTED_EDGE('',*,*,#7277,.F.);
#9389=ORIENTED_EDGE('',*,*,#7260,.F.);
#9390=ORIENTED_EDGE('',*,*,#7223,.T.);
#9391=ORIENTED_EDGE('',*,*,#7244,.T.);
#9392=ORIENTED_EDGE('',*,*,#7286,.F.);
#9393=ORIENTED_EDGE('',*,*,#7265,.T.);
#9394=ORIENTED_EDGE('',*,*,#7246,.T.);
#9395=ORIENTED_EDGE('',*,*,#7253,.T.);
#9396=ORIENTED_EDGE('',*,*,#7283,.T.);
#9397=ORIENTED_EDGE('',*,*,#7285,.T.);
#9398=ORIENTED_EDGE('',*,*,#7237,.T.);
#9399=ORIENTED_EDGE('',*,*,#7274,.F.);
#9400=ORIENTED_EDGE('',*,*,#7287,.F.);
#9401=ORIENTED_EDGE('',*,*,#7259,.F.);
#9402=ORIENTED_EDGE('',*,*,#7281,.T.);
#9403=ORIENTED_EDGE('',*,*,#7288,.F.);
#9404=ORIENTED_EDGE('',*,*,#7289,.T.);
#9405=ORIENTED_EDGE('',*,*,#7290,.T.);
#9406=ORIENTED_EDGE('',*,*,#7289,.F.);
#9407=ORIENTED_EDGE('',*,*,#7291,.F.);
#9408=ORIENTED_EDGE('',*,*,#7292,.T.);
#9409=ORIENTED_EDGE('',*,*,#7293,.T.);
#9410=ORIENTED_EDGE('',*,*,#7292,.F.);
#9411=ORIENTED_EDGE('',*,*,#7291,.T.);
#9412=ORIENTED_EDGE('',*,*,#7288,.T.);
#9413=ORIENTED_EDGE('',*,*,#7293,.F.);
#9414=ORIENTED_EDGE('',*,*,#7290,.F.);
#9415=ORIENTED_EDGE('',*,*,#7294,.F.);
#9416=ORIENTED_EDGE('',*,*,#7295,.T.);
#9417=ORIENTED_EDGE('',*,*,#7296,.T.);
#9418=ORIENTED_EDGE('',*,*,#7295,.F.);
#9419=ORIENTED_EDGE('',*,*,#7294,.T.);
#9420=ORIENTED_EDGE('',*,*,#7296,.F.);
#9421=ORIENTED_EDGE('',*,*,#7297,.F.);
#9422=ORIENTED_EDGE('',*,*,#7298,.T.);
#9423=ORIENTED_EDGE('',*,*,#7299,.T.);
#9424=ORIENTED_EDGE('',*,*,#7298,.F.);
#9425=ORIENTED_EDGE('',*,*,#7297,.T.);
#9426=ORIENTED_EDGE('',*,*,#7299,.F.);
#9427=ORIENTED_EDGE('',*,*,#7300,.F.);
#9428=ORIENTED_EDGE('',*,*,#7301,.T.);
#9429=ORIENTED_EDGE('',*,*,#7302,.F.);
#9430=ORIENTED_EDGE('',*,*,#7301,.F.);
#9431=ORIENTED_EDGE('',*,*,#7300,.T.);
#9432=ORIENTED_EDGE('',*,*,#7303,.F.);
#9433=ORIENTED_EDGE('',*,*,#7304,.F.);
#9434=ORIENTED_EDGE('',*,*,#7305,.T.);
#9435=ORIENTED_EDGE('',*,*,#7306,.F.);
#9436=ORIENTED_EDGE('',*,*,#7305,.F.);
#9437=ORIENTED_EDGE('',*,*,#7304,.T.);
#9438=ORIENTED_EDGE('',*,*,#7307,.F.);
#9439=ORIENTED_EDGE('',*,*,#7308,.F.);
#9440=ORIENTED_EDGE('',*,*,#7309,.T.);
#9441=ORIENTED_EDGE('',*,*,#7310,.F.);
#9442=ORIENTED_EDGE('',*,*,#7309,.F.);
#9443=ORIENTED_EDGE('',*,*,#7308,.T.);
#9444=ORIENTED_EDGE('',*,*,#7311,.F.);
#9445=ORIENTED_EDGE('',*,*,#7312,.F.);
#9446=ORIENTED_EDGE('',*,*,#7313,.T.);
#9447=ORIENTED_EDGE('',*,*,#7314,.F.);
#9448=ORIENTED_EDGE('',*,*,#7313,.F.);
#9449=ORIENTED_EDGE('',*,*,#7312,.T.);
#9450=ORIENTED_EDGE('',*,*,#7315,.F.);
#9451=ORIENTED_EDGE('',*,*,#7316,.F.);
#9452=ORIENTED_EDGE('',*,*,#7317,.T.);
#9453=ORIENTED_EDGE('',*,*,#7303,.T.);
#9454=ORIENTED_EDGE('',*,*,#7317,.F.);
#9455=ORIENTED_EDGE('',*,*,#7318,.F.);
#9456=ORIENTED_EDGE('',*,*,#7319,.T.);
#9457=ORIENTED_EDGE('',*,*,#7307,.T.);
#9458=ORIENTED_EDGE('',*,*,#7319,.F.);
#9459=ORIENTED_EDGE('',*,*,#7320,.F.);
#9460=ORIENTED_EDGE('',*,*,#7321,.T.);
#9461=ORIENTED_EDGE('',*,*,#7311,.T.);
#9462=ORIENTED_EDGE('',*,*,#7321,.F.);
#9463=ORIENTED_EDGE('',*,*,#7322,.F.);
#9464=ORIENTED_EDGE('',*,*,#7323,.T.);
#9465=ORIENTED_EDGE('',*,*,#7315,.T.);
#9466=ORIENTED_EDGE('',*,*,#7323,.F.);
#9467=ORIENTED_EDGE('',*,*,#7324,.T.);
#9468=ORIENTED_EDGE('',*,*,#7325,.T.);
#9469=ORIENTED_EDGE('',*,*,#7326,.F.);
#9470=ORIENTED_EDGE('',*,*,#7327,.F.);
#9471=ORIENTED_EDGE('',*,*,#7328,.T.);
#9472=ORIENTED_EDGE('',*,*,#7327,.T.);
#9473=ORIENTED_EDGE('',*,*,#7329,.F.);
#9474=ORIENTED_EDGE('',*,*,#7330,.F.);
#9475=ORIENTED_EDGE('',*,*,#7331,.T.);
#9476=ORIENTED_EDGE('',*,*,#7330,.T.);
#9477=ORIENTED_EDGE('',*,*,#7332,.F.);
#9478=ORIENTED_EDGE('',*,*,#7333,.F.);
#9479=ORIENTED_EDGE('',*,*,#7334,.T.);
#9480=ORIENTED_EDGE('',*,*,#7333,.T.);
#9481=ORIENTED_EDGE('',*,*,#7335,.F.);
#9482=ORIENTED_EDGE('',*,*,#7336,.F.);
#9483=ORIENTED_EDGE('',*,*,#7337,.T.);
#9484=ORIENTED_EDGE('',*,*,#7336,.T.);
#9485=ORIENTED_EDGE('',*,*,#7338,.F.);
#9486=ORIENTED_EDGE('',*,*,#7339,.F.);
#9487=ORIENTED_EDGE('',*,*,#7314,.T.);
#9488=ORIENTED_EDGE('',*,*,#7310,.T.);
#9489=ORIENTED_EDGE('',*,*,#7306,.T.);
#9490=ORIENTED_EDGE('',*,*,#7302,.T.);
#9491=ORIENTED_EDGE('',*,*,#7340,.T.);
#9492=ORIENTED_EDGE('',*,*,#7339,.T.);
#9493=ORIENTED_EDGE('',*,*,#7341,.F.);
#9494=ORIENTED_EDGE('',*,*,#7342,.F.);
#9495=ORIENTED_EDGE('',*,*,#7343,.T.);
#9496=ORIENTED_EDGE('',*,*,#7342,.T.);
#9497=ORIENTED_EDGE('',*,*,#7344,.F.);
#9498=ORIENTED_EDGE('',*,*,#7345,.F.);
#9499=ORIENTED_EDGE('',*,*,#7346,.T.);
#9500=ORIENTED_EDGE('',*,*,#7345,.T.);
#9501=ORIENTED_EDGE('',*,*,#7347,.F.);
#9502=ORIENTED_EDGE('',*,*,#7348,.F.);
#9503=ORIENTED_EDGE('',*,*,#7349,.T.);
#9504=ORIENTED_EDGE('',*,*,#7348,.T.);
#9505=ORIENTED_EDGE('',*,*,#7350,.F.);
#9506=ORIENTED_EDGE('',*,*,#7351,.F.);
#9507=ORIENTED_EDGE('',*,*,#7352,.T.);
#9508=ORIENTED_EDGE('',*,*,#7351,.T.);
#9509=ORIENTED_EDGE('',*,*,#7353,.F.);
#9510=ORIENTED_EDGE('',*,*,#7354,.F.);
#9511=ORIENTED_EDGE('',*,*,#7355,.T.);
#9512=ORIENTED_EDGE('',*,*,#7354,.T.);
#9513=ORIENTED_EDGE('',*,*,#7356,.F.);
#9514=ORIENTED_EDGE('',*,*,#7357,.F.);
#9515=ORIENTED_EDGE('',*,*,#7316,.T.);
#9516=ORIENTED_EDGE('',*,*,#7318,.T.);
#9517=ORIENTED_EDGE('',*,*,#7320,.T.);
#9518=ORIENTED_EDGE('',*,*,#7322,.T.);
#9519=ORIENTED_EDGE('',*,*,#7358,.T.);
#9520=ORIENTED_EDGE('',*,*,#7357,.T.);
#9521=ORIENTED_EDGE('',*,*,#7359,.F.);
#9522=ORIENTED_EDGE('',*,*,#7325,.F.);
#9523=ORIENTED_EDGE('',*,*,#7359,.T.);
#9524=ORIENTED_EDGE('',*,*,#7356,.T.);
#9525=ORIENTED_EDGE('',*,*,#7353,.T.);
#9526=ORIENTED_EDGE('',*,*,#7350,.T.);
#9527=ORIENTED_EDGE('',*,*,#7347,.T.);
#9528=ORIENTED_EDGE('',*,*,#7344,.T.);
#9529=ORIENTED_EDGE('',*,*,#7341,.T.);
#9530=ORIENTED_EDGE('',*,*,#7338,.T.);
#9531=ORIENTED_EDGE('',*,*,#7335,.T.);
#9532=ORIENTED_EDGE('',*,*,#7332,.T.);
#9533=ORIENTED_EDGE('',*,*,#7329,.T.);
#9534=ORIENTED_EDGE('',*,*,#7326,.T.);
#9535=ORIENTED_EDGE('',*,*,#7358,.F.);
#9536=ORIENTED_EDGE('',*,*,#7324,.F.);
#9537=ORIENTED_EDGE('',*,*,#7328,.F.);
#9538=ORIENTED_EDGE('',*,*,#7331,.F.);
#9539=ORIENTED_EDGE('',*,*,#7334,.F.);
#9540=ORIENTED_EDGE('',*,*,#7337,.F.);
#9541=ORIENTED_EDGE('',*,*,#7340,.F.);
#9542=ORIENTED_EDGE('',*,*,#7343,.F.);
#9543=ORIENTED_EDGE('',*,*,#7346,.F.);
#9544=ORIENTED_EDGE('',*,*,#7349,.F.);
#9545=ORIENTED_EDGE('',*,*,#7352,.F.);
#9546=ORIENTED_EDGE('',*,*,#7355,.F.);
#9547=ORIENTED_EDGE('',*,*,#7360,.F.);
#9548=ORIENTED_EDGE('',*,*,#7361,.F.);
#9549=ORIENTED_EDGE('',*,*,#7362,.T.);
#9550=ORIENTED_EDGE('',*,*,#7363,.F.);
#9551=ORIENTED_EDGE('',*,*,#7364,.F.);
#9552=ORIENTED_EDGE('',*,*,#7362,.F.);
#9553=ORIENTED_EDGE('',*,*,#7363,.T.);
#9554=ORIENTED_EDGE('',*,*,#7364,.T.);
#9555=ORIENTED_EDGE('',*,*,#7365,.T.);
#9556=ORIENTED_EDGE('',*,*,#7366,.T.);
#9557=ORIENTED_EDGE('',*,*,#7365,.F.);
#9558=ORIENTED_EDGE('',*,*,#7367,.T.);
#9559=ORIENTED_EDGE('',*,*,#7368,.T.);
#9560=ORIENTED_EDGE('',*,*,#7369,.F.);
#9561=ORIENTED_EDGE('',*,*,#7368,.F.);
#9562=ORIENTED_EDGE('',*,*,#7369,.T.);
#9563=ORIENTED_EDGE('',*,*,#7370,.T.);
#9564=ORIENTED_EDGE('',*,*,#7371,.F.);
#9565=ORIENTED_EDGE('',*,*,#7370,.F.);
#9566=ORIENTED_EDGE('',*,*,#7366,.F.);
#9567=ORIENTED_EDGE('',*,*,#7371,.T.);
#9568=ORIENTED_EDGE('',*,*,#7372,.F.);
#9569=ORIENTED_EDGE('',*,*,#7373,.T.);
#9570=ORIENTED_EDGE('',*,*,#7360,.T.);
#9571=ORIENTED_EDGE('',*,*,#7361,.T.);
#9572=ORIENTED_EDGE('',*,*,#7373,.F.);
#9573=ORIENTED_EDGE('',*,*,#7372,.T.);
#9574=ORIENTED_EDGE('',*,*,#7374,.F.);
#9575=ORIENTED_EDGE('',*,*,#7374,.T.);
#9576=ORIENTED_EDGE('',*,*,#7375,.T.);
#9577=ORIENTED_EDGE('',*,*,#7367,.F.);
#9578=ORIENTED_EDGE('',*,*,#7375,.F.);
#9579=ORIENTED_EDGE('',*,*,#7376,.F.);
#9580=ORIENTED_EDGE('',*,*,#7377,.F.);
#9581=ORIENTED_EDGE('',*,*,#7378,.T.);
#9582=ORIENTED_EDGE('',*,*,#7379,.F.);
#9583=ORIENTED_EDGE('',*,*,#7380,.F.);
#9584=ORIENTED_EDGE('',*,*,#7378,.F.);
#9585=ORIENTED_EDGE('',*,*,#7381,.T.);
#9586=ORIENTED_EDGE('',*,*,#7382,.T.);
#9587=ORIENTED_EDGE('',*,*,#7379,.T.);
#9588=ORIENTED_EDGE('',*,*,#7380,.T.);
#9589=ORIENTED_EDGE('',*,*,#7382,.F.);
#9590=ORIENTED_EDGE('',*,*,#7383,.F.);
#9591=ORIENTED_EDGE('',*,*,#7384,.T.);
#9592=ORIENTED_EDGE('',*,*,#7385,.F.);
#9593=ORIENTED_EDGE('',*,*,#7386,.T.);
#9594=ORIENTED_EDGE('',*,*,#7383,.T.);
#9595=ORIENTED_EDGE('',*,*,#7386,.F.);
#9596=ORIENTED_EDGE('',*,*,#7387,.F.);
#9597=ORIENTED_EDGE('',*,*,#7388,.T.);
#9598=ORIENTED_EDGE('',*,*,#7385,.T.);
#9599=ORIENTED_EDGE('',*,*,#7388,.F.);
#9600=ORIENTED_EDGE('',*,*,#7389,.F.);
#9601=ORIENTED_EDGE('',*,*,#7390,.T.);
#9602=ORIENTED_EDGE('',*,*,#7387,.T.);
#9603=ORIENTED_EDGE('',*,*,#7390,.F.);
#9604=ORIENTED_EDGE('',*,*,#7389,.T.);
#9605=ORIENTED_EDGE('',*,*,#7381,.F.);
#9606=ORIENTED_EDGE('',*,*,#7376,.T.);
#9607=ORIENTED_EDGE('',*,*,#7377,.T.);
#9608=ORIENTED_EDGE('',*,*,#7391,.T.);
#9609=ORIENTED_EDGE('',*,*,#7384,.F.);
#9610=ORIENTED_EDGE('',*,*,#7391,.F.);
#9611=ORIENTED_EDGE('',*,*,#7392,.T.);
#9612=ORIENTED_EDGE('',*,*,#7392,.F.);
#9613=ORIENTED_EDGE('',*,*,#7393,.T.);
#9614=ORIENTED_EDGE('',*,*,#7393,.F.);
#9615=ORIENTED_EDGE('',*,*,#7394,.T.);
#9616=ORIENTED_EDGE('',*,*,#7394,.F.);
#9617=ORIENTED_EDGE('',*,*,#7395,.T.);
#9618=ORIENTED_EDGE('',*,*,#7395,.F.);
#9619=ORIENTED_EDGE('',*,*,#7396,.T.);
#9620=ORIENTED_EDGE('',*,*,#7396,.F.);
#9621=ORIENTED_EDGE('',*,*,#7397,.T.);
#9622=ORIENTED_EDGE('',*,*,#7397,.F.);
#9623=ORIENTED_EDGE('',*,*,#7398,.T.);
#9624=ORIENTED_EDGE('',*,*,#7398,.F.);
#9625=ORIENTED_EDGE('',*,*,#7399,.F.);
#9626=ORIENTED_EDGE('',*,*,#7400,.F.);
#9627=ORIENTED_EDGE('',*,*,#7401,.F.);
#9628=ORIENTED_EDGE('',*,*,#7402,.F.);
#9629=ORIENTED_EDGE('',*,*,#7401,.T.);
#9630=ORIENTED_EDGE('',*,*,#7403,.F.);
#9631=ORIENTED_EDGE('',*,*,#7404,.T.);
#9632=ORIENTED_EDGE('',*,*,#7405,.F.);
#9633=ORIENTED_EDGE('',*,*,#7406,.T.);
#9634=ORIENTED_EDGE('',*,*,#7407,.F.);
#9635=ORIENTED_EDGE('',*,*,#7408,.T.);
#9636=ORIENTED_EDGE('',*,*,#7409,.F.);
#9637=ORIENTED_EDGE('',*,*,#7408,.F.);
#9638=ORIENTED_EDGE('',*,*,#7410,.F.);
#9639=ORIENTED_EDGE('',*,*,#7411,.T.);
#9640=ORIENTED_EDGE('',*,*,#7412,.F.);
#9641=ORIENTED_EDGE('',*,*,#7413,.T.);
#9642=ORIENTED_EDGE('',*,*,#7414,.F.);
#9643=ORIENTED_EDGE('',*,*,#7415,.T.);
#9644=ORIENTED_EDGE('',*,*,#7416,.F.);
#9645=ORIENTED_EDGE('',*,*,#7417,.T.);
#9646=ORIENTED_EDGE('',*,*,#7418,.F.);
#9647=ORIENTED_EDGE('',*,*,#7400,.T.);
#9648=ORIENTED_EDGE('',*,*,#7419,.T.);
#9649=ORIENTED_EDGE('',*,*,#7420,.T.);
#9650=ORIENTED_EDGE('',*,*,#7403,.T.);
#9651=ORIENTED_EDGE('',*,*,#7421,.F.);
#9652=ORIENTED_EDGE('',*,*,#7422,.F.);
#9653=ORIENTED_EDGE('',*,*,#7404,.F.);
#9654=ORIENTED_EDGE('',*,*,#7420,.F.);
#9655=ORIENTED_EDGE('',*,*,#7422,.T.);
#9656=ORIENTED_EDGE('',*,*,#7423,.T.);
#9657=ORIENTED_EDGE('',*,*,#7424,.T.);
#9658=ORIENTED_EDGE('',*,*,#7405,.T.);
#9659=ORIENTED_EDGE('',*,*,#7425,.F.);
#9660=ORIENTED_EDGE('',*,*,#7426,.F.);
#9661=ORIENTED_EDGE('',*,*,#7406,.F.);
#9662=ORIENTED_EDGE('',*,*,#7424,.F.);
#9663=ORIENTED_EDGE('',*,*,#7426,.T.);
#9664=ORIENTED_EDGE('',*,*,#7427,.T.);
#9665=ORIENTED_EDGE('',*,*,#7428,.T.);
#9666=ORIENTED_EDGE('',*,*,#7429,.T.);
#9667=ORIENTED_EDGE('',*,*,#7410,.T.);
#9668=ORIENTED_EDGE('',*,*,#7407,.T.);
#9669=ORIENTED_EDGE('',*,*,#7430,.F.);
#9670=ORIENTED_EDGE('',*,*,#7431,.F.);
#9671=ORIENTED_EDGE('',*,*,#7411,.F.);
#9672=ORIENTED_EDGE('',*,*,#7429,.F.);
#9673=ORIENTED_EDGE('',*,*,#7431,.T.);
#9674=ORIENTED_EDGE('',*,*,#7432,.T.);
#9675=ORIENTED_EDGE('',*,*,#7433,.T.);
#9676=ORIENTED_EDGE('',*,*,#7412,.T.);
#9677=ORIENTED_EDGE('',*,*,#7434,.F.);
#9678=ORIENTED_EDGE('',*,*,#7435,.F.);
#9679=ORIENTED_EDGE('',*,*,#7413,.F.);
#9680=ORIENTED_EDGE('',*,*,#7433,.F.);
#9681=ORIENTED_EDGE('',*,*,#7435,.T.);
#9682=ORIENTED_EDGE('',*,*,#7436,.T.);
#9683=ORIENTED_EDGE('',*,*,#7437,.T.);
#9684=ORIENTED_EDGE('',*,*,#7414,.T.);
#9685=ORIENTED_EDGE('',*,*,#7415,.F.);
#9686=ORIENTED_EDGE('',*,*,#7437,.F.);
#9687=ORIENTED_EDGE('',*,*,#7438,.F.);
#9688=ORIENTED_EDGE('',*,*,#7439,.F.);
#9689=ORIENTED_EDGE('',*,*,#7440,.F.);
#9690=ORIENTED_EDGE('',*,*,#7441,.T.);
#9691=ORIENTED_EDGE('',*,*,#7427,.F.);
#9692=ORIENTED_EDGE('',*,*,#7425,.T.);
#9693=ORIENTED_EDGE('',*,*,#7423,.F.);
#9694=ORIENTED_EDGE('',*,*,#7421,.T.);
#9695=ORIENTED_EDGE('',*,*,#7419,.F.);
#9696=ORIENTED_EDGE('',*,*,#7399,.T.);
#9697=ORIENTED_EDGE('',*,*,#7442,.F.);
#9698=ORIENTED_EDGE('',*,*,#7443,.T.);
#9699=ORIENTED_EDGE('',*,*,#7444,.F.);
#9700=ORIENTED_EDGE('',*,*,#7438,.T.);
#9701=ORIENTED_EDGE('',*,*,#7436,.F.);
#9702=ORIENTED_EDGE('',*,*,#7434,.T.);
#9703=ORIENTED_EDGE('',*,*,#7432,.F.);
#9704=ORIENTED_EDGE('',*,*,#7430,.T.);
#9705=ORIENTED_EDGE('',*,*,#7428,.F.);
#9706=ORIENTED_EDGE('',*,*,#7441,.F.);
#9707=ORIENTED_EDGE('',*,*,#7402,.T.);
#9708=ORIENTED_EDGE('',*,*,#7418,.T.);
#9709=ORIENTED_EDGE('',*,*,#7445,.T.);
#9710=ORIENTED_EDGE('',*,*,#7442,.T.);
#9711=ORIENTED_EDGE('',*,*,#7417,.F.);
#9712=ORIENTED_EDGE('',*,*,#7446,.F.);
#9713=ORIENTED_EDGE('',*,*,#7443,.F.);
#9714=ORIENTED_EDGE('',*,*,#7445,.F.);
#9715=ORIENTED_EDGE('',*,*,#7409,.T.);
#9716=ORIENTED_EDGE('',*,*,#7440,.T.);
#9717=ORIENTED_EDGE('',*,*,#7439,.T.);
#9718=ORIENTED_EDGE('',*,*,#7444,.T.);
#9719=ORIENTED_EDGE('',*,*,#7446,.T.);
#9720=ORIENTED_EDGE('',*,*,#7416,.T.);
#9721=ORIENTED_EDGE('',*,*,#7447,.F.);
#9722=ORIENTED_EDGE('',*,*,#7448,.T.);
#9723=ORIENTED_EDGE('',*,*,#7449,.F.);
#9724=ORIENTED_EDGE('',*,*,#7450,.T.);
#9725=ORIENTED_EDGE('',*,*,#7447,.T.);
#9726=ORIENTED_EDGE('',*,*,#7450,.F.);
#9727=ORIENTED_EDGE('',*,*,#7449,.T.);
#9728=ORIENTED_EDGE('',*,*,#7451,.F.);
#9729=ORIENTED_EDGE('',*,*,#7451,.T.);
#9730=ORIENTED_EDGE('',*,*,#7452,.T.);
#9731=ORIENTED_EDGE('',*,*,#7448,.F.);
#9732=ORIENTED_EDGE('',*,*,#7452,.F.);
#9733=ORIENTED_EDGE('',*,*,#7453,.F.);
#9734=ORIENTED_EDGE('',*,*,#7454,.T.);
#9735=ORIENTED_EDGE('',*,*,#7455,.F.);
#9736=ORIENTED_EDGE('',*,*,#7456,.T.);
#9737=ORIENTED_EDGE('',*,*,#7453,.T.);
#9738=ORIENTED_EDGE('',*,*,#7456,.F.);
#9739=ORIENTED_EDGE('',*,*,#7455,.T.);
#9740=ORIENTED_EDGE('',*,*,#7457,.F.);
#9741=ORIENTED_EDGE('',*,*,#7457,.T.);
#9742=ORIENTED_EDGE('',*,*,#7458,.T.);
#9743=ORIENTED_EDGE('',*,*,#7454,.F.);
#9744=ORIENTED_EDGE('',*,*,#7458,.F.);
#9745=ORIENTED_EDGE('',*,*,#7459,.F.);
#9746=ORIENTED_EDGE('',*,*,#7460,.F.);
#9747=ORIENTED_EDGE('',*,*,#7461,.T.);
#9748=ORIENTED_EDGE('',*,*,#7459,.T.);
#9749=ORIENTED_EDGE('',*,*,#7461,.F.);
#9750=ORIENTED_EDGE('',*,*,#7462,.F.);
#9751=ORIENTED_EDGE('',*,*,#7463,.T.);
#9752=ORIENTED_EDGE('',*,*,#7460,.T.);
#9753=ORIENTED_EDGE('',*,*,#7463,.F.);
#9754=ORIENTED_EDGE('',*,*,#7464,.F.);
#9755=ORIENTED_EDGE('',*,*,#7465,.T.);
#9756=ORIENTED_EDGE('',*,*,#7462,.T.);
#9757=ORIENTED_EDGE('',*,*,#7465,.F.);
#9758=ORIENTED_EDGE('',*,*,#7464,.T.);
#9759=ORIENTED_EDGE('',*,*,#7466,.F.);
#9760=ORIENTED_EDGE('',*,*,#7467,.F.);
#9761=ORIENTED_EDGE('',*,*,#7468,.T.);
#9762=ORIENTED_EDGE('',*,*,#7466,.T.);
#9763=ORIENTED_EDGE('',*,*,#7468,.F.);
#9764=ORIENTED_EDGE('',*,*,#7469,.F.);
#9765=ORIENTED_EDGE('',*,*,#7470,.T.);
#9766=ORIENTED_EDGE('',*,*,#7467,.T.);
#9767=ORIENTED_EDGE('',*,*,#7470,.F.);
#9768=ORIENTED_EDGE('',*,*,#7471,.F.);
#9769=ORIENTED_EDGE('',*,*,#7472,.T.);
#9770=ORIENTED_EDGE('',*,*,#7469,.T.);
#9771=ORIENTED_EDGE('',*,*,#7472,.F.);
#9772=ORIENTED_EDGE('',*,*,#7471,.T.);
#9773=ORIENTED_EDGE('',*,*,#7473,.T.);
#9774=ORIENTED_EDGE('',*,*,#7474,.T.);
#9775=ORIENTED_EDGE('',*,*,#7475,.T.);
#9776=ORIENTED_EDGE('',*,*,#7476,.F.);
#9777=ORIENTED_EDGE('',*,*,#7477,.T.);
#9778=ORIENTED_EDGE('',*,*,#7478,.T.);
#9779=ORIENTED_EDGE('',*,*,#7479,.T.);
#9780=ORIENTED_EDGE('',*,*,#7474,.F.);
#9781=ORIENTED_EDGE('',*,*,#7480,.T.);
#9782=ORIENTED_EDGE('',*,*,#7481,.T.);
#9783=ORIENTED_EDGE('',*,*,#7482,.T.);
#9784=ORIENTED_EDGE('',*,*,#7478,.F.);
#9785=ORIENTED_EDGE('',*,*,#7483,.T.);
#9786=ORIENTED_EDGE('',*,*,#7484,.T.);
#9787=ORIENTED_EDGE('',*,*,#7485,.T.);
#9788=ORIENTED_EDGE('',*,*,#7481,.F.);
#9789=ORIENTED_EDGE('',*,*,#7486,.T.);
#9790=ORIENTED_EDGE('',*,*,#7487,.T.);
#9791=ORIENTED_EDGE('',*,*,#7488,.T.);
#9792=ORIENTED_EDGE('',*,*,#7484,.F.);
#9793=ORIENTED_EDGE('',*,*,#7489,.T.);
#9794=ORIENTED_EDGE('',*,*,#7476,.T.);
#9795=ORIENTED_EDGE('',*,*,#7490,.T.);
#9796=ORIENTED_EDGE('',*,*,#7487,.F.);
#9797=ORIENTED_EDGE('',*,*,#7489,.F.);
#9798=ORIENTED_EDGE('',*,*,#7486,.F.);
#9799=ORIENTED_EDGE('',*,*,#7483,.F.);
#9800=ORIENTED_EDGE('',*,*,#7480,.F.);
#9801=ORIENTED_EDGE('',*,*,#7477,.F.);
#9802=ORIENTED_EDGE('',*,*,#7473,.F.);
#9803=ORIENTED_EDGE('',*,*,#7490,.F.);
#9804=ORIENTED_EDGE('',*,*,#7475,.F.);
#9805=ORIENTED_EDGE('',*,*,#7479,.F.);
#9806=ORIENTED_EDGE('',*,*,#7482,.F.);
#9807=ORIENTED_EDGE('',*,*,#7485,.F.);
#9808=ORIENTED_EDGE('',*,*,#7488,.F.);
#9809=ORIENTED_EDGE('',*,*,#7491,.F.);
#9810=ORIENTED_EDGE('',*,*,#7492,.T.);
#9811=ORIENTED_EDGE('',*,*,#7493,.F.);
#9812=ORIENTED_EDGE('',*,*,#7492,.F.);
#9813=ORIENTED_EDGE('',*,*,#7494,.F.);
#9814=ORIENTED_EDGE('',*,*,#7495,.T.);
#9815=ORIENTED_EDGE('',*,*,#7496,.F.);
#9816=ORIENTED_EDGE('',*,*,#7495,.F.);
#9817=ORIENTED_EDGE('',*,*,#7497,.F.);
#9818=ORIENTED_EDGE('',*,*,#7498,.T.);
#9819=ORIENTED_EDGE('',*,*,#7499,.F.);
#9820=ORIENTED_EDGE('',*,*,#7498,.F.);
#9821=ORIENTED_EDGE('',*,*,#7500,.F.);
#9822=ORIENTED_EDGE('',*,*,#7501,.T.);
#9823=ORIENTED_EDGE('',*,*,#7502,.F.);
#9824=ORIENTED_EDGE('',*,*,#7501,.F.);
#9825=ORIENTED_EDGE('',*,*,#7503,.F.);
#9826=ORIENTED_EDGE('',*,*,#7504,.T.);
#9827=ORIENTED_EDGE('',*,*,#7505,.F.);
#9828=ORIENTED_EDGE('',*,*,#7504,.F.);
#9829=ORIENTED_EDGE('',*,*,#7506,.T.);
#9830=ORIENTED_EDGE('',*,*,#7507,.T.);
#9831=ORIENTED_EDGE('',*,*,#7508,.F.);
#9832=ORIENTED_EDGE('',*,*,#7509,.F.);
#9833=ORIENTED_EDGE('',*,*,#7505,.T.);
#9834=ORIENTED_EDGE('',*,*,#7510,.T.);
#9835=ORIENTED_EDGE('',*,*,#7509,.T.);
#9836=ORIENTED_EDGE('',*,*,#7511,.F.);
#9837=ORIENTED_EDGE('',*,*,#7512,.F.);
#9838=ORIENTED_EDGE('',*,*,#7513,.T.);
#9839=ORIENTED_EDGE('',*,*,#7512,.T.);
#9840=ORIENTED_EDGE('',*,*,#7514,.F.);
#9841=ORIENTED_EDGE('',*,*,#7515,.F.);
#9842=ORIENTED_EDGE('',*,*,#7503,.T.);
#9843=ORIENTED_EDGE('',*,*,#7516,.T.);
#9844=ORIENTED_EDGE('',*,*,#7515,.T.);
#9845=ORIENTED_EDGE('',*,*,#7517,.F.);
#9846=ORIENTED_EDGE('',*,*,#7507,.F.);
#9847=ORIENTED_EDGE('',*,*,#7516,.F.);
#9848=ORIENTED_EDGE('',*,*,#7506,.F.);
#9849=ORIENTED_EDGE('',*,*,#7510,.F.);
#9850=ORIENTED_EDGE('',*,*,#7513,.F.);
#9851=ORIENTED_EDGE('',*,*,#7518,.F.);
#9852=ORIENTED_EDGE('',*,*,#7519,.T.);
#9853=ORIENTED_EDGE('',*,*,#7520,.F.);
#9854=ORIENTED_EDGE('',*,*,#7519,.F.);
#9855=ORIENTED_EDGE('',*,*,#7521,.F.);
#9856=ORIENTED_EDGE('',*,*,#7522,.T.);
#9857=ORIENTED_EDGE('',*,*,#7523,.F.);
#9858=ORIENTED_EDGE('',*,*,#7522,.F.);
#9859=ORIENTED_EDGE('',*,*,#7524,.F.);
#9860=ORIENTED_EDGE('',*,*,#7525,.T.);
#9861=ORIENTED_EDGE('',*,*,#7526,.F.);
#9862=ORIENTED_EDGE('',*,*,#7525,.F.);
#9863=ORIENTED_EDGE('',*,*,#7527,.F.);
#9864=ORIENTED_EDGE('',*,*,#7528,.T.);
#9865=ORIENTED_EDGE('',*,*,#7529,.F.);
#9866=ORIENTED_EDGE('',*,*,#7528,.F.);
#9867=ORIENTED_EDGE('',*,*,#7530,.F.);
#9868=ORIENTED_EDGE('',*,*,#7531,.F.);
#9869=ORIENTED_EDGE('',*,*,#7532,.F.);
#9870=ORIENTED_EDGE('',*,*,#7533,.F.);
#9871=ORIENTED_EDGE('',*,*,#7531,.T.);
#9872=ORIENTED_EDGE('',*,*,#7534,.T.);
#9873=ORIENTED_EDGE('',*,*,#7535,.T.);
#9874=ORIENTED_EDGE('',*,*,#7536,.T.);
#9875=ORIENTED_EDGE('',*,*,#7537,.T.);
#9876=ORIENTED_EDGE('',*,*,#7538,.T.);
#9877=ORIENTED_EDGE('',*,*,#7529,.T.);
#9878=ORIENTED_EDGE('',*,*,#7526,.T.);
#9879=ORIENTED_EDGE('',*,*,#7523,.T.);
#9880=ORIENTED_EDGE('',*,*,#7520,.T.);
#9881=ORIENTED_EDGE('',*,*,#7502,.T.);
#9882=ORIENTED_EDGE('',*,*,#7499,.T.);
#9883=ORIENTED_EDGE('',*,*,#7496,.T.);
#9884=ORIENTED_EDGE('',*,*,#7493,.T.);
#9885=ORIENTED_EDGE('',*,*,#7530,.T.);
#9886=ORIENTED_EDGE('',*,*,#7539,.T.);
#9887=ORIENTED_EDGE('',*,*,#7540,.T.);
#9888=ORIENTED_EDGE('',*,*,#7534,.F.);
#9889=ORIENTED_EDGE('',*,*,#7532,.T.);
#9890=ORIENTED_EDGE('',*,*,#7538,.F.);
#9891=ORIENTED_EDGE('',*,*,#7541,.F.);
#9892=ORIENTED_EDGE('',*,*,#7542,.T.);
#9893=ORIENTED_EDGE('',*,*,#7543,.T.);
#9894=ORIENTED_EDGE('',*,*,#7541,.T.);
#9895=ORIENTED_EDGE('',*,*,#7537,.F.);
#9896=ORIENTED_EDGE('',*,*,#7544,.F.);
#9897=ORIENTED_EDGE('',*,*,#7545,.T.);
#9898=ORIENTED_EDGE('',*,*,#7544,.T.);
#9899=ORIENTED_EDGE('',*,*,#7536,.F.);
#9900=ORIENTED_EDGE('',*,*,#7546,.F.);
#9901=ORIENTED_EDGE('',*,*,#7547,.T.);
#9902=ORIENTED_EDGE('',*,*,#7546,.T.);
#9903=ORIENTED_EDGE('',*,*,#7535,.F.);
#9904=ORIENTED_EDGE('',*,*,#7540,.F.);
#9905=ORIENTED_EDGE('',*,*,#7533,.T.);
#9906=ORIENTED_EDGE('',*,*,#7542,.F.);
#9907=ORIENTED_EDGE('',*,*,#7543,.F.);
#9908=ORIENTED_EDGE('',*,*,#7545,.F.);
#9909=ORIENTED_EDGE('',*,*,#7547,.F.);
#9910=ORIENTED_EDGE('',*,*,#7539,.F.);
#9911=ORIENTED_EDGE('',*,*,#7527,.T.);
#9912=ORIENTED_EDGE('',*,*,#7524,.T.);
#9913=ORIENTED_EDGE('',*,*,#7521,.T.);
#9914=ORIENTED_EDGE('',*,*,#7518,.T.);
#9915=ORIENTED_EDGE('',*,*,#7508,.T.);
#9916=ORIENTED_EDGE('',*,*,#7517,.T.);
#9917=ORIENTED_EDGE('',*,*,#7514,.T.);
#9918=ORIENTED_EDGE('',*,*,#7511,.T.);
#9919=ORIENTED_EDGE('',*,*,#7500,.T.);
#9920=ORIENTED_EDGE('',*,*,#7497,.T.);
#9921=ORIENTED_EDGE('',*,*,#7494,.T.);
#9922=ORIENTED_EDGE('',*,*,#7491,.T.);
#9923=ORIENTED_EDGE('',*,*,#7548,.T.);
#9924=ORIENTED_EDGE('',*,*,#7549,.T.);
#9925=ORIENTED_EDGE('',*,*,#7550,.F.);
#9926=ORIENTED_EDGE('',*,*,#7551,.F.);
#9927=ORIENTED_EDGE('',*,*,#7552,.T.);
#9928=ORIENTED_EDGE('',*,*,#7551,.T.);
#9929=ORIENTED_EDGE('',*,*,#7553,.F.);
#9930=ORIENTED_EDGE('',*,*,#7554,.F.);
#9931=ORIENTED_EDGE('',*,*,#7555,.T.);
#9932=ORIENTED_EDGE('',*,*,#7554,.T.);
#9933=ORIENTED_EDGE('',*,*,#7556,.F.);
#9934=ORIENTED_EDGE('',*,*,#7557,.F.);
#9935=ORIENTED_EDGE('',*,*,#7558,.T.);
#9936=ORIENTED_EDGE('',*,*,#7557,.T.);
#9937=ORIENTED_EDGE('',*,*,#7559,.F.);
#9938=ORIENTED_EDGE('',*,*,#7549,.F.);
#9939=ORIENTED_EDGE('',*,*,#7559,.T.);
#9940=ORIENTED_EDGE('',*,*,#7556,.T.);
#9941=ORIENTED_EDGE('',*,*,#7553,.T.);
#9942=ORIENTED_EDGE('',*,*,#7550,.T.);
#9943=ORIENTED_EDGE('',*,*,#7558,.F.);
#9944=ORIENTED_EDGE('',*,*,#7548,.F.);
#9945=ORIENTED_EDGE('',*,*,#7552,.F.);
#9946=ORIENTED_EDGE('',*,*,#7555,.F.);
#9947=ORIENTED_EDGE('',*,*,#7560,.F.);
#9948=ORIENTED_EDGE('',*,*,#7561,.F.);
#9949=ORIENTED_EDGE('',*,*,#7562,.T.);
#9950=ORIENTED_EDGE('',*,*,#7563,.F.);
#9951=ORIENTED_EDGE('',*,*,#7564,.F.);
#9952=ORIENTED_EDGE('',*,*,#7562,.F.);
#9953=ORIENTED_EDGE('',*,*,#7565,.F.);
#9954=ORIENTED_EDGE('',*,*,#7566,.T.);
#9955=ORIENTED_EDGE('',*,*,#7567,.F.);
#9956=ORIENTED_EDGE('',*,*,#7566,.F.);
#9957=ORIENTED_EDGE('',*,*,#7565,.T.);
#9958=ORIENTED_EDGE('',*,*,#7568,.F.);
#9959=ORIENTED_EDGE('',*,*,#7569,.T.);
#9960=ORIENTED_EDGE('',*,*,#7570,.F.);
#9961=ORIENTED_EDGE('',*,*,#7569,.F.);
#9962=ORIENTED_EDGE('',*,*,#7568,.T.);
#9963=ORIENTED_EDGE('',*,*,#7571,.F.);
#9964=ORIENTED_EDGE('',*,*,#7572,.T.);
#9965=ORIENTED_EDGE('',*,*,#7573,.F.);
#9966=ORIENTED_EDGE('',*,*,#7572,.F.);
#9967=ORIENTED_EDGE('',*,*,#7571,.T.);
#9968=ORIENTED_EDGE('',*,*,#7574,.F.);
#9969=ORIENTED_EDGE('',*,*,#7575,.T.);
#9970=ORIENTED_EDGE('',*,*,#7576,.F.);
#9971=ORIENTED_EDGE('',*,*,#7575,.F.);
#9972=ORIENTED_EDGE('',*,*,#7574,.T.);
#9973=ORIENTED_EDGE('',*,*,#7577,.F.);
#9974=ORIENTED_EDGE('',*,*,#7578,.T.);
#9975=ORIENTED_EDGE('',*,*,#7579,.F.);
#9976=ORIENTED_EDGE('',*,*,#7580,.F.);
#9977=ORIENTED_EDGE('',*,*,#7581,.F.);
#9978=ORIENTED_EDGE('',*,*,#7578,.F.);
#9979=ORIENTED_EDGE('',*,*,#7582,.F.);
#9980=ORIENTED_EDGE('',*,*,#7583,.T.);
#9981=ORIENTED_EDGE('',*,*,#7584,.F.);
#9982=ORIENTED_EDGE('',*,*,#7585,.F.);
#9983=ORIENTED_EDGE('',*,*,#7586,.F.);
#9984=ORIENTED_EDGE('',*,*,#7583,.F.);
#9985=ORIENTED_EDGE('',*,*,#7587,.F.);
#9986=ORIENTED_EDGE('',*,*,#7588,.T.);
#9987=ORIENTED_EDGE('',*,*,#7589,.F.);
#9988=ORIENTED_EDGE('',*,*,#7590,.F.);
#9989=ORIENTED_EDGE('',*,*,#7591,.F.);
#9990=ORIENTED_EDGE('',*,*,#7588,.F.);
#9991=ORIENTED_EDGE('',*,*,#7592,.F.);
#9992=ORIENTED_EDGE('',*,*,#7593,.T.);
#9993=ORIENTED_EDGE('',*,*,#7594,.F.);
#9994=ORIENTED_EDGE('',*,*,#7595,.F.);
#9995=ORIENTED_EDGE('',*,*,#7596,.F.);
#9996=ORIENTED_EDGE('',*,*,#7593,.F.);
#9997=ORIENTED_EDGE('',*,*,#7597,.F.);
#9998=ORIENTED_EDGE('',*,*,#7598,.T.);
#9999=ORIENTED_EDGE('',*,*,#7599,.F.);
#10000=ORIENTED_EDGE('',*,*,#7598,.F.);
#10001=ORIENTED_EDGE('',*,*,#7600,.T.);
#10002=ORIENTED_EDGE('',*,*,#7601,.F.);
#10003=ORIENTED_EDGE('',*,*,#7585,.T.);
#10004=ORIENTED_EDGE('',*,*,#7602,.F.);
#10005=ORIENTED_EDGE('',*,*,#7590,.T.);
#10006=ORIENTED_EDGE('',*,*,#7603,.F.);
#10007=ORIENTED_EDGE('',*,*,#7595,.T.);
#10008=ORIENTED_EDGE('',*,*,#7604,.F.);
#10009=ORIENTED_EDGE('',*,*,#7580,.T.);
#10010=ORIENTED_EDGE('',*,*,#7605,.F.);
#10011=ORIENTED_EDGE('',*,*,#7606,.T.);
#10012=ORIENTED_EDGE('',*,*,#7599,.T.);
#10013=ORIENTED_EDGE('',*,*,#7607,.T.);
#10014=ORIENTED_EDGE('',*,*,#7608,.T.);
#10015=ORIENTED_EDGE('',*,*,#7609,.F.);
#10016=ORIENTED_EDGE('',*,*,#7610,.T.);
#10017=ORIENTED_EDGE('',*,*,#7607,.F.);
#10018=ORIENTED_EDGE('',*,*,#7610,.F.);
#10019=ORIENTED_EDGE('',*,*,#7611,.F.);
#10020=ORIENTED_EDGE('',*,*,#7612,.T.);
#10021=ORIENTED_EDGE('',*,*,#7606,.F.);
#10022=ORIENTED_EDGE('',*,*,#7612,.F.);
#10023=ORIENTED_EDGE('',*,*,#7613,.F.);
#10024=ORIENTED_EDGE('',*,*,#7614,.T.);
#10025=ORIENTED_EDGE('',*,*,#7608,.F.);
#10026=ORIENTED_EDGE('',*,*,#7614,.F.);
#10027=ORIENTED_EDGE('',*,*,#7615,.F.);
#10028=ORIENTED_EDGE('',*,*,#7616,.T.);
#10029=ORIENTED_EDGE('',*,*,#7605,.T.);
#10030=ORIENTED_EDGE('',*,*,#7579,.T.);
#10031=ORIENTED_EDGE('',*,*,#7581,.T.);
#10032=ORIENTED_EDGE('',*,*,#7577,.T.);
#10033=ORIENTED_EDGE('',*,*,#7604,.T.);
#10034=ORIENTED_EDGE('',*,*,#7594,.T.);
#10035=ORIENTED_EDGE('',*,*,#7596,.T.);
#10036=ORIENTED_EDGE('',*,*,#7592,.T.);
#10037=ORIENTED_EDGE('',*,*,#7603,.T.);
#10038=ORIENTED_EDGE('',*,*,#7589,.T.);
#10039=ORIENTED_EDGE('',*,*,#7591,.T.);
#10040=ORIENTED_EDGE('',*,*,#7587,.T.);
#10041=ORIENTED_EDGE('',*,*,#7602,.T.);
#10042=ORIENTED_EDGE('',*,*,#7584,.T.);
#10043=ORIENTED_EDGE('',*,*,#7586,.T.);
#10044=ORIENTED_EDGE('',*,*,#7582,.T.);
#10045=ORIENTED_EDGE('',*,*,#7601,.T.);
#10046=ORIENTED_EDGE('',*,*,#7616,.F.);
#10047=ORIENTED_EDGE('',*,*,#7563,.T.);
#10048=ORIENTED_EDGE('',*,*,#7564,.T.);
#10049=ORIENTED_EDGE('',*,*,#7617,.F.);
#10050=ORIENTED_EDGE('',*,*,#7618,.T.);
#10051=ORIENTED_EDGE('',*,*,#7619,.F.);
#10052=ORIENTED_EDGE('',*,*,#7618,.F.);
#10053=ORIENTED_EDGE('',*,*,#7617,.T.);
#10054=ORIENTED_EDGE('',*,*,#7620,.F.);
#10055=ORIENTED_EDGE('',*,*,#7600,.F.);
#10056=ORIENTED_EDGE('',*,*,#7621,.T.);
#10057=ORIENTED_EDGE('',*,*,#7622,.T.);
#10058=ORIENTED_EDGE('',*,*,#7621,.F.);
#10059=ORIENTED_EDGE('',*,*,#7620,.T.);
#10060=ORIENTED_EDGE('',*,*,#7623,.T.);
#10061=ORIENTED_EDGE('',*,*,#7624,.T.);
#10062=ORIENTED_EDGE('',*,*,#7623,.F.);
#10063=ORIENTED_EDGE('',*,*,#7560,.T.);
#10064=ORIENTED_EDGE('',*,*,#7561,.T.);
#10065=ORIENTED_EDGE('',*,*,#7615,.T.);
#10066=ORIENTED_EDGE('',*,*,#7619,.T.);
#10067=ORIENTED_EDGE('',*,*,#7576,.T.);
#10068=ORIENTED_EDGE('',*,*,#7573,.T.);
#10069=ORIENTED_EDGE('',*,*,#7570,.T.);
#10070=ORIENTED_EDGE('',*,*,#7567,.T.);
#10071=ORIENTED_EDGE('',*,*,#7622,.F.);
#10072=ORIENTED_EDGE('',*,*,#7624,.F.);
#10073=ORIENTED_EDGE('',*,*,#7609,.T.);
#10074=ORIENTED_EDGE('',*,*,#7597,.T.);
#10075=ORIENTED_EDGE('',*,*,#7613,.T.);
#10076=ORIENTED_EDGE('',*,*,#7611,.T.);
#10077=ORIENTED_EDGE('',*,*,#7625,.F.);
#10078=ORIENTED_EDGE('',*,*,#7626,.T.);
#10079=ORIENTED_EDGE('',*,*,#7627,.T.);
#10080=ORIENTED_EDGE('',*,*,#7626,.F.);
#10081=ORIENTED_EDGE('',*,*,#7628,.F.);
#10082=ORIENTED_EDGE('',*,*,#7629,.T.);
#10083=ORIENTED_EDGE('',*,*,#7630,.T.);
#10084=ORIENTED_EDGE('',*,*,#7629,.F.);
#10085=ORIENTED_EDGE('',*,*,#7628,.T.);
#10086=ORIENTED_EDGE('',*,*,#7625,.T.);
#10087=ORIENTED_EDGE('',*,*,#7630,.F.);
#10088=ORIENTED_EDGE('',*,*,#7627,.F.);
#10089=ORIENTED_EDGE('',*,*,#7631,.F.);
#10090=ORIENTED_EDGE('',*,*,#7632,.T.);
#10091=ORIENTED_EDGE('',*,*,#7633,.F.);
#10092=ORIENTED_EDGE('',*,*,#7632,.F.);
#10093=ORIENTED_EDGE('',*,*,#7634,.F.);
#10094=ORIENTED_EDGE('',*,*,#7635,.T.);
#10095=ORIENTED_EDGE('',*,*,#7636,.F.);
#10096=ORIENTED_EDGE('',*,*,#7635,.F.);
#10097=ORIENTED_EDGE('',*,*,#7637,.F.);
#10098=ORIENTED_EDGE('',*,*,#7638,.T.);
#10099=ORIENTED_EDGE('',*,*,#7639,.F.);
#10100=ORIENTED_EDGE('',*,*,#7638,.F.);
#10101=ORIENTED_EDGE('',*,*,#7640,.F.);
#10102=ORIENTED_EDGE('',*,*,#7641,.T.);
#10103=ORIENTED_EDGE('',*,*,#7642,.F.);
#10104=ORIENTED_EDGE('',*,*,#7641,.F.);
#10105=ORIENTED_EDGE('',*,*,#7643,.F.);
#10106=ORIENTED_EDGE('',*,*,#7644,.T.);
#10107=ORIENTED_EDGE('',*,*,#7645,.T.);
#10108=ORIENTED_EDGE('',*,*,#7644,.F.);
#10109=ORIENTED_EDGE('',*,*,#7646,.F.);
#10110=ORIENTED_EDGE('',*,*,#7647,.T.);
#10111=ORIENTED_EDGE('',*,*,#7648,.T.);
#10112=ORIENTED_EDGE('',*,*,#7647,.F.);
#10113=ORIENTED_EDGE('',*,*,#7646,.T.);
#10114=ORIENTED_EDGE('',*,*,#7643,.T.);
#10115=ORIENTED_EDGE('',*,*,#7642,.T.);
#10116=ORIENTED_EDGE('',*,*,#7639,.T.);
#10117=ORIENTED_EDGE('',*,*,#7636,.T.);
#10118=ORIENTED_EDGE('',*,*,#7633,.T.);
#10119=ORIENTED_EDGE('',*,*,#7648,.F.);
#10120=ORIENTED_EDGE('',*,*,#7645,.F.);
#10121=ORIENTED_EDGE('',*,*,#7640,.T.);
#10122=ORIENTED_EDGE('',*,*,#7637,.T.);
#10123=ORIENTED_EDGE('',*,*,#7634,.T.);
#10124=ORIENTED_EDGE('',*,*,#7631,.T.);
#10125=ORIENTED_EDGE('',*,*,#7649,.F.);
#10126=ORIENTED_EDGE('',*,*,#7650,.T.);
#10127=ORIENTED_EDGE('',*,*,#7651,.F.);
#10128=ORIENTED_EDGE('',*,*,#7652,.F.);
#10129=ORIENTED_EDGE('',*,*,#7653,.T.);
#10130=ORIENTED_EDGE('',*,*,#7654,.F.);
#10131=ORIENTED_EDGE('',*,*,#7653,.F.);
#10132=ORIENTED_EDGE('',*,*,#7655,.F.);
#10133=ORIENTED_EDGE('',*,*,#7656,.F.);
#10134=ORIENTED_EDGE('',*,*,#7650,.F.);
#10135=ORIENTED_EDGE('',*,*,#7657,.F.);
#10136=ORIENTED_EDGE('',*,*,#7658,.T.);
#10137=ORIENTED_EDGE('',*,*,#7659,.F.);
#10138=ORIENTED_EDGE('',*,*,#7660,.F.);
#10139=ORIENTED_EDGE('',*,*,#7661,.T.);
#10140=ORIENTED_EDGE('',*,*,#7662,.F.);
#10141=ORIENTED_EDGE('',*,*,#7661,.F.);
#10142=ORIENTED_EDGE('',*,*,#7663,.F.);
#10143=ORIENTED_EDGE('',*,*,#7664,.F.);
#10144=ORIENTED_EDGE('',*,*,#7658,.F.);
#10145=ORIENTED_EDGE('',*,*,#7665,.F.);
#10146=ORIENTED_EDGE('',*,*,#7666,.T.);
#10147=ORIENTED_EDGE('',*,*,#7667,.F.);
#10148=ORIENTED_EDGE('',*,*,#7668,.F.);
#10149=ORIENTED_EDGE('',*,*,#7669,.T.);
#10150=ORIENTED_EDGE('',*,*,#7670,.F.);
#10151=ORIENTED_EDGE('',*,*,#7669,.F.);
#10152=ORIENTED_EDGE('',*,*,#7671,.F.);
#10153=ORIENTED_EDGE('',*,*,#7672,.F.);
#10154=ORIENTED_EDGE('',*,*,#7666,.F.);
#10155=ORIENTED_EDGE('',*,*,#7673,.F.);
#10156=ORIENTED_EDGE('',*,*,#7674,.T.);
#10157=ORIENTED_EDGE('',*,*,#7675,.F.);
#10158=ORIENTED_EDGE('',*,*,#7676,.F.);
#10159=ORIENTED_EDGE('',*,*,#7677,.T.);
#10160=ORIENTED_EDGE('',*,*,#7678,.F.);
#10161=ORIENTED_EDGE('',*,*,#7677,.F.);
#10162=ORIENTED_EDGE('',*,*,#7679,.F.);
#10163=ORIENTED_EDGE('',*,*,#7680,.F.);
#10164=ORIENTED_EDGE('',*,*,#7674,.F.);
#10165=ORIENTED_EDGE('',*,*,#7651,.T.);
#10166=ORIENTED_EDGE('',*,*,#7649,.T.);
#10167=ORIENTED_EDGE('',*,*,#7656,.T.);
#10168=ORIENTED_EDGE('',*,*,#7681,.T.);
#10169=ORIENTED_EDGE('',*,*,#7667,.T.);
#10170=ORIENTED_EDGE('',*,*,#7665,.T.);
#10171=ORIENTED_EDGE('',*,*,#7672,.T.);
#10172=ORIENTED_EDGE('',*,*,#7682,.T.);
#10173=ORIENTED_EDGE('',*,*,#7683,.F.);
#10174=ORIENTED_EDGE('',*,*,#7684,.T.);
#10175=ORIENTED_EDGE('',*,*,#7685,.F.);
#10176=ORIENTED_EDGE('',*,*,#7686,.T.);
#10177=ORIENTED_EDGE('',*,*,#7659,.T.);
#10178=ORIENTED_EDGE('',*,*,#7657,.T.);
#10179=ORIENTED_EDGE('',*,*,#7664,.T.);
#10180=ORIENTED_EDGE('',*,*,#7687,.T.);
#10181=ORIENTED_EDGE('',*,*,#7675,.T.);
#10182=ORIENTED_EDGE('',*,*,#7673,.T.);
#10183=ORIENTED_EDGE('',*,*,#7680,.T.);
#10184=ORIENTED_EDGE('',*,*,#7688,.T.);
#10185=ORIENTED_EDGE('',*,*,#7689,.F.);
#10186=ORIENTED_EDGE('',*,*,#7690,.F.);
#10187=ORIENTED_EDGE('',*,*,#7691,.F.);
#10188=ORIENTED_EDGE('',*,*,#7692,.T.);
#10189=ORIENTED_EDGE('',*,*,#7683,.T.);
#10190=ORIENTED_EDGE('',*,*,#7693,.T.);
#10191=ORIENTED_EDGE('',*,*,#7694,.T.);
#10192=ORIENTED_EDGE('',*,*,#7695,.T.);
#10193=ORIENTED_EDGE('',*,*,#7696,.T.);
#10194=ORIENTED_EDGE('',*,*,#7697,.T.);
#10195=ORIENTED_EDGE('',*,*,#7691,.T.);
#10196=ORIENTED_EDGE('',*,*,#7698,.T.);
#10197=ORIENTED_EDGE('',*,*,#7699,.T.);
#10198=ORIENTED_EDGE('',*,*,#7700,.T.);
#10199=ORIENTED_EDGE('',*,*,#7701,.T.);
#10200=ORIENTED_EDGE('',*,*,#7702,.T.);
#10201=ORIENTED_EDGE('',*,*,#7655,.T.);
#10202=ORIENTED_EDGE('',*,*,#7652,.T.);
#10203=ORIENTED_EDGE('',*,*,#7686,.F.);
#10204=ORIENTED_EDGE('',*,*,#7703,.F.);
#10205=ORIENTED_EDGE('',*,*,#7704,.F.);
#10206=ORIENTED_EDGE('',*,*,#7693,.F.);
#10207=ORIENTED_EDGE('',*,*,#7682,.F.);
#10208=ORIENTED_EDGE('',*,*,#7671,.T.);
#10209=ORIENTED_EDGE('',*,*,#7668,.T.);
#10210=ORIENTED_EDGE('',*,*,#7681,.F.);
#10211=ORIENTED_EDGE('',*,*,#7704,.T.);
#10212=ORIENTED_EDGE('',*,*,#7705,.F.);
#10213=ORIENTED_EDGE('',*,*,#7706,.F.);
#10214=ORIENTED_EDGE('',*,*,#7694,.F.);
#10215=ORIENTED_EDGE('',*,*,#7706,.T.);
#10216=ORIENTED_EDGE('',*,*,#7707,.F.);
#10217=ORIENTED_EDGE('',*,*,#7708,.F.);
#10218=ORIENTED_EDGE('',*,*,#7695,.F.);
#10219=ORIENTED_EDGE('',*,*,#7654,.T.);
#10220=ORIENTED_EDGE('',*,*,#7662,.T.);
#10221=ORIENTED_EDGE('',*,*,#7670,.T.);
#10222=ORIENTED_EDGE('',*,*,#7678,.T.);
#10223=ORIENTED_EDGE('',*,*,#7708,.T.);
#10224=ORIENTED_EDGE('',*,*,#7709,.F.);
#10225=ORIENTED_EDGE('',*,*,#7710,.F.);
#10226=ORIENTED_EDGE('',*,*,#7696,.F.);
#10227=ORIENTED_EDGE('',*,*,#7663,.T.);
#10228=ORIENTED_EDGE('',*,*,#7660,.T.);
#10229=ORIENTED_EDGE('',*,*,#7692,.F.);
#10230=ORIENTED_EDGE('',*,*,#7697,.F.);
#10231=ORIENTED_EDGE('',*,*,#7710,.T.);
#10232=ORIENTED_EDGE('',*,*,#7711,.F.);
#10233=ORIENTED_EDGE('',*,*,#7688,.F.);
#10234=ORIENTED_EDGE('',*,*,#7679,.T.);
#10235=ORIENTED_EDGE('',*,*,#7676,.T.);
#10236=ORIENTED_EDGE('',*,*,#7687,.F.);
#10237=ORIENTED_EDGE('',*,*,#7690,.T.);
#10238=ORIENTED_EDGE('',*,*,#7712,.F.);
#10239=ORIENTED_EDGE('',*,*,#7713,.F.);
#10240=ORIENTED_EDGE('',*,*,#7698,.F.);
#10241=ORIENTED_EDGE('',*,*,#7713,.T.);
#10242=ORIENTED_EDGE('',*,*,#7714,.F.);
#10243=ORIENTED_EDGE('',*,*,#7715,.F.);
#10244=ORIENTED_EDGE('',*,*,#7699,.F.);
#10245=ORIENTED_EDGE('',*,*,#7715,.T.);
#10246=ORIENTED_EDGE('',*,*,#7716,.F.);
#10247=ORIENTED_EDGE('',*,*,#7717,.F.);
#10248=ORIENTED_EDGE('',*,*,#7700,.F.);
#10249=ORIENTED_EDGE('',*,*,#7717,.T.);
#10250=ORIENTED_EDGE('',*,*,#7718,.F.);
#10251=ORIENTED_EDGE('',*,*,#7719,.F.);
#10252=ORIENTED_EDGE('',*,*,#7701,.F.);
#10253=ORIENTED_EDGE('',*,*,#7719,.T.);
#10254=ORIENTED_EDGE('',*,*,#7720,.F.);
#10255=ORIENTED_EDGE('',*,*,#7684,.F.);
#10256=ORIENTED_EDGE('',*,*,#7702,.F.);
#10257=ORIENTED_EDGE('',*,*,#7685,.T.);
#10258=ORIENTED_EDGE('',*,*,#7720,.T.);
#10259=ORIENTED_EDGE('',*,*,#7718,.T.);
#10260=ORIENTED_EDGE('',*,*,#7716,.T.);
#10261=ORIENTED_EDGE('',*,*,#7714,.T.);
#10262=ORIENTED_EDGE('',*,*,#7712,.T.);
#10263=ORIENTED_EDGE('',*,*,#7689,.T.);
#10264=ORIENTED_EDGE('',*,*,#7711,.T.);
#10265=ORIENTED_EDGE('',*,*,#7709,.T.);
#10266=ORIENTED_EDGE('',*,*,#7707,.T.);
#10267=ORIENTED_EDGE('',*,*,#7705,.T.);
#10268=ORIENTED_EDGE('',*,*,#7703,.T.);
#10269=ORIENTED_EDGE('',*,*,#7721,.T.);
#10270=ORIENTED_EDGE('',*,*,#7722,.T.);
#10271=ORIENTED_EDGE('',*,*,#7723,.F.);
#10272=ORIENTED_EDGE('',*,*,#7724,.F.);
#10273=ORIENTED_EDGE('',*,*,#7725,.T.);
#10274=ORIENTED_EDGE('',*,*,#7724,.T.);
#10275=ORIENTED_EDGE('',*,*,#7726,.F.);
#10276=ORIENTED_EDGE('',*,*,#7727,.F.);
#10277=ORIENTED_EDGE('',*,*,#7728,.T.);
#10278=ORIENTED_EDGE('',*,*,#7727,.T.);
#10279=ORIENTED_EDGE('',*,*,#7729,.F.);
#10280=ORIENTED_EDGE('',*,*,#7730,.F.);
#10281=ORIENTED_EDGE('',*,*,#7731,.T.);
#10282=ORIENTED_EDGE('',*,*,#7730,.T.);
#10283=ORIENTED_EDGE('',*,*,#7732,.F.);
#10284=ORIENTED_EDGE('',*,*,#7733,.F.);
#10285=ORIENTED_EDGE('',*,*,#7734,.T.);
#10286=ORIENTED_EDGE('',*,*,#7733,.T.);
#10287=ORIENTED_EDGE('',*,*,#7735,.F.);
#10288=ORIENTED_EDGE('',*,*,#7736,.F.);
#10289=ORIENTED_EDGE('',*,*,#7737,.T.);
#10290=ORIENTED_EDGE('',*,*,#7736,.T.);
#10291=ORIENTED_EDGE('',*,*,#7738,.F.);
#10292=ORIENTED_EDGE('',*,*,#7739,.F.);
#10293=ORIENTED_EDGE('',*,*,#7740,.T.);
#10294=ORIENTED_EDGE('',*,*,#7739,.T.);
#10295=ORIENTED_EDGE('',*,*,#7741,.F.);
#10296=ORIENTED_EDGE('',*,*,#7742,.F.);
#10297=ORIENTED_EDGE('',*,*,#7743,.T.);
#10298=ORIENTED_EDGE('',*,*,#7742,.T.);
#10299=ORIENTED_EDGE('',*,*,#7744,.F.);
#10300=ORIENTED_EDGE('',*,*,#7722,.F.);
#10301=ORIENTED_EDGE('',*,*,#7744,.T.);
#10302=ORIENTED_EDGE('',*,*,#7741,.T.);
#10303=ORIENTED_EDGE('',*,*,#7738,.T.);
#10304=ORIENTED_EDGE('',*,*,#7735,.T.);
#10305=ORIENTED_EDGE('',*,*,#7732,.T.);
#10306=ORIENTED_EDGE('',*,*,#7729,.T.);
#10307=ORIENTED_EDGE('',*,*,#7726,.T.);
#10308=ORIENTED_EDGE('',*,*,#7723,.T.);
#10309=ORIENTED_EDGE('',*,*,#7743,.F.);
#10310=ORIENTED_EDGE('',*,*,#7721,.F.);
#10311=ORIENTED_EDGE('',*,*,#7725,.F.);
#10312=ORIENTED_EDGE('',*,*,#7728,.F.);
#10313=ORIENTED_EDGE('',*,*,#7731,.F.);
#10314=ORIENTED_EDGE('',*,*,#7734,.F.);
#10315=ORIENTED_EDGE('',*,*,#7737,.F.);
#10316=ORIENTED_EDGE('',*,*,#7740,.F.);
#10317=ORIENTED_EDGE('',*,*,#7745,.F.);
#10318=ORIENTED_EDGE('',*,*,#7746,.T.);
#10319=ORIENTED_EDGE('',*,*,#7747,.F.);
#10320=ORIENTED_EDGE('',*,*,#7748,.F.);
#10321=ORIENTED_EDGE('',*,*,#7749,.F.);
#10322=ORIENTED_EDGE('',*,*,#7748,.T.);
#10323=ORIENTED_EDGE('',*,*,#7750,.F.);
#10324=ORIENTED_EDGE('',*,*,#7751,.F.);
#10325=ORIENTED_EDGE('',*,*,#7752,.F.);
#10326=ORIENTED_EDGE('',*,*,#7751,.T.);
#10327=ORIENTED_EDGE('',*,*,#7753,.F.);
#10328=ORIENTED_EDGE('',*,*,#7754,.F.);
#10329=ORIENTED_EDGE('',*,*,#7755,.F.);
#10330=ORIENTED_EDGE('',*,*,#7754,.T.);
#10331=ORIENTED_EDGE('',*,*,#7756,.F.);
#10332=ORIENTED_EDGE('',*,*,#7757,.F.);
#10333=ORIENTED_EDGE('',*,*,#7758,.F.);
#10334=ORIENTED_EDGE('',*,*,#7757,.T.);
#10335=ORIENTED_EDGE('',*,*,#7759,.F.);
#10336=ORIENTED_EDGE('',*,*,#7760,.F.);
#10337=ORIENTED_EDGE('',*,*,#7761,.F.);
#10338=ORIENTED_EDGE('',*,*,#7760,.T.);
#10339=ORIENTED_EDGE('',*,*,#7762,.F.);
#10340=ORIENTED_EDGE('',*,*,#7763,.F.);
#10341=ORIENTED_EDGE('',*,*,#7764,.F.);
#10342=ORIENTED_EDGE('',*,*,#7763,.T.);
#10343=ORIENTED_EDGE('',*,*,#7765,.F.);
#10344=ORIENTED_EDGE('',*,*,#7766,.F.);
#10345=ORIENTED_EDGE('',*,*,#7767,.F.);
#10346=ORIENTED_EDGE('',*,*,#7766,.T.);
#10347=ORIENTED_EDGE('',*,*,#7768,.F.);
#10348=ORIENTED_EDGE('',*,*,#7746,.F.);
#10349=ORIENTED_EDGE('',*,*,#7767,.T.);
#10350=ORIENTED_EDGE('',*,*,#7745,.T.);
#10351=ORIENTED_EDGE('',*,*,#7749,.T.);
#10352=ORIENTED_EDGE('',*,*,#7752,.T.);
#10353=ORIENTED_EDGE('',*,*,#7755,.T.);
#10354=ORIENTED_EDGE('',*,*,#7758,.T.);
#10355=ORIENTED_EDGE('',*,*,#7761,.T.);
#10356=ORIENTED_EDGE('',*,*,#7764,.T.);
#10357=ORIENTED_EDGE('',*,*,#7768,.T.);
#10358=ORIENTED_EDGE('',*,*,#7765,.T.);
#10359=ORIENTED_EDGE('',*,*,#7762,.T.);
#10360=ORIENTED_EDGE('',*,*,#7759,.T.);
#10361=ORIENTED_EDGE('',*,*,#7756,.T.);
#10362=ORIENTED_EDGE('',*,*,#7753,.T.);
#10363=ORIENTED_EDGE('',*,*,#7750,.T.);
#10364=ORIENTED_EDGE('',*,*,#7747,.T.);
#10365=ORIENTED_EDGE('',*,*,#7769,.F.);
#10366=ORIENTED_EDGE('',*,*,#7770,.T.);
#10367=ORIENTED_EDGE('',*,*,#7771,.T.);
#10368=ORIENTED_EDGE('',*,*,#7772,.F.);
#10369=ORIENTED_EDGE('',*,*,#7773,.F.);
#10370=ORIENTED_EDGE('',*,*,#7774,.T.);
#10371=ORIENTED_EDGE('',*,*,#7775,.T.);
#10372=ORIENTED_EDGE('',*,*,#7770,.F.);
#10373=ORIENTED_EDGE('',*,*,#7776,.F.);
#10374=ORIENTED_EDGE('',*,*,#7777,.T.);
#10375=ORIENTED_EDGE('',*,*,#7778,.T.);
#10376=ORIENTED_EDGE('',*,*,#7774,.F.);
#10377=ORIENTED_EDGE('',*,*,#7779,.F.);
#10378=ORIENTED_EDGE('',*,*,#7780,.T.);
#10379=ORIENTED_EDGE('',*,*,#7781,.T.);
#10380=ORIENTED_EDGE('',*,*,#7777,.F.);
#10381=ORIENTED_EDGE('',*,*,#7782,.F.);
#10382=ORIENTED_EDGE('',*,*,#7783,.T.);
#10383=ORIENTED_EDGE('',*,*,#7784,.T.);
#10384=ORIENTED_EDGE('',*,*,#7780,.F.);
#10385=ORIENTED_EDGE('',*,*,#7785,.F.);
#10386=ORIENTED_EDGE('',*,*,#7772,.T.);
#10387=ORIENTED_EDGE('',*,*,#7786,.T.);
#10388=ORIENTED_EDGE('',*,*,#7783,.F.);
#10389=ORIENTED_EDGE('',*,*,#7786,.F.);
#10390=ORIENTED_EDGE('',*,*,#7771,.F.);
#10391=ORIENTED_EDGE('',*,*,#7775,.F.);
#10392=ORIENTED_EDGE('',*,*,#7778,.F.);
#10393=ORIENTED_EDGE('',*,*,#7781,.F.);
#10394=ORIENTED_EDGE('',*,*,#7784,.F.);
#10395=ORIENTED_EDGE('',*,*,#7787,.F.);
#10396=ORIENTED_EDGE('',*,*,#7769,.T.);
#10397=ORIENTED_EDGE('',*,*,#7785,.T.);
#10398=ORIENTED_EDGE('',*,*,#7782,.T.);
#10399=ORIENTED_EDGE('',*,*,#7779,.T.);
#10400=ORIENTED_EDGE('',*,*,#7776,.T.);
#10401=ORIENTED_EDGE('',*,*,#7773,.T.);
#10402=ORIENTED_EDGE('',*,*,#7788,.F.);
#10403=ORIENTED_EDGE('',*,*,#7789,.T.);
#10404=ORIENTED_EDGE('',*,*,#7787,.T.);
#10405=ORIENTED_EDGE('',*,*,#7789,.F.);
#10406=ORIENTED_EDGE('',*,*,#7790,.F.);
#10407=ORIENTED_EDGE('',*,*,#7791,.T.);
#10408=ORIENTED_EDGE('',*,*,#7788,.T.);
#10409=ORIENTED_EDGE('',*,*,#7791,.F.);
#10410=ORIENTED_EDGE('',*,*,#7792,.F.);
#10411=ORIENTED_EDGE('',*,*,#7793,.T.);
#10412=ORIENTED_EDGE('',*,*,#7790,.T.);
#10413=ORIENTED_EDGE('',*,*,#7793,.F.);
#10414=ORIENTED_EDGE('',*,*,#7792,.T.);
#10415=ORIENTED_EDGE('',*,*,#7794,.T.);
#10416=ORIENTED_EDGE('',*,*,#7795,.T.);
#10417=ORIENTED_EDGE('',*,*,#7796,.T.);
#10418=ORIENTED_EDGE('',*,*,#7797,.F.);
#10419=ORIENTED_EDGE('',*,*,#7798,.T.);
#10420=ORIENTED_EDGE('',*,*,#7799,.T.);
#10421=ORIENTED_EDGE('',*,*,#7800,.T.);
#10422=ORIENTED_EDGE('',*,*,#7795,.F.);
#10423=ORIENTED_EDGE('',*,*,#7801,.T.);
#10424=ORIENTED_EDGE('',*,*,#7802,.T.);
#10425=ORIENTED_EDGE('',*,*,#7803,.T.);
#10426=ORIENTED_EDGE('',*,*,#7799,.F.);
#10427=ORIENTED_EDGE('',*,*,#7804,.T.);
#10428=ORIENTED_EDGE('',*,*,#7805,.T.);
#10429=ORIENTED_EDGE('',*,*,#7806,.T.);
#10430=ORIENTED_EDGE('',*,*,#7802,.F.);
#10431=ORIENTED_EDGE('',*,*,#7807,.T.);
#10432=ORIENTED_EDGE('',*,*,#7808,.T.);
#10433=ORIENTED_EDGE('',*,*,#7809,.T.);
#10434=ORIENTED_EDGE('',*,*,#7805,.F.);
#10435=ORIENTED_EDGE('',*,*,#7810,.T.);
#10436=ORIENTED_EDGE('',*,*,#7797,.T.);
#10437=ORIENTED_EDGE('',*,*,#7811,.T.);
#10438=ORIENTED_EDGE('',*,*,#7808,.F.);
#10439=ORIENTED_EDGE('',*,*,#7810,.F.);
#10440=ORIENTED_EDGE('',*,*,#7807,.F.);
#10441=ORIENTED_EDGE('',*,*,#7804,.F.);
#10442=ORIENTED_EDGE('',*,*,#7801,.F.);
#10443=ORIENTED_EDGE('',*,*,#7798,.F.);
#10444=ORIENTED_EDGE('',*,*,#7794,.F.);
#10445=ORIENTED_EDGE('',*,*,#7811,.F.);
#10446=ORIENTED_EDGE('',*,*,#7796,.F.);
#10447=ORIENTED_EDGE('',*,*,#7800,.F.);
#10448=ORIENTED_EDGE('',*,*,#7803,.F.);
#10449=ORIENTED_EDGE('',*,*,#7806,.F.);
#10450=ORIENTED_EDGE('',*,*,#7809,.F.);
#10451=ORIENTED_EDGE('',*,*,#7812,.F.);
#10452=ORIENTED_EDGE('',*,*,#7813,.F.);
#10453=ORIENTED_EDGE('',*,*,#7814,.F.);
#10454=ORIENTED_EDGE('',*,*,#7815,.T.);
#10455=ORIENTED_EDGE('',*,*,#7813,.T.);
#10456=ORIENTED_EDGE('',*,*,#7815,.F.);
#10457=ORIENTED_EDGE('',*,*,#7816,.F.);
#10458=ORIENTED_EDGE('',*,*,#7817,.T.);
#10459=ORIENTED_EDGE('',*,*,#7814,.T.);
#10460=ORIENTED_EDGE('',*,*,#7817,.F.);
#10461=ORIENTED_EDGE('',*,*,#7818,.F.);
#10462=ORIENTED_EDGE('',*,*,#7819,.T.);
#10463=ORIENTED_EDGE('',*,*,#7816,.T.);
#10464=ORIENTED_EDGE('',*,*,#7819,.F.);
#10465=ORIENTED_EDGE('',*,*,#7818,.T.);
#10466=ORIENTED_EDGE('',*,*,#7820,.F.);
#10467=ORIENTED_EDGE('',*,*,#7821,.F.);
#10468=ORIENTED_EDGE('',*,*,#7822,.T.);
#10469=ORIENTED_EDGE('',*,*,#7820,.T.);
#10470=ORIENTED_EDGE('',*,*,#7822,.F.);
#10471=ORIENTED_EDGE('',*,*,#7812,.T.);
#10472=ORIENTED_EDGE('',*,*,#7823,.T.);
#10473=ORIENTED_EDGE('',*,*,#7821,.T.);
#10474=ORIENTED_EDGE('',*,*,#7823,.F.);
#10475=ORIENTED_EDGE('',*,*,#7824,.F.);
#10476=ORIENTED_EDGE('',*,*,#7825,.F.);
#10477=ORIENTED_EDGE('',*,*,#7826,.T.);
#10478=ORIENTED_EDGE('',*,*,#7827,.F.);
#10479=ORIENTED_EDGE('',*,*,#7828,.F.);
#10480=ORIENTED_EDGE('',*,*,#7826,.F.);
#10481=ORIENTED_EDGE('',*,*,#7827,.T.);
#10482=ORIENTED_EDGE('',*,*,#7828,.T.);
#10483=ORIENTED_EDGE('',*,*,#7829,.T.);
#10484=ORIENTED_EDGE('',*,*,#7830,.T.);
#10485=ORIENTED_EDGE('',*,*,#7829,.F.);
#10486=ORIENTED_EDGE('',*,*,#7831,.T.);
#10487=ORIENTED_EDGE('',*,*,#7832,.T.);
#10488=ORIENTED_EDGE('',*,*,#7833,.F.);
#10489=ORIENTED_EDGE('',*,*,#7832,.F.);
#10490=ORIENTED_EDGE('',*,*,#7833,.T.);
#10491=ORIENTED_EDGE('',*,*,#7834,.T.);
#10492=ORIENTED_EDGE('',*,*,#7835,.F.);
#10493=ORIENTED_EDGE('',*,*,#7834,.F.);
#10494=ORIENTED_EDGE('',*,*,#7830,.F.);
#10495=ORIENTED_EDGE('',*,*,#7835,.T.);
#10496=ORIENTED_EDGE('',*,*,#7836,.F.);
#10497=ORIENTED_EDGE('',*,*,#7837,.T.);
#10498=ORIENTED_EDGE('',*,*,#7824,.T.);
#10499=ORIENTED_EDGE('',*,*,#7825,.T.);
#10500=ORIENTED_EDGE('',*,*,#7837,.F.);
#10501=ORIENTED_EDGE('',*,*,#7836,.T.);
#10502=ORIENTED_EDGE('',*,*,#7838,.F.);
#10503=ORIENTED_EDGE('',*,*,#7838,.T.);
#10504=ORIENTED_EDGE('',*,*,#7839,.T.);
#10505=ORIENTED_EDGE('',*,*,#7831,.F.);
#10506=ORIENTED_EDGE('',*,*,#7839,.F.);
#10507=ORIENTED_EDGE('',*,*,#7840,.F.);
#10508=ORIENTED_EDGE('',*,*,#7841,.F.);
#10509=ORIENTED_EDGE('',*,*,#7842,.T.);
#10510=ORIENTED_EDGE('',*,*,#7843,.F.);
#10511=ORIENTED_EDGE('',*,*,#7844,.F.);
#10512=ORIENTED_EDGE('',*,*,#7842,.F.);
#10513=ORIENTED_EDGE('',*,*,#7845,.T.);
#10514=ORIENTED_EDGE('',*,*,#7846,.T.);
#10515=ORIENTED_EDGE('',*,*,#7843,.T.);
#10516=ORIENTED_EDGE('',*,*,#7844,.T.);
#10517=ORIENTED_EDGE('',*,*,#7846,.F.);
#10518=ORIENTED_EDGE('',*,*,#7847,.F.);
#10519=ORIENTED_EDGE('',*,*,#7848,.T.);
#10520=ORIENTED_EDGE('',*,*,#7849,.F.);
#10521=ORIENTED_EDGE('',*,*,#7850,.T.);
#10522=ORIENTED_EDGE('',*,*,#7847,.T.);
#10523=ORIENTED_EDGE('',*,*,#7850,.F.);
#10524=ORIENTED_EDGE('',*,*,#7851,.F.);
#10525=ORIENTED_EDGE('',*,*,#7852,.T.);
#10526=ORIENTED_EDGE('',*,*,#7849,.T.);
#10527=ORIENTED_EDGE('',*,*,#7852,.F.);
#10528=ORIENTED_EDGE('',*,*,#7853,.F.);
#10529=ORIENTED_EDGE('',*,*,#7854,.T.);
#10530=ORIENTED_EDGE('',*,*,#7851,.T.);
#10531=ORIENTED_EDGE('',*,*,#7854,.F.);
#10532=ORIENTED_EDGE('',*,*,#7853,.T.);
#10533=ORIENTED_EDGE('',*,*,#7845,.F.);
#10534=ORIENTED_EDGE('',*,*,#7840,.T.);
#10535=ORIENTED_EDGE('',*,*,#7841,.T.);
#10536=ORIENTED_EDGE('',*,*,#7855,.T.);
#10537=ORIENTED_EDGE('',*,*,#7848,.F.);
#10538=ORIENTED_EDGE('',*,*,#7855,.F.);
#10539=ORIENTED_EDGE('',*,*,#7856,.T.);
#10540=ORIENTED_EDGE('',*,*,#7856,.F.);
#10541=ORIENTED_EDGE('',*,*,#7857,.T.);
#10542=ORIENTED_EDGE('',*,*,#7857,.F.);
#10543=ORIENTED_EDGE('',*,*,#7858,.T.);
#10544=ORIENTED_EDGE('',*,*,#7858,.F.);
#10545=ORIENTED_EDGE('',*,*,#7859,.T.);
#10546=ORIENTED_EDGE('',*,*,#7859,.F.);
#10547=ORIENTED_EDGE('',*,*,#7860,.T.);
#10548=ORIENTED_EDGE('',*,*,#7860,.F.);
#10549=ORIENTED_EDGE('',*,*,#7861,.T.);
#10550=ORIENTED_EDGE('',*,*,#7861,.F.);
#10551=ORIENTED_EDGE('',*,*,#7862,.T.);
#10552=ORIENTED_EDGE('',*,*,#7862,.F.);
#10553=ORIENTED_EDGE('',*,*,#7863,.T.);
#10554=ORIENTED_EDGE('',*,*,#7863,.F.);
#10555=ORIENTED_EDGE('',*,*,#7864,.F.);
#10556=ORIENTED_EDGE('',*,*,#7865,.F.);
#10557=ORIENTED_EDGE('',*,*,#7866,.F.);
#10558=ORIENTED_EDGE('',*,*,#7867,.F.);
#10559=ORIENTED_EDGE('',*,*,#7866,.T.);
#10560=ORIENTED_EDGE('',*,*,#7868,.F.);
#10561=ORIENTED_EDGE('',*,*,#7869,.T.);
#10562=ORIENTED_EDGE('',*,*,#7870,.F.);
#10563=ORIENTED_EDGE('',*,*,#7871,.T.);
#10564=ORIENTED_EDGE('',*,*,#7872,.F.);
#10565=ORIENTED_EDGE('',*,*,#7873,.T.);
#10566=ORIENTED_EDGE('',*,*,#7874,.T.);
#10567=ORIENTED_EDGE('',*,*,#7875,.F.);
#10568=ORIENTED_EDGE('',*,*,#7874,.F.);
#10569=ORIENTED_EDGE('',*,*,#7876,.T.);
#10570=ORIENTED_EDGE('',*,*,#7877,.F.);
#10571=ORIENTED_EDGE('',*,*,#7878,.T.);
#10572=ORIENTED_EDGE('',*,*,#7879,.F.);
#10573=ORIENTED_EDGE('',*,*,#7880,.T.);
#10574=ORIENTED_EDGE('',*,*,#7881,.F.);
#10575=ORIENTED_EDGE('',*,*,#7882,.T.);
#10576=ORIENTED_EDGE('',*,*,#7883,.F.);
#10577=ORIENTED_EDGE('',*,*,#7884,.T.);
#10578=ORIENTED_EDGE('',*,*,#7885,.F.);
#10579=ORIENTED_EDGE('',*,*,#7865,.T.);
#10580=ORIENTED_EDGE('',*,*,#7886,.T.);
#10581=ORIENTED_EDGE('',*,*,#7887,.T.);
#10582=ORIENTED_EDGE('',*,*,#7868,.T.);
#10583=ORIENTED_EDGE('',*,*,#7888,.F.);
#10584=ORIENTED_EDGE('',*,*,#7889,.F.);
#10585=ORIENTED_EDGE('',*,*,#7869,.F.);
#10586=ORIENTED_EDGE('',*,*,#7887,.F.);
#10587=ORIENTED_EDGE('',*,*,#7889,.T.);
#10588=ORIENTED_EDGE('',*,*,#7890,.T.);
#10589=ORIENTED_EDGE('',*,*,#7891,.T.);
#10590=ORIENTED_EDGE('',*,*,#7870,.T.);
#10591=ORIENTED_EDGE('',*,*,#7892,.F.);
#10592=ORIENTED_EDGE('',*,*,#7893,.F.);
#10593=ORIENTED_EDGE('',*,*,#7871,.F.);
#10594=ORIENTED_EDGE('',*,*,#7891,.F.);
#10595=ORIENTED_EDGE('',*,*,#7893,.T.);
#10596=ORIENTED_EDGE('',*,*,#7894,.T.);
#10597=ORIENTED_EDGE('',*,*,#7895,.T.);
#10598=ORIENTED_EDGE('',*,*,#7872,.T.);
#10599=ORIENTED_EDGE('',*,*,#7896,.F.);
#10600=ORIENTED_EDGE('',*,*,#7897,.F.);
#10601=ORIENTED_EDGE('',*,*,#7876,.F.);
#10602=ORIENTED_EDGE('',*,*,#7873,.F.);
#10603=ORIENTED_EDGE('',*,*,#7895,.F.);
#10604=ORIENTED_EDGE('',*,*,#7898,.F.);
#10605=ORIENTED_EDGE('',*,*,#7897,.T.);
#10606=ORIENTED_EDGE('',*,*,#7899,.T.);
#10607=ORIENTED_EDGE('',*,*,#7900,.T.);
#10608=ORIENTED_EDGE('',*,*,#7877,.T.);
#10609=ORIENTED_EDGE('',*,*,#7901,.F.);
#10610=ORIENTED_EDGE('',*,*,#7902,.F.);
#10611=ORIENTED_EDGE('',*,*,#7878,.F.);
#10612=ORIENTED_EDGE('',*,*,#7900,.F.);
#10613=ORIENTED_EDGE('',*,*,#7902,.T.);
#10614=ORIENTED_EDGE('',*,*,#7903,.T.);
#10615=ORIENTED_EDGE('',*,*,#7904,.T.);
#10616=ORIENTED_EDGE('',*,*,#7879,.T.);
#10617=ORIENTED_EDGE('',*,*,#7905,.F.);
#10618=ORIENTED_EDGE('',*,*,#7906,.F.);
#10619=ORIENTED_EDGE('',*,*,#7880,.F.);
#10620=ORIENTED_EDGE('',*,*,#7904,.F.);
#10621=ORIENTED_EDGE('',*,*,#7906,.T.);
#10622=ORIENTED_EDGE('',*,*,#7907,.T.);
#10623=ORIENTED_EDGE('',*,*,#7908,.T.);
#10624=ORIENTED_EDGE('',*,*,#7881,.T.);
#10625=ORIENTED_EDGE('',*,*,#7882,.F.);
#10626=ORIENTED_EDGE('',*,*,#7908,.F.);
#10627=ORIENTED_EDGE('',*,*,#7909,.F.);
#10628=ORIENTED_EDGE('',*,*,#7910,.F.);
#10629=ORIENTED_EDGE('',*,*,#7911,.F.);
#10630=ORIENTED_EDGE('',*,*,#7912,.T.);
#10631=ORIENTED_EDGE('',*,*,#7898,.T.);
#10632=ORIENTED_EDGE('',*,*,#7894,.F.);
#10633=ORIENTED_EDGE('',*,*,#7892,.T.);
#10634=ORIENTED_EDGE('',*,*,#7890,.F.);
#10635=ORIENTED_EDGE('',*,*,#7888,.T.);
#10636=ORIENTED_EDGE('',*,*,#7886,.F.);
#10637=ORIENTED_EDGE('',*,*,#7864,.T.);
#10638=ORIENTED_EDGE('',*,*,#7913,.F.);
#10639=ORIENTED_EDGE('',*,*,#7914,.T.);
#10640=ORIENTED_EDGE('',*,*,#7915,.F.);
#10641=ORIENTED_EDGE('',*,*,#7909,.T.);
#10642=ORIENTED_EDGE('',*,*,#7907,.F.);
#10643=ORIENTED_EDGE('',*,*,#7905,.T.);
#10644=ORIENTED_EDGE('',*,*,#7903,.F.);
#10645=ORIENTED_EDGE('',*,*,#7901,.T.);
#10646=ORIENTED_EDGE('',*,*,#7899,.F.);
#10647=ORIENTED_EDGE('',*,*,#7896,.T.);
#10648=ORIENTED_EDGE('',*,*,#7912,.F.);
#10649=ORIENTED_EDGE('',*,*,#7867,.T.);
#10650=ORIENTED_EDGE('',*,*,#7885,.T.);
#10651=ORIENTED_EDGE('',*,*,#7916,.T.);
#10652=ORIENTED_EDGE('',*,*,#7913,.T.);
#10653=ORIENTED_EDGE('',*,*,#7884,.F.);
#10654=ORIENTED_EDGE('',*,*,#7917,.F.);
#10655=ORIENTED_EDGE('',*,*,#7914,.F.);
#10656=ORIENTED_EDGE('',*,*,#7916,.F.);
#10657=ORIENTED_EDGE('',*,*,#7875,.T.);
#10658=ORIENTED_EDGE('',*,*,#7911,.T.);
#10659=ORIENTED_EDGE('',*,*,#7910,.T.);
#10660=ORIENTED_EDGE('',*,*,#7915,.T.);
#10661=ORIENTED_EDGE('',*,*,#7917,.T.);
#10662=ORIENTED_EDGE('',*,*,#7883,.T.);
#10663=ORIENTED_EDGE('',*,*,#7918,.F.);
#10664=ORIENTED_EDGE('',*,*,#7919,.T.);
#10665=ORIENTED_EDGE('',*,*,#7920,.F.);
#10666=ORIENTED_EDGE('',*,*,#7921,.T.);
#10667=ORIENTED_EDGE('',*,*,#7918,.T.);
#10668=ORIENTED_EDGE('',*,*,#7921,.F.);
#10669=ORIENTED_EDGE('',*,*,#7920,.T.);
#10670=ORIENTED_EDGE('',*,*,#7922,.F.);
#10671=ORIENTED_EDGE('',*,*,#7922,.T.);
#10672=ORIENTED_EDGE('',*,*,#7923,.T.);
#10673=ORIENTED_EDGE('',*,*,#7919,.F.);
#10674=ORIENTED_EDGE('',*,*,#7923,.F.);
#10675=ORIENTED_EDGE('',*,*,#7924,.F.);
#10676=ORIENTED_EDGE('',*,*,#7925,.T.);
#10677=ORIENTED_EDGE('',*,*,#7926,.F.);
#10678=ORIENTED_EDGE('',*,*,#7927,.T.);
#10679=ORIENTED_EDGE('',*,*,#7924,.T.);
#10680=ORIENTED_EDGE('',*,*,#7927,.F.);
#10681=ORIENTED_EDGE('',*,*,#7926,.T.);
#10682=ORIENTED_EDGE('',*,*,#7928,.F.);
#10683=ORIENTED_EDGE('',*,*,#7928,.T.);
#10684=ORIENTED_EDGE('',*,*,#7929,.T.);
#10685=ORIENTED_EDGE('',*,*,#7925,.F.);
#10686=ORIENTED_EDGE('',*,*,#7929,.F.);
#10687=ORIENTED_EDGE('',*,*,#7930,.F.);
#10688=ORIENTED_EDGE('',*,*,#7931,.T.);
#10689=ORIENTED_EDGE('',*,*,#7932,.F.);
#10690=ORIENTED_EDGE('',*,*,#7931,.F.);
#10691=ORIENTED_EDGE('',*,*,#7930,.T.);
#10692=ORIENTED_EDGE('',*,*,#7933,.F.);
#10693=ORIENTED_EDGE('',*,*,#7934,.T.);
#10694=ORIENTED_EDGE('',*,*,#7935,.F.);
#10695=ORIENTED_EDGE('',*,*,#7936,.T.);
#10696=ORIENTED_EDGE('',*,*,#7937,.F.);
#10697=ORIENTED_EDGE('',*,*,#7936,.F.);
#10698=ORIENTED_EDGE('',*,*,#7938,.F.);
#10699=ORIENTED_EDGE('',*,*,#7939,.F.);
#10700=ORIENTED_EDGE('',*,*,#7938,.T.);
#10701=ORIENTED_EDGE('',*,*,#7935,.T.);
#10702=ORIENTED_EDGE('',*,*,#7940,.T.);
#10703=ORIENTED_EDGE('',*,*,#7941,.F.);
#10704=ORIENTED_EDGE('',*,*,#7942,.F.);
#10705=ORIENTED_EDGE('',*,*,#7939,.T.);
#10706=ORIENTED_EDGE('',*,*,#7941,.T.);
#10707=ORIENTED_EDGE('',*,*,#7943,.T.);
#10708=ORIENTED_EDGE('',*,*,#7944,.F.);
#10709=ORIENTED_EDGE('',*,*,#7943,.F.);
#10710=ORIENTED_EDGE('',*,*,#7940,.F.);
#10711=ORIENTED_EDGE('',*,*,#7934,.F.);
#10712=ORIENTED_EDGE('',*,*,#7945,.T.);
#10713=ORIENTED_EDGE('',*,*,#7946,.F.);
#10714=ORIENTED_EDGE('',*,*,#7947,.F.);
#10715=ORIENTED_EDGE('',*,*,#7948,.F.);
#10716=ORIENTED_EDGE('',*,*,#7945,.F.);
#10717=ORIENTED_EDGE('',*,*,#7949,.T.);
#10718=ORIENTED_EDGE('',*,*,#7947,.T.);
#10719=ORIENTED_EDGE('',*,*,#7949,.F.);
#10720=ORIENTED_EDGE('',*,*,#7948,.T.);
#10721=ORIENTED_EDGE('',*,*,#7950,.T.);
#10722=ORIENTED_EDGE('',*,*,#7951,.T.);
#10723=ORIENTED_EDGE('',*,*,#7950,.F.);
#10724=ORIENTED_EDGE('',*,*,#7952,.F.);
#10725=ORIENTED_EDGE('',*,*,#7953,.T.);
#10726=ORIENTED_EDGE('',*,*,#7946,.T.);
#10727=ORIENTED_EDGE('',*,*,#7953,.F.);
#10728=ORIENTED_EDGE('',*,*,#7942,.T.);
#10729=ORIENTED_EDGE('',*,*,#7944,.T.);
#10730=ORIENTED_EDGE('',*,*,#7933,.T.);
#10731=ORIENTED_EDGE('',*,*,#7937,.T.);
#10732=ORIENTED_EDGE('',*,*,#7952,.T.);
#10733=ORIENTED_EDGE('',*,*,#7932,.T.);
#10734=ORIENTED_EDGE('',*,*,#7951,.F.);
#10735=ORIENTED_EDGE('',*,*,#7954,.F.);
#10736=ORIENTED_EDGE('',*,*,#7955,.T.);
#10737=ORIENTED_EDGE('',*,*,#7956,.T.);
#10738=ORIENTED_EDGE('',*,*,#7955,.F.);
#10739=ORIENTED_EDGE('',*,*,#7957,.F.);
#10740=ORIENTED_EDGE('',*,*,#7958,.T.);
#10741=ORIENTED_EDGE('',*,*,#7959,.T.);
#10742=ORIENTED_EDGE('',*,*,#7958,.F.);
#10743=ORIENTED_EDGE('',*,*,#7957,.T.);
#10744=ORIENTED_EDGE('',*,*,#7954,.T.);
#10745=ORIENTED_EDGE('',*,*,#7959,.F.);
#10746=ORIENTED_EDGE('',*,*,#7956,.F.);
#10747=ORIENTED_EDGE('',*,*,#7960,.F.);
#10748=ORIENTED_EDGE('',*,*,#7961,.T.);
#10749=ORIENTED_EDGE('',*,*,#7962,.T.);
#10750=ORIENTED_EDGE('',*,*,#7961,.F.);
#10751=ORIENTED_EDGE('',*,*,#7963,.F.);
#10752=ORIENTED_EDGE('',*,*,#7964,.T.);
#10753=ORIENTED_EDGE('',*,*,#7965,.T.);
#10754=ORIENTED_EDGE('',*,*,#7964,.F.);
#10755=ORIENTED_EDGE('',*,*,#7963,.T.);
#10756=ORIENTED_EDGE('',*,*,#7960,.T.);
#10757=ORIENTED_EDGE('',*,*,#7965,.F.);
#10758=ORIENTED_EDGE('',*,*,#7962,.F.);
#10759=ORIENTED_EDGE('',*,*,#7966,.F.);
#10760=ORIENTED_EDGE('',*,*,#7967,.T.);
#10761=ORIENTED_EDGE('',*,*,#7968,.T.);
#10762=ORIENTED_EDGE('',*,*,#7967,.F.);
#10763=ORIENTED_EDGE('',*,*,#7969,.F.);
#10764=ORIENTED_EDGE('',*,*,#7970,.T.);
#10765=ORIENTED_EDGE('',*,*,#7971,.T.);
#10766=ORIENTED_EDGE('',*,*,#7970,.F.);
#10767=ORIENTED_EDGE('',*,*,#7969,.T.);
#10768=ORIENTED_EDGE('',*,*,#7966,.T.);
#10769=ORIENTED_EDGE('',*,*,#7971,.F.);
#10770=ORIENTED_EDGE('',*,*,#7968,.F.);
#10771=ORIENTED_EDGE('',*,*,#7972,.F.);
#10772=ORIENTED_EDGE('',*,*,#7973,.T.);
#10773=ORIENTED_EDGE('',*,*,#7974,.F.);
#10774=ORIENTED_EDGE('',*,*,#7975,.F.);
#10775=ORIENTED_EDGE('',*,*,#7976,.F.);
#10776=ORIENTED_EDGE('',*,*,#7977,.F.);
#10777=ORIENTED_EDGE('',*,*,#7978,.F.);
#10778=ORIENTED_EDGE('',*,*,#7979,.F.);
#10779=ORIENTED_EDGE('',*,*,#7980,.F.);
#10780=ORIENTED_EDGE('',*,*,#7981,.F.);
#10781=ORIENTED_EDGE('',*,*,#7982,.T.);
#10782=ORIENTED_EDGE('',*,*,#7975,.T.);
#10783=ORIENTED_EDGE('',*,*,#7983,.F.);
#10784=ORIENTED_EDGE('',*,*,#7978,.T.);
#10785=ORIENTED_EDGE('',*,*,#7984,.F.);
#10786=ORIENTED_EDGE('',*,*,#7976,.T.);
#10787=ORIENTED_EDGE('',*,*,#7982,.F.);
#10788=ORIENTED_EDGE('',*,*,#7985,.F.);
#10789=ORIENTED_EDGE('',*,*,#7973,.F.);
#10790=ORIENTED_EDGE('',*,*,#7986,.F.);
#10791=ORIENTED_EDGE('',*,*,#7980,.T.);
#10792=ORIENTED_EDGE('',*,*,#7987,.F.);
#10793=ORIENTED_EDGE('',*,*,#7988,.T.);
#10794=ORIENTED_EDGE('',*,*,#7989,.T.);
#10795=ORIENTED_EDGE('',*,*,#7988,.F.);
#10796=ORIENTED_EDGE('',*,*,#7985,.T.);
#10797=ORIENTED_EDGE('',*,*,#7981,.T.);
#10798=ORIENTED_EDGE('',*,*,#7986,.T.);
#10799=ORIENTED_EDGE('',*,*,#7979,.T.);
#10800=ORIENTED_EDGE('',*,*,#7972,.T.);
#10801=ORIENTED_EDGE('',*,*,#7990,.F.);
#10802=ORIENTED_EDGE('',*,*,#7991,.T.);
#10803=ORIENTED_EDGE('',*,*,#7992,.T.);
#10804=ORIENTED_EDGE('',*,*,#7991,.F.);
#10805=ORIENTED_EDGE('',*,*,#7983,.T.);
#10806=ORIENTED_EDGE('',*,*,#7974,.T.);
#10807=ORIENTED_EDGE('',*,*,#7984,.T.);
#10808=ORIENTED_EDGE('',*,*,#7977,.T.);
#10809=ORIENTED_EDGE('',*,*,#7990,.T.);
#10810=ORIENTED_EDGE('',*,*,#7987,.T.);
#10811=ORIENTED_EDGE('',*,*,#7992,.F.);
#10812=ORIENTED_EDGE('',*,*,#7989,.F.);
#10813=ORIENTED_EDGE('',*,*,#7993,.F.);
#10814=ORIENTED_EDGE('',*,*,#7994,.T.);
#10815=ORIENTED_EDGE('',*,*,#7995,.F.);
#10816=ORIENTED_EDGE('',*,*,#7996,.F.);
#10817=ORIENTED_EDGE('',*,*,#7997,.F.);
#10818=ORIENTED_EDGE('',*,*,#7996,.T.);
#10819=ORIENTED_EDGE('',*,*,#7998,.F.);
#10820=ORIENTED_EDGE('',*,*,#7999,.F.);
#10821=ORIENTED_EDGE('',*,*,#8000,.F.);
#10822=ORIENTED_EDGE('',*,*,#7999,.T.);
#10823=ORIENTED_EDGE('',*,*,#8001,.F.);
#10824=ORIENTED_EDGE('',*,*,#8002,.F.);
#10825=ORIENTED_EDGE('',*,*,#8003,.F.);
#10826=ORIENTED_EDGE('',*,*,#8002,.T.);
#10827=ORIENTED_EDGE('',*,*,#8004,.F.);
#10828=ORIENTED_EDGE('',*,*,#7994,.F.);
#10829=ORIENTED_EDGE('',*,*,#8004,.T.);
#10830=ORIENTED_EDGE('',*,*,#8001,.T.);
#10831=ORIENTED_EDGE('',*,*,#7998,.T.);
#10832=ORIENTED_EDGE('',*,*,#7995,.T.);
#10833=ORIENTED_EDGE('',*,*,#8003,.T.);
#10834=ORIENTED_EDGE('',*,*,#7993,.T.);
#10835=ORIENTED_EDGE('',*,*,#7997,.T.);
#10836=ORIENTED_EDGE('',*,*,#8000,.T.);
#10837=ORIENTED_EDGE('',*,*,#8005,.F.);
#10838=ORIENTED_EDGE('',*,*,#8006,.T.);
#10839=ORIENTED_EDGE('',*,*,#8007,.T.);
#10840=ORIENTED_EDGE('',*,*,#8006,.F.);
#10841=ORIENTED_EDGE('',*,*,#8008,.F.);
#10842=ORIENTED_EDGE('',*,*,#8009,.T.);
#10843=ORIENTED_EDGE('',*,*,#8010,.T.);
#10844=ORIENTED_EDGE('',*,*,#8009,.F.);
#10845=ORIENTED_EDGE('',*,*,#8008,.T.);
#10846=ORIENTED_EDGE('',*,*,#8005,.T.);
#10847=ORIENTED_EDGE('',*,*,#8010,.F.);
#10848=ORIENTED_EDGE('',*,*,#8007,.F.);
#10849=ORIENTED_EDGE('',*,*,#8011,.F.);
#10850=ORIENTED_EDGE('',*,*,#8012,.F.);
#10851=ORIENTED_EDGE('',*,*,#8013,.F.);
#10852=ORIENTED_EDGE('',*,*,#8014,.F.);
#10853=ORIENTED_EDGE('',*,*,#8015,.F.);
#10854=ORIENTED_EDGE('',*,*,#8016,.T.);
#10855=ORIENTED_EDGE('',*,*,#8017,.F.);
#10856=ORIENTED_EDGE('',*,*,#8012,.T.);
#10857=ORIENTED_EDGE('',*,*,#8018,.F.);
#10858=ORIENTED_EDGE('',*,*,#8019,.F.);
#10859=ORIENTED_EDGE('',*,*,#8020,.F.);
#10860=ORIENTED_EDGE('',*,*,#8016,.F.);
#10861=ORIENTED_EDGE('',*,*,#8021,.T.);
#10862=ORIENTED_EDGE('',*,*,#8022,.T.);
#10863=ORIENTED_EDGE('',*,*,#8023,.T.);
#10864=ORIENTED_EDGE('',*,*,#8024,.T.);
#10865=ORIENTED_EDGE('',*,*,#8025,.T.);
#10866=ORIENTED_EDGE('',*,*,#8026,.T.);
#10867=ORIENTED_EDGE('',*,*,#8027,.T.);
#10868=ORIENTED_EDGE('',*,*,#8028,.T.);
#10869=ORIENTED_EDGE('',*,*,#8029,.T.);
#10870=ORIENTED_EDGE('',*,*,#8030,.T.);
#10871=ORIENTED_EDGE('',*,*,#8031,.T.);
#10872=ORIENTED_EDGE('',*,*,#8032,.T.);
#10873=ORIENTED_EDGE('',*,*,#8033,.T.);
#10874=ORIENTED_EDGE('',*,*,#8034,.T.);
#10875=ORIENTED_EDGE('',*,*,#8035,.T.);
#10876=ORIENTED_EDGE('',*,*,#8036,.T.);
#10877=ORIENTED_EDGE('',*,*,#8037,.T.);
#10878=ORIENTED_EDGE('',*,*,#8038,.T.);
#10879=ORIENTED_EDGE('',*,*,#8039,.T.);
#10880=ORIENTED_EDGE('',*,*,#8040,.T.);
#10881=ORIENTED_EDGE('',*,*,#8041,.T.);
#10882=ORIENTED_EDGE('',*,*,#8042,.T.);
#10883=ORIENTED_EDGE('',*,*,#8043,.T.);
#10884=ORIENTED_EDGE('',*,*,#8044,.T.);
#10885=ORIENTED_EDGE('',*,*,#8045,.T.);
#10886=ORIENTED_EDGE('',*,*,#8046,.T.);
#10887=ORIENTED_EDGE('',*,*,#8047,.T.);
#10888=ORIENTED_EDGE('',*,*,#8048,.T.);
#10889=ORIENTED_EDGE('',*,*,#8049,.T.);
#10890=ORIENTED_EDGE('',*,*,#8050,.T.);
#10891=ORIENTED_EDGE('',*,*,#8051,.T.);
#10892=ORIENTED_EDGE('',*,*,#8052,.T.);
#10893=ORIENTED_EDGE('',*,*,#8053,.T.);
#10894=ORIENTED_EDGE('',*,*,#8054,.T.);
#10895=ORIENTED_EDGE('',*,*,#8055,.T.);
#10896=ORIENTED_EDGE('',*,*,#8056,.T.);
#10897=ORIENTED_EDGE('',*,*,#8057,.T.);
#10898=ORIENTED_EDGE('',*,*,#8058,.T.);
#10899=ORIENTED_EDGE('',*,*,#8059,.T.);
#10900=ORIENTED_EDGE('',*,*,#8060,.T.);
#10901=ORIENTED_EDGE('',*,*,#8061,.T.);
#10902=ORIENTED_EDGE('',*,*,#8062,.T.);
#10903=ORIENTED_EDGE('',*,*,#8063,.T.);
#10904=ORIENTED_EDGE('',*,*,#8064,.T.);
#10905=ORIENTED_EDGE('',*,*,#8065,.T.);
#10906=ORIENTED_EDGE('',*,*,#8066,.T.);
#10907=ORIENTED_EDGE('',*,*,#8067,.T.);
#10908=ORIENTED_EDGE('',*,*,#8068,.T.);
#10909=ORIENTED_EDGE('',*,*,#8069,.T.);
#10910=ORIENTED_EDGE('',*,*,#8070,.T.);
#10911=ORIENTED_EDGE('',*,*,#8071,.T.);
#10912=ORIENTED_EDGE('',*,*,#8072,.T.);
#10913=ORIENTED_EDGE('',*,*,#8073,.T.);
#10914=ORIENTED_EDGE('',*,*,#8074,.T.);
#10915=ORIENTED_EDGE('',*,*,#8075,.T.);
#10916=ORIENTED_EDGE('',*,*,#8076,.T.);
#10917=ORIENTED_EDGE('',*,*,#8077,.T.);
#10918=ORIENTED_EDGE('',*,*,#8078,.T.);
#10919=ORIENTED_EDGE('',*,*,#8079,.T.);
#10920=ORIENTED_EDGE('',*,*,#8080,.T.);
#10921=ORIENTED_EDGE('',*,*,#8081,.T.);
#10922=ORIENTED_EDGE('',*,*,#8082,.T.);
#10923=ORIENTED_EDGE('',*,*,#8083,.T.);
#10924=ORIENTED_EDGE('',*,*,#8084,.T.);
#10925=ORIENTED_EDGE('',*,*,#8085,.T.);
#10926=ORIENTED_EDGE('',*,*,#8086,.T.);
#10927=ORIENTED_EDGE('',*,*,#8087,.T.);
#10928=ORIENTED_EDGE('',*,*,#8088,.T.);
#10929=ORIENTED_EDGE('',*,*,#8089,.T.);
#10930=ORIENTED_EDGE('',*,*,#8090,.T.);
#10931=ORIENTED_EDGE('',*,*,#8091,.T.);
#10932=ORIENTED_EDGE('',*,*,#8092,.T.);
#10933=ORIENTED_EDGE('',*,*,#8093,.T.);
#10934=ORIENTED_EDGE('',*,*,#8094,.T.);
#10935=ORIENTED_EDGE('',*,*,#8095,.T.);
#10936=ORIENTED_EDGE('',*,*,#8096,.T.);
#10937=ORIENTED_EDGE('',*,*,#8097,.T.);
#10938=ORIENTED_EDGE('',*,*,#8098,.T.);
#10939=ORIENTED_EDGE('',*,*,#8099,.T.);
#10940=ORIENTED_EDGE('',*,*,#8100,.T.);
#10941=ORIENTED_EDGE('',*,*,#8013,.T.);
#10942=ORIENTED_EDGE('',*,*,#8017,.T.);
#10943=ORIENTED_EDGE('',*,*,#8020,.T.);
#10944=ORIENTED_EDGE('',*,*,#8101,.T.);
#10945=ORIENTED_EDGE('',*,*,#8014,.T.);
#10946=ORIENTED_EDGE('',*,*,#8101,.F.);
#10947=ORIENTED_EDGE('',*,*,#8019,.T.);
#10948=ORIENTED_EDGE('',*,*,#8102,.F.);
#10949=ORIENTED_EDGE('',*,*,#8103,.F.);
#10950=ORIENTED_EDGE('',*,*,#8104,.T.);
#10951=ORIENTED_EDGE('',*,*,#8105,.F.);
#10952=ORIENTED_EDGE('',*,*,#8104,.F.);
#10953=ORIENTED_EDGE('',*,*,#8103,.T.);
#10954=ORIENTED_EDGE('',*,*,#8011,.T.);
#10955=ORIENTED_EDGE('',*,*,#8102,.T.);
#10956=ORIENTED_EDGE('',*,*,#8018,.T.);
#10957=ORIENTED_EDGE('',*,*,#8015,.T.);
#10958=ORIENTED_EDGE('',*,*,#8106,.F.);
#10959=ORIENTED_EDGE('',*,*,#8107,.F.);
#10960=ORIENTED_EDGE('',*,*,#8108,.F.);
#10961=ORIENTED_EDGE('',*,*,#8098,.F.);
#10962=ORIENTED_EDGE('',*,*,#8108,.T.);
#10963=ORIENTED_EDGE('',*,*,#8109,.F.);
#10964=ORIENTED_EDGE('',*,*,#8110,.F.);
#10965=ORIENTED_EDGE('',*,*,#8099,.F.);
#10966=ORIENTED_EDGE('',*,*,#8110,.T.);
#10967=ORIENTED_EDGE('',*,*,#8111,.F.);
#10968=ORIENTED_EDGE('',*,*,#8112,.F.);
#10969=ORIENTED_EDGE('',*,*,#8100,.F.);
#10970=ORIENTED_EDGE('',*,*,#8112,.T.);
#10971=ORIENTED_EDGE('',*,*,#8113,.F.);
#10972=ORIENTED_EDGE('',*,*,#8114,.T.);
#10973=ORIENTED_EDGE('',*,*,#8021,.F.);
#10974=ORIENTED_EDGE('',*,*,#8114,.F.);
#10975=ORIENTED_EDGE('',*,*,#8115,.F.);
#10976=ORIENTED_EDGE('',*,*,#8116,.F.);
#10977=ORIENTED_EDGE('',*,*,#8022,.F.);
#10978=ORIENTED_EDGE('',*,*,#8116,.T.);
#10979=ORIENTED_EDGE('',*,*,#8117,.F.);
#10980=ORIENTED_EDGE('',*,*,#8118,.F.);
#10981=ORIENTED_EDGE('',*,*,#8023,.F.);
#10982=ORIENTED_EDGE('',*,*,#8118,.T.);
#10983=ORIENTED_EDGE('',*,*,#8119,.F.);
#10984=ORIENTED_EDGE('',*,*,#8120,.F.);
#10985=ORIENTED_EDGE('',*,*,#8024,.F.);
#10986=ORIENTED_EDGE('',*,*,#8120,.T.);
#10987=ORIENTED_EDGE('',*,*,#8121,.F.);
#10988=ORIENTED_EDGE('',*,*,#8122,.T.);
#10989=ORIENTED_EDGE('',*,*,#8025,.F.);
#10990=ORIENTED_EDGE('',*,*,#8122,.F.);
#10991=ORIENTED_EDGE('',*,*,#8123,.F.);
#10992=ORIENTED_EDGE('',*,*,#8124,.F.);
#10993=ORIENTED_EDGE('',*,*,#8026,.F.);
#10994=ORIENTED_EDGE('',*,*,#8124,.T.);
#10995=ORIENTED_EDGE('',*,*,#8125,.F.);
#10996=ORIENTED_EDGE('',*,*,#8126,.F.);
#10997=ORIENTED_EDGE('',*,*,#8027,.F.);
#10998=ORIENTED_EDGE('',*,*,#8126,.T.);
#10999=ORIENTED_EDGE('',*,*,#8127,.F.);
#11000=ORIENTED_EDGE('',*,*,#8128,.F.);
#11001=ORIENTED_EDGE('',*,*,#8028,.F.);
#11002=ORIENTED_EDGE('',*,*,#8128,.T.);
#11003=ORIENTED_EDGE('',*,*,#8129,.F.);
#11004=ORIENTED_EDGE('',*,*,#8130,.T.);
#11005=ORIENTED_EDGE('',*,*,#8029,.F.);
#11006=ORIENTED_EDGE('',*,*,#8130,.F.);
#11007=ORIENTED_EDGE('',*,*,#8131,.F.);
#11008=ORIENTED_EDGE('',*,*,#8132,.F.);
#11009=ORIENTED_EDGE('',*,*,#8030,.F.);
#11010=ORIENTED_EDGE('',*,*,#8132,.T.);
#11011=ORIENTED_EDGE('',*,*,#8133,.F.);
#11012=ORIENTED_EDGE('',*,*,#8134,.F.);
#11013=ORIENTED_EDGE('',*,*,#8031,.F.);
#11014=ORIENTED_EDGE('',*,*,#8134,.T.);
#11015=ORIENTED_EDGE('',*,*,#8135,.F.);
#11016=ORIENTED_EDGE('',*,*,#8136,.F.);
#11017=ORIENTED_EDGE('',*,*,#8032,.F.);
#11018=ORIENTED_EDGE('',*,*,#8136,.T.);
#11019=ORIENTED_EDGE('',*,*,#8137,.F.);
#11020=ORIENTED_EDGE('',*,*,#8138,.T.);
#11021=ORIENTED_EDGE('',*,*,#8033,.F.);
#11022=ORIENTED_EDGE('',*,*,#8138,.F.);
#11023=ORIENTED_EDGE('',*,*,#8139,.F.);
#11024=ORIENTED_EDGE('',*,*,#8140,.F.);
#11025=ORIENTED_EDGE('',*,*,#8034,.F.);
#11026=ORIENTED_EDGE('',*,*,#8140,.T.);
#11027=ORIENTED_EDGE('',*,*,#8141,.F.);
#11028=ORIENTED_EDGE('',*,*,#8142,.F.);
#11029=ORIENTED_EDGE('',*,*,#8035,.F.);
#11030=ORIENTED_EDGE('',*,*,#8142,.T.);
#11031=ORIENTED_EDGE('',*,*,#8143,.F.);
#11032=ORIENTED_EDGE('',*,*,#8144,.F.);
#11033=ORIENTED_EDGE('',*,*,#8036,.F.);
#11034=ORIENTED_EDGE('',*,*,#8144,.T.);
#11035=ORIENTED_EDGE('',*,*,#8145,.F.);
#11036=ORIENTED_EDGE('',*,*,#8146,.T.);
#11037=ORIENTED_EDGE('',*,*,#8037,.F.);
#11038=ORIENTED_EDGE('',*,*,#8146,.F.);
#11039=ORIENTED_EDGE('',*,*,#8147,.F.);
#11040=ORIENTED_EDGE('',*,*,#8148,.F.);
#11041=ORIENTED_EDGE('',*,*,#8038,.F.);
#11042=ORIENTED_EDGE('',*,*,#8148,.T.);
#11043=ORIENTED_EDGE('',*,*,#8149,.F.);
#11044=ORIENTED_EDGE('',*,*,#8150,.F.);
#11045=ORIENTED_EDGE('',*,*,#8039,.F.);
#11046=ORIENTED_EDGE('',*,*,#8150,.T.);
#11047=ORIENTED_EDGE('',*,*,#8151,.F.);
#11048=ORIENTED_EDGE('',*,*,#8152,.F.);
#11049=ORIENTED_EDGE('',*,*,#8040,.F.);
#11050=ORIENTED_EDGE('',*,*,#8152,.T.);
#11051=ORIENTED_EDGE('',*,*,#8153,.F.);
#11052=ORIENTED_EDGE('',*,*,#8154,.T.);
#11053=ORIENTED_EDGE('',*,*,#8041,.F.);
#11054=ORIENTED_EDGE('',*,*,#8154,.F.);
#11055=ORIENTED_EDGE('',*,*,#8155,.F.);
#11056=ORIENTED_EDGE('',*,*,#8156,.F.);
#11057=ORIENTED_EDGE('',*,*,#8042,.F.);
#11058=ORIENTED_EDGE('',*,*,#8156,.T.);
#11059=ORIENTED_EDGE('',*,*,#8157,.F.);
#11060=ORIENTED_EDGE('',*,*,#8158,.F.);
#11061=ORIENTED_EDGE('',*,*,#8043,.F.);
#11062=ORIENTED_EDGE('',*,*,#8158,.T.);
#11063=ORIENTED_EDGE('',*,*,#8159,.F.);
#11064=ORIENTED_EDGE('',*,*,#8160,.F.);
#11065=ORIENTED_EDGE('',*,*,#8044,.F.);
#11066=ORIENTED_EDGE('',*,*,#8160,.T.);
#11067=ORIENTED_EDGE('',*,*,#8161,.F.);
#11068=ORIENTED_EDGE('',*,*,#8162,.T.);
#11069=ORIENTED_EDGE('',*,*,#8045,.F.);
#11070=ORIENTED_EDGE('',*,*,#8162,.F.);
#11071=ORIENTED_EDGE('',*,*,#8163,.F.);
#11072=ORIENTED_EDGE('',*,*,#8164,.F.);
#11073=ORIENTED_EDGE('',*,*,#8046,.F.);
#11074=ORIENTED_EDGE('',*,*,#8164,.T.);
#11075=ORIENTED_EDGE('',*,*,#8165,.F.);
#11076=ORIENTED_EDGE('',*,*,#8166,.F.);
#11077=ORIENTED_EDGE('',*,*,#8047,.F.);
#11078=ORIENTED_EDGE('',*,*,#8166,.T.);
#11079=ORIENTED_EDGE('',*,*,#8167,.F.);
#11080=ORIENTED_EDGE('',*,*,#8168,.F.);
#11081=ORIENTED_EDGE('',*,*,#8048,.F.);
#11082=ORIENTED_EDGE('',*,*,#8168,.T.);
#11083=ORIENTED_EDGE('',*,*,#8169,.F.);
#11084=ORIENTED_EDGE('',*,*,#8170,.T.);
#11085=ORIENTED_EDGE('',*,*,#8049,.F.);
#11086=ORIENTED_EDGE('',*,*,#8170,.F.);
#11087=ORIENTED_EDGE('',*,*,#8171,.F.);
#11088=ORIENTED_EDGE('',*,*,#8172,.F.);
#11089=ORIENTED_EDGE('',*,*,#8050,.F.);
#11090=ORIENTED_EDGE('',*,*,#8172,.T.);
#11091=ORIENTED_EDGE('',*,*,#8173,.F.);
#11092=ORIENTED_EDGE('',*,*,#8174,.F.);
#11093=ORIENTED_EDGE('',*,*,#8051,.F.);
#11094=ORIENTED_EDGE('',*,*,#8174,.T.);
#11095=ORIENTED_EDGE('',*,*,#8175,.F.);
#11096=ORIENTED_EDGE('',*,*,#8176,.F.);
#11097=ORIENTED_EDGE('',*,*,#8052,.F.);
#11098=ORIENTED_EDGE('',*,*,#8176,.T.);
#11099=ORIENTED_EDGE('',*,*,#8177,.F.);
#11100=ORIENTED_EDGE('',*,*,#8178,.T.);
#11101=ORIENTED_EDGE('',*,*,#8053,.F.);
#11102=ORIENTED_EDGE('',*,*,#8178,.F.);
#11103=ORIENTED_EDGE('',*,*,#8179,.F.);
#11104=ORIENTED_EDGE('',*,*,#8180,.F.);
#11105=ORIENTED_EDGE('',*,*,#8054,.F.);
#11106=ORIENTED_EDGE('',*,*,#8180,.T.);
#11107=ORIENTED_EDGE('',*,*,#8181,.F.);
#11108=ORIENTED_EDGE('',*,*,#8182,.F.);
#11109=ORIENTED_EDGE('',*,*,#8055,.F.);
#11110=ORIENTED_EDGE('',*,*,#8182,.T.);
#11111=ORIENTED_EDGE('',*,*,#8183,.F.);
#11112=ORIENTED_EDGE('',*,*,#8184,.F.);
#11113=ORIENTED_EDGE('',*,*,#8056,.F.);
#11114=ORIENTED_EDGE('',*,*,#8184,.T.);
#11115=ORIENTED_EDGE('',*,*,#8185,.F.);
#11116=ORIENTED_EDGE('',*,*,#8186,.T.);
#11117=ORIENTED_EDGE('',*,*,#8057,.F.);
#11118=ORIENTED_EDGE('',*,*,#8186,.F.);
#11119=ORIENTED_EDGE('',*,*,#8187,.F.);
#11120=ORIENTED_EDGE('',*,*,#8188,.F.);
#11121=ORIENTED_EDGE('',*,*,#8058,.F.);
#11122=ORIENTED_EDGE('',*,*,#8188,.T.);
#11123=ORIENTED_EDGE('',*,*,#8189,.F.);
#11124=ORIENTED_EDGE('',*,*,#8190,.F.);
#11125=ORIENTED_EDGE('',*,*,#8059,.F.);
#11126=ORIENTED_EDGE('',*,*,#8190,.T.);
#11127=ORIENTED_EDGE('',*,*,#8191,.F.);
#11128=ORIENTED_EDGE('',*,*,#8192,.F.);
#11129=ORIENTED_EDGE('',*,*,#8060,.F.);
#11130=ORIENTED_EDGE('',*,*,#8192,.T.);
#11131=ORIENTED_EDGE('',*,*,#8193,.F.);
#11132=ORIENTED_EDGE('',*,*,#8194,.T.);
#11133=ORIENTED_EDGE('',*,*,#8061,.F.);
#11134=ORIENTED_EDGE('',*,*,#8194,.F.);
#11135=ORIENTED_EDGE('',*,*,#8195,.F.);
#11136=ORIENTED_EDGE('',*,*,#8196,.F.);
#11137=ORIENTED_EDGE('',*,*,#8062,.F.);
#11138=ORIENTED_EDGE('',*,*,#8196,.T.);
#11139=ORIENTED_EDGE('',*,*,#8197,.F.);
#11140=ORIENTED_EDGE('',*,*,#8198,.F.);
#11141=ORIENTED_EDGE('',*,*,#8063,.F.);
#11142=ORIENTED_EDGE('',*,*,#8198,.T.);
#11143=ORIENTED_EDGE('',*,*,#8199,.F.);
#11144=ORIENTED_EDGE('',*,*,#8200,.F.);
#11145=ORIENTED_EDGE('',*,*,#8064,.F.);
#11146=ORIENTED_EDGE('',*,*,#8200,.T.);
#11147=ORIENTED_EDGE('',*,*,#8201,.F.);
#11148=ORIENTED_EDGE('',*,*,#8202,.T.);
#11149=ORIENTED_EDGE('',*,*,#8065,.F.);
#11150=ORIENTED_EDGE('',*,*,#8202,.F.);
#11151=ORIENTED_EDGE('',*,*,#8203,.F.);
#11152=ORIENTED_EDGE('',*,*,#8204,.F.);
#11153=ORIENTED_EDGE('',*,*,#8066,.F.);
#11154=ORIENTED_EDGE('',*,*,#8204,.T.);
#11155=ORIENTED_EDGE('',*,*,#8205,.F.);
#11156=ORIENTED_EDGE('',*,*,#8206,.F.);
#11157=ORIENTED_EDGE('',*,*,#8067,.F.);
#11158=ORIENTED_EDGE('',*,*,#8206,.T.);
#11159=ORIENTED_EDGE('',*,*,#8207,.F.);
#11160=ORIENTED_EDGE('',*,*,#8208,.F.);
#11161=ORIENTED_EDGE('',*,*,#8068,.F.);
#11162=ORIENTED_EDGE('',*,*,#8208,.T.);
#11163=ORIENTED_EDGE('',*,*,#8209,.F.);
#11164=ORIENTED_EDGE('',*,*,#8210,.T.);
#11165=ORIENTED_EDGE('',*,*,#8069,.F.);
#11166=ORIENTED_EDGE('',*,*,#8210,.F.);
#11167=ORIENTED_EDGE('',*,*,#8211,.F.);
#11168=ORIENTED_EDGE('',*,*,#8212,.F.);
#11169=ORIENTED_EDGE('',*,*,#8070,.F.);
#11170=ORIENTED_EDGE('',*,*,#8212,.T.);
#11171=ORIENTED_EDGE('',*,*,#8213,.F.);
#11172=ORIENTED_EDGE('',*,*,#8214,.F.);
#11173=ORIENTED_EDGE('',*,*,#8071,.F.);
#11174=ORIENTED_EDGE('',*,*,#8214,.T.);
#11175=ORIENTED_EDGE('',*,*,#8215,.F.);
#11176=ORIENTED_EDGE('',*,*,#8216,.F.);
#11177=ORIENTED_EDGE('',*,*,#8072,.F.);
#11178=ORIENTED_EDGE('',*,*,#8216,.T.);
#11179=ORIENTED_EDGE('',*,*,#8217,.F.);
#11180=ORIENTED_EDGE('',*,*,#8218,.T.);
#11181=ORIENTED_EDGE('',*,*,#8073,.F.);
#11182=ORIENTED_EDGE('',*,*,#8218,.F.);
#11183=ORIENTED_EDGE('',*,*,#8219,.F.);
#11184=ORIENTED_EDGE('',*,*,#8220,.F.);
#11185=ORIENTED_EDGE('',*,*,#8074,.F.);
#11186=ORIENTED_EDGE('',*,*,#8220,.T.);
#11187=ORIENTED_EDGE('',*,*,#8221,.F.);
#11188=ORIENTED_EDGE('',*,*,#8222,.F.);
#11189=ORIENTED_EDGE('',*,*,#8075,.F.);
#11190=ORIENTED_EDGE('',*,*,#8222,.T.);
#11191=ORIENTED_EDGE('',*,*,#8223,.F.);
#11192=ORIENTED_EDGE('',*,*,#8224,.F.);
#11193=ORIENTED_EDGE('',*,*,#8076,.F.);
#11194=ORIENTED_EDGE('',*,*,#8224,.T.);
#11195=ORIENTED_EDGE('',*,*,#8225,.F.);
#11196=ORIENTED_EDGE('',*,*,#8226,.T.);
#11197=ORIENTED_EDGE('',*,*,#8077,.F.);
#11198=ORIENTED_EDGE('',*,*,#8226,.F.);
#11199=ORIENTED_EDGE('',*,*,#8227,.F.);
#11200=ORIENTED_EDGE('',*,*,#8228,.F.);
#11201=ORIENTED_EDGE('',*,*,#8078,.F.);
#11202=ORIENTED_EDGE('',*,*,#8228,.T.);
#11203=ORIENTED_EDGE('',*,*,#8229,.F.);
#11204=ORIENTED_EDGE('',*,*,#8230,.F.);
#11205=ORIENTED_EDGE('',*,*,#8079,.F.);
#11206=ORIENTED_EDGE('',*,*,#8230,.T.);
#11207=ORIENTED_EDGE('',*,*,#8231,.F.);
#11208=ORIENTED_EDGE('',*,*,#8232,.F.);
#11209=ORIENTED_EDGE('',*,*,#8080,.F.);
#11210=ORIENTED_EDGE('',*,*,#8232,.T.);
#11211=ORIENTED_EDGE('',*,*,#8233,.F.);
#11212=ORIENTED_EDGE('',*,*,#8234,.T.);
#11213=ORIENTED_EDGE('',*,*,#8081,.F.);
#11214=ORIENTED_EDGE('',*,*,#8234,.F.);
#11215=ORIENTED_EDGE('',*,*,#8235,.F.);
#11216=ORIENTED_EDGE('',*,*,#8236,.F.);
#11217=ORIENTED_EDGE('',*,*,#8082,.F.);
#11218=ORIENTED_EDGE('',*,*,#8236,.T.);
#11219=ORIENTED_EDGE('',*,*,#8237,.F.);
#11220=ORIENTED_EDGE('',*,*,#8238,.F.);
#11221=ORIENTED_EDGE('',*,*,#8083,.F.);
#11222=ORIENTED_EDGE('',*,*,#8238,.T.);
#11223=ORIENTED_EDGE('',*,*,#8239,.F.);
#11224=ORIENTED_EDGE('',*,*,#8240,.F.);
#11225=ORIENTED_EDGE('',*,*,#8084,.F.);
#11226=ORIENTED_EDGE('',*,*,#8240,.T.);
#11227=ORIENTED_EDGE('',*,*,#8241,.F.);
#11228=ORIENTED_EDGE('',*,*,#8242,.T.);
#11229=ORIENTED_EDGE('',*,*,#8085,.F.);
#11230=ORIENTED_EDGE('',*,*,#8242,.F.);
#11231=ORIENTED_EDGE('',*,*,#8243,.F.);
#11232=ORIENTED_EDGE('',*,*,#8244,.F.);
#11233=ORIENTED_EDGE('',*,*,#8086,.F.);
#11234=ORIENTED_EDGE('',*,*,#8244,.T.);
#11235=ORIENTED_EDGE('',*,*,#8245,.F.);
#11236=ORIENTED_EDGE('',*,*,#8246,.F.);
#11237=ORIENTED_EDGE('',*,*,#8087,.F.);
#11238=ORIENTED_EDGE('',*,*,#8246,.T.);
#11239=ORIENTED_EDGE('',*,*,#8247,.F.);
#11240=ORIENTED_EDGE('',*,*,#8248,.F.);
#11241=ORIENTED_EDGE('',*,*,#8088,.F.);
#11242=ORIENTED_EDGE('',*,*,#8248,.T.);
#11243=ORIENTED_EDGE('',*,*,#8249,.F.);
#11244=ORIENTED_EDGE('',*,*,#8250,.T.);
#11245=ORIENTED_EDGE('',*,*,#8089,.F.);
#11246=ORIENTED_EDGE('',*,*,#8250,.F.);
#11247=ORIENTED_EDGE('',*,*,#8251,.F.);
#11248=ORIENTED_EDGE('',*,*,#8252,.F.);
#11249=ORIENTED_EDGE('',*,*,#8090,.F.);
#11250=ORIENTED_EDGE('',*,*,#8252,.T.);
#11251=ORIENTED_EDGE('',*,*,#8253,.F.);
#11252=ORIENTED_EDGE('',*,*,#8254,.F.);
#11253=ORIENTED_EDGE('',*,*,#8091,.F.);
#11254=ORIENTED_EDGE('',*,*,#8254,.T.);
#11255=ORIENTED_EDGE('',*,*,#8255,.F.);
#11256=ORIENTED_EDGE('',*,*,#8256,.F.);
#11257=ORIENTED_EDGE('',*,*,#8092,.F.);
#11258=ORIENTED_EDGE('',*,*,#8256,.T.);
#11259=ORIENTED_EDGE('',*,*,#8257,.F.);
#11260=ORIENTED_EDGE('',*,*,#8258,.T.);
#11261=ORIENTED_EDGE('',*,*,#8093,.F.);
#11262=ORIENTED_EDGE('',*,*,#8258,.F.);
#11263=ORIENTED_EDGE('',*,*,#8259,.F.);
#11264=ORIENTED_EDGE('',*,*,#8260,.F.);
#11265=ORIENTED_EDGE('',*,*,#8094,.F.);
#11266=ORIENTED_EDGE('',*,*,#8260,.T.);
#11267=ORIENTED_EDGE('',*,*,#8261,.F.);
#11268=ORIENTED_EDGE('',*,*,#8262,.F.);
#11269=ORIENTED_EDGE('',*,*,#8095,.F.);
#11270=ORIENTED_EDGE('',*,*,#8262,.T.);
#11271=ORIENTED_EDGE('',*,*,#8263,.F.);
#11272=ORIENTED_EDGE('',*,*,#8264,.F.);
#11273=ORIENTED_EDGE('',*,*,#8096,.F.);
#11274=ORIENTED_EDGE('',*,*,#8265,.T.);
#11275=ORIENTED_EDGE('',*,*,#8263,.T.);
#11276=ORIENTED_EDGE('',*,*,#8261,.T.);
#11277=ORIENTED_EDGE('',*,*,#8259,.T.);
#11278=ORIENTED_EDGE('',*,*,#8257,.T.);
#11279=ORIENTED_EDGE('',*,*,#8255,.T.);
#11280=ORIENTED_EDGE('',*,*,#8253,.T.);
#11281=ORIENTED_EDGE('',*,*,#8251,.T.);
#11282=ORIENTED_EDGE('',*,*,#8249,.T.);
#11283=ORIENTED_EDGE('',*,*,#8247,.T.);
#11284=ORIENTED_EDGE('',*,*,#8245,.T.);
#11285=ORIENTED_EDGE('',*,*,#8243,.T.);
#11286=ORIENTED_EDGE('',*,*,#8241,.T.);
#11287=ORIENTED_EDGE('',*,*,#8239,.T.);
#11288=ORIENTED_EDGE('',*,*,#8237,.T.);
#11289=ORIENTED_EDGE('',*,*,#8235,.T.);
#11290=ORIENTED_EDGE('',*,*,#8233,.T.);
#11291=ORIENTED_EDGE('',*,*,#8231,.T.);
#11292=ORIENTED_EDGE('',*,*,#8229,.T.);
#11293=ORIENTED_EDGE('',*,*,#8227,.T.);
#11294=ORIENTED_EDGE('',*,*,#8225,.T.);
#11295=ORIENTED_EDGE('',*,*,#8223,.T.);
#11296=ORIENTED_EDGE('',*,*,#8221,.T.);
#11297=ORIENTED_EDGE('',*,*,#8219,.T.);
#11298=ORIENTED_EDGE('',*,*,#8217,.T.);
#11299=ORIENTED_EDGE('',*,*,#8215,.T.);
#11300=ORIENTED_EDGE('',*,*,#8213,.T.);
#11301=ORIENTED_EDGE('',*,*,#8211,.T.);
#11302=ORIENTED_EDGE('',*,*,#8209,.T.);
#11303=ORIENTED_EDGE('',*,*,#8207,.T.);
#11304=ORIENTED_EDGE('',*,*,#8205,.T.);
#11305=ORIENTED_EDGE('',*,*,#8203,.T.);
#11306=ORIENTED_EDGE('',*,*,#8201,.T.);
#11307=ORIENTED_EDGE('',*,*,#8199,.T.);
#11308=ORIENTED_EDGE('',*,*,#8197,.T.);
#11309=ORIENTED_EDGE('',*,*,#8195,.T.);
#11310=ORIENTED_EDGE('',*,*,#8193,.T.);
#11311=ORIENTED_EDGE('',*,*,#8191,.T.);
#11312=ORIENTED_EDGE('',*,*,#8189,.T.);
#11313=ORIENTED_EDGE('',*,*,#8187,.T.);
#11314=ORIENTED_EDGE('',*,*,#8185,.T.);
#11315=ORIENTED_EDGE('',*,*,#8183,.T.);
#11316=ORIENTED_EDGE('',*,*,#8181,.T.);
#11317=ORIENTED_EDGE('',*,*,#8179,.T.);
#11318=ORIENTED_EDGE('',*,*,#8177,.T.);
#11319=ORIENTED_EDGE('',*,*,#8175,.T.);
#11320=ORIENTED_EDGE('',*,*,#8173,.T.);
#11321=ORIENTED_EDGE('',*,*,#8171,.T.);
#11322=ORIENTED_EDGE('',*,*,#8169,.T.);
#11323=ORIENTED_EDGE('',*,*,#8167,.T.);
#11324=ORIENTED_EDGE('',*,*,#8165,.T.);
#11325=ORIENTED_EDGE('',*,*,#8163,.T.);
#11326=ORIENTED_EDGE('',*,*,#8161,.T.);
#11327=ORIENTED_EDGE('',*,*,#8159,.T.);
#11328=ORIENTED_EDGE('',*,*,#8157,.T.);
#11329=ORIENTED_EDGE('',*,*,#8155,.T.);
#11330=ORIENTED_EDGE('',*,*,#8153,.T.);
#11331=ORIENTED_EDGE('',*,*,#8151,.T.);
#11332=ORIENTED_EDGE('',*,*,#8149,.T.);
#11333=ORIENTED_EDGE('',*,*,#8147,.T.);
#11334=ORIENTED_EDGE('',*,*,#8145,.T.);
#11335=ORIENTED_EDGE('',*,*,#8143,.T.);
#11336=ORIENTED_EDGE('',*,*,#8141,.T.);
#11337=ORIENTED_EDGE('',*,*,#8139,.T.);
#11338=ORIENTED_EDGE('',*,*,#8137,.T.);
#11339=ORIENTED_EDGE('',*,*,#8135,.T.);
#11340=ORIENTED_EDGE('',*,*,#8133,.T.);
#11341=ORIENTED_EDGE('',*,*,#8131,.T.);
#11342=ORIENTED_EDGE('',*,*,#8129,.T.);
#11343=ORIENTED_EDGE('',*,*,#8127,.T.);
#11344=ORIENTED_EDGE('',*,*,#8125,.T.);
#11345=ORIENTED_EDGE('',*,*,#8123,.T.);
#11346=ORIENTED_EDGE('',*,*,#8121,.T.);
#11347=ORIENTED_EDGE('',*,*,#8119,.T.);
#11348=ORIENTED_EDGE('',*,*,#8117,.T.);
#11349=ORIENTED_EDGE('',*,*,#8115,.T.);
#11350=ORIENTED_EDGE('',*,*,#8113,.T.);
#11351=ORIENTED_EDGE('',*,*,#8111,.T.);
#11352=ORIENTED_EDGE('',*,*,#8109,.T.);
#11353=ORIENTED_EDGE('',*,*,#8107,.T.);
#11354=ORIENTED_EDGE('',*,*,#8105,.T.);
#11355=ORIENTED_EDGE('',*,*,#8106,.T.);
#11356=ORIENTED_EDGE('',*,*,#8097,.F.);
#11357=ORIENTED_EDGE('',*,*,#8264,.T.);
#11358=ORIENTED_EDGE('',*,*,#8265,.F.);
#11359=ORIENTED_EDGE('',*,*,#8266,.F.);
#11360=ORIENTED_EDGE('',*,*,#8267,.T.);
#11361=ORIENTED_EDGE('',*,*,#8268,.F.);
#11362=ORIENTED_EDGE('',*,*,#8267,.F.);
#11363=ORIENTED_EDGE('',*,*,#8266,.T.);
#11364=ORIENTED_EDGE('',*,*,#8269,.F.);
#11365=ORIENTED_EDGE('',*,*,#8270,.T.);
#11366=ORIENTED_EDGE('',*,*,#8271,.F.);
#11367=ORIENTED_EDGE('',*,*,#8272,.T.);
#11368=ORIENTED_EDGE('',*,*,#8273,.F.);
#11369=ORIENTED_EDGE('',*,*,#8272,.F.);
#11370=ORIENTED_EDGE('',*,*,#8274,.F.);
#11371=ORIENTED_EDGE('',*,*,#8275,.F.);
#11372=ORIENTED_EDGE('',*,*,#8274,.T.);
#11373=ORIENTED_EDGE('',*,*,#8271,.T.);
#11374=ORIENTED_EDGE('',*,*,#8276,.T.);
#11375=ORIENTED_EDGE('',*,*,#8277,.F.);
#11376=ORIENTED_EDGE('',*,*,#8278,.F.);
#11377=ORIENTED_EDGE('',*,*,#8275,.T.);
#11378=ORIENTED_EDGE('',*,*,#8277,.T.);
#11379=ORIENTED_EDGE('',*,*,#8279,.T.);
#11380=ORIENTED_EDGE('',*,*,#8280,.F.);
#11381=ORIENTED_EDGE('',*,*,#8279,.F.);
#11382=ORIENTED_EDGE('',*,*,#8276,.F.);
#11383=ORIENTED_EDGE('',*,*,#8270,.F.);
#11384=ORIENTED_EDGE('',*,*,#8281,.T.);
#11385=ORIENTED_EDGE('',*,*,#8282,.F.);
#11386=ORIENTED_EDGE('',*,*,#8283,.F.);
#11387=ORIENTED_EDGE('',*,*,#8284,.F.);
#11388=ORIENTED_EDGE('',*,*,#8281,.F.);
#11389=ORIENTED_EDGE('',*,*,#8285,.T.);
#11390=ORIENTED_EDGE('',*,*,#8283,.T.);
#11391=ORIENTED_EDGE('',*,*,#8285,.F.);
#11392=ORIENTED_EDGE('',*,*,#8284,.T.);
#11393=ORIENTED_EDGE('',*,*,#8286,.T.);
#11394=ORIENTED_EDGE('',*,*,#8287,.T.);
#11395=ORIENTED_EDGE('',*,*,#8286,.F.);
#11396=ORIENTED_EDGE('',*,*,#8288,.F.);
#11397=ORIENTED_EDGE('',*,*,#8289,.T.);
#11398=ORIENTED_EDGE('',*,*,#8282,.T.);
#11399=ORIENTED_EDGE('',*,*,#8289,.F.);
#11400=ORIENTED_EDGE('',*,*,#8278,.T.);
#11401=ORIENTED_EDGE('',*,*,#8280,.T.);
#11402=ORIENTED_EDGE('',*,*,#8269,.T.);
#11403=ORIENTED_EDGE('',*,*,#8273,.T.);
#11404=ORIENTED_EDGE('',*,*,#8288,.T.);
#11405=ORIENTED_EDGE('',*,*,#8268,.T.);
#11406=ORIENTED_EDGE('',*,*,#8287,.F.);
#11407=ORIENTED_EDGE('',*,*,#8290,.F.);
#11408=ORIENTED_EDGE('',*,*,#8291,.T.);
#11409=ORIENTED_EDGE('',*,*,#8292,.T.);
#11410=ORIENTED_EDGE('',*,*,#8291,.F.);
#11411=ORIENTED_EDGE('',*,*,#8293,.F.);
#11412=ORIENTED_EDGE('',*,*,#8294,.T.);
#11413=ORIENTED_EDGE('',*,*,#8295,.T.);
#11414=ORIENTED_EDGE('',*,*,#8294,.F.);
#11415=ORIENTED_EDGE('',*,*,#8293,.T.);
#11416=ORIENTED_EDGE('',*,*,#8290,.T.);
#11417=ORIENTED_EDGE('',*,*,#8295,.F.);
#11418=ORIENTED_EDGE('',*,*,#8292,.F.);
#11419=ORIENTED_EDGE('',*,*,#8296,.F.);
#11420=ORIENTED_EDGE('',*,*,#8297,.T.);
#11421=ORIENTED_EDGE('',*,*,#8298,.T.);
#11422=ORIENTED_EDGE('',*,*,#8297,.F.);
#11423=ORIENTED_EDGE('',*,*,#8299,.F.);
#11424=ORIENTED_EDGE('',*,*,#8300,.T.);
#11425=ORIENTED_EDGE('',*,*,#8301,.T.);
#11426=ORIENTED_EDGE('',*,*,#8300,.F.);
#11427=ORIENTED_EDGE('',*,*,#8299,.T.);
#11428=ORIENTED_EDGE('',*,*,#8296,.T.);
#11429=ORIENTED_EDGE('',*,*,#8301,.F.);
#11430=ORIENTED_EDGE('',*,*,#8298,.F.);
#11431=ORIENTED_EDGE('',*,*,#8302,.F.);
#11432=ORIENTED_EDGE('',*,*,#8303,.F.);
#11433=ORIENTED_EDGE('',*,*,#8304,.T.);
#11434=ORIENTED_EDGE('',*,*,#8305,.F.);
#11435=ORIENTED_EDGE('',*,*,#8306,.F.);
#11436=ORIENTED_EDGE('',*,*,#8304,.F.);
#11437=ORIENTED_EDGE('',*,*,#8307,.F.);
#11438=ORIENTED_EDGE('',*,*,#8308,.T.);
#11439=ORIENTED_EDGE('',*,*,#8309,.T.);
#11440=ORIENTED_EDGE('',*,*,#8308,.F.);
#11441=ORIENTED_EDGE('',*,*,#8302,.T.);
#11442=ORIENTED_EDGE('',*,*,#8303,.T.);
#11443=ORIENTED_EDGE('',*,*,#8310,.F.);
#11444=ORIENTED_EDGE('',*,*,#8311,.T.);
#11445=ORIENTED_EDGE('',*,*,#8312,.T.);
#11446=ORIENTED_EDGE('',*,*,#8311,.F.);
#11447=ORIENTED_EDGE('',*,*,#8305,.T.);
#11448=ORIENTED_EDGE('',*,*,#8306,.T.);
#11449=ORIENTED_EDGE('',*,*,#8310,.T.);
#11450=ORIENTED_EDGE('',*,*,#8307,.T.);
#11451=ORIENTED_EDGE('',*,*,#8312,.F.);
#11452=ORIENTED_EDGE('',*,*,#8309,.F.);
#11453=ORIENTED_EDGE('',*,*,#8313,.F.);
#11454=ORIENTED_EDGE('',*,*,#8314,.T.);
#11455=ORIENTED_EDGE('',*,*,#8315,.F.);
#11456=ORIENTED_EDGE('',*,*,#8316,.F.);
#11457=ORIENTED_EDGE('',*,*,#8317,.F.);
#11458=ORIENTED_EDGE('',*,*,#8316,.T.);
#11459=ORIENTED_EDGE('',*,*,#8318,.F.);
#11460=ORIENTED_EDGE('',*,*,#8319,.F.);
#11461=ORIENTED_EDGE('',*,*,#8320,.F.);
#11462=ORIENTED_EDGE('',*,*,#8319,.T.);
#11463=ORIENTED_EDGE('',*,*,#8321,.F.);
#11464=ORIENTED_EDGE('',*,*,#8322,.F.);
#11465=ORIENTED_EDGE('',*,*,#8323,.F.);
#11466=ORIENTED_EDGE('',*,*,#8322,.T.);
#11467=ORIENTED_EDGE('',*,*,#8324,.F.);
#11468=ORIENTED_EDGE('',*,*,#8314,.F.);
#11469=ORIENTED_EDGE('',*,*,#8324,.T.);
#11470=ORIENTED_EDGE('',*,*,#8321,.T.);
#11471=ORIENTED_EDGE('',*,*,#8318,.T.);
#11472=ORIENTED_EDGE('',*,*,#8315,.T.);
#11473=ORIENTED_EDGE('',*,*,#8323,.T.);
#11474=ORIENTED_EDGE('',*,*,#8313,.T.);
#11475=ORIENTED_EDGE('',*,*,#8317,.T.);
#11476=ORIENTED_EDGE('',*,*,#8320,.T.);
#11477=ORIENTED_EDGE('',*,*,#8325,.F.);
#11478=ORIENTED_EDGE('',*,*,#8326,.T.);
#11479=ORIENTED_EDGE('',*,*,#8327,.T.);
#11480=ORIENTED_EDGE('',*,*,#8326,.F.);
#11481=ORIENTED_EDGE('',*,*,#8328,.F.);
#11482=ORIENTED_EDGE('',*,*,#8329,.T.);
#11483=ORIENTED_EDGE('',*,*,#8330,.T.);
#11484=ORIENTED_EDGE('',*,*,#8329,.F.);
#11485=ORIENTED_EDGE('',*,*,#8328,.T.);
#11486=ORIENTED_EDGE('',*,*,#8325,.T.);
#11487=ORIENTED_EDGE('',*,*,#8330,.F.);
#11488=ORIENTED_EDGE('',*,*,#8327,.F.);
#11489=ORIENTED_EDGE('',*,*,#8331,.F.);
#11490=ORIENTED_EDGE('',*,*,#8332,.F.);
#11491=ORIENTED_EDGE('',*,*,#8333,.T.);
#11492=ORIENTED_EDGE('',*,*,#8334,.T.);
#11493=ORIENTED_EDGE('',*,*,#8335,.F.);
#11494=ORIENTED_EDGE('',*,*,#8336,.F.);
#11495=ORIENTED_EDGE('',*,*,#8337,.T.);
#11496=ORIENTED_EDGE('',*,*,#8338,.T.);
#11497=ORIENTED_EDGE('',*,*,#8333,.F.);
#11498=ORIENTED_EDGE('',*,*,#8339,.F.);
#11499=ORIENTED_EDGE('',*,*,#8340,.T.);
#11500=ORIENTED_EDGE('',*,*,#8341,.T.);
#11501=ORIENTED_EDGE('',*,*,#8337,.F.);
#11502=ORIENTED_EDGE('',*,*,#8342,.F.);
#11503=ORIENTED_EDGE('',*,*,#8343,.T.);
#11504=ORIENTED_EDGE('',*,*,#8344,.T.);
#11505=ORIENTED_EDGE('',*,*,#8340,.F.);
#11506=ORIENTED_EDGE('',*,*,#8345,.F.);
#11507=ORIENTED_EDGE('',*,*,#8346,.T.);
#11508=ORIENTED_EDGE('',*,*,#8347,.T.);
#11509=ORIENTED_EDGE('',*,*,#8343,.F.);
#11510=ORIENTED_EDGE('',*,*,#8348,.F.);
#11511=ORIENTED_EDGE('',*,*,#8335,.T.);
#11512=ORIENTED_EDGE('',*,*,#8349,.T.);
#11513=ORIENTED_EDGE('',*,*,#8346,.F.);
#11514=ORIENTED_EDGE('',*,*,#8349,.F.);
#11515=ORIENTED_EDGE('',*,*,#8334,.F.);
#11516=ORIENTED_EDGE('',*,*,#8338,.F.);
#11517=ORIENTED_EDGE('',*,*,#8341,.F.);
#11518=ORIENTED_EDGE('',*,*,#8344,.F.);
#11519=ORIENTED_EDGE('',*,*,#8347,.F.);
#11520=ORIENTED_EDGE('',*,*,#8350,.F.);
#11521=ORIENTED_EDGE('',*,*,#8332,.T.);
#11522=ORIENTED_EDGE('',*,*,#8348,.T.);
#11523=ORIENTED_EDGE('',*,*,#8345,.T.);
#11524=ORIENTED_EDGE('',*,*,#8342,.T.);
#11525=ORIENTED_EDGE('',*,*,#8339,.T.);
#11526=ORIENTED_EDGE('',*,*,#8336,.T.);
#11527=ORIENTED_EDGE('',*,*,#8351,.F.);
#11528=ORIENTED_EDGE('',*,*,#8352,.T.);
#11529=ORIENTED_EDGE('',*,*,#8350,.T.);
#11530=ORIENTED_EDGE('',*,*,#8352,.F.);
#11531=ORIENTED_EDGE('',*,*,#8331,.T.);
#11532=ORIENTED_EDGE('',*,*,#8353,.T.);
#11533=ORIENTED_EDGE('',*,*,#8351,.T.);
#11534=ORIENTED_EDGE('',*,*,#8353,.F.);
#11535=ORIENTED_EDGE('',*,*,#8354,.F.);
#11536=ORIENTED_EDGE('',*,*,#8355,.F.);
#11537=ORIENTED_EDGE('',*,*,#8356,.F.);
#11538=ORIENTED_EDGE('',*,*,#8357,.F.);
#11539=ORIENTED_EDGE('',*,*,#8358,.F.);
#11540=ORIENTED_EDGE('',*,*,#8359,.T.);
#11541=ORIENTED_EDGE('',*,*,#8360,.F.);
#11542=ORIENTED_EDGE('',*,*,#8355,.T.);
#11543=ORIENTED_EDGE('',*,*,#8361,.F.);
#11544=ORIENTED_EDGE('',*,*,#8362,.F.);
#11545=ORIENTED_EDGE('',*,*,#8363,.F.);
#11546=ORIENTED_EDGE('',*,*,#8359,.F.);
#11547=ORIENTED_EDGE('',*,*,#8364,.T.);
#11548=ORIENTED_EDGE('',*,*,#8365,.T.);
#11549=ORIENTED_EDGE('',*,*,#8366,.T.);
#11550=ORIENTED_EDGE('',*,*,#8367,.T.);
#11551=ORIENTED_EDGE('',*,*,#8368,.T.);
#11552=ORIENTED_EDGE('',*,*,#8369,.T.);
#11553=ORIENTED_EDGE('',*,*,#8370,.T.);
#11554=ORIENTED_EDGE('',*,*,#8371,.T.);
#11555=ORIENTED_EDGE('',*,*,#8372,.T.);
#11556=ORIENTED_EDGE('',*,*,#8373,.T.);
#11557=ORIENTED_EDGE('',*,*,#8374,.T.);
#11558=ORIENTED_EDGE('',*,*,#8375,.T.);
#11559=ORIENTED_EDGE('',*,*,#8376,.T.);
#11560=ORIENTED_EDGE('',*,*,#8377,.T.);
#11561=ORIENTED_EDGE('',*,*,#8378,.T.);
#11562=ORIENTED_EDGE('',*,*,#8379,.T.);
#11563=ORIENTED_EDGE('',*,*,#8380,.T.);
#11564=ORIENTED_EDGE('',*,*,#8381,.T.);
#11565=ORIENTED_EDGE('',*,*,#8382,.T.);
#11566=ORIENTED_EDGE('',*,*,#8383,.T.);
#11567=ORIENTED_EDGE('',*,*,#8384,.T.);
#11568=ORIENTED_EDGE('',*,*,#8385,.T.);
#11569=ORIENTED_EDGE('',*,*,#8386,.T.);
#11570=ORIENTED_EDGE('',*,*,#8387,.T.);
#11571=ORIENTED_EDGE('',*,*,#8388,.T.);
#11572=ORIENTED_EDGE('',*,*,#8389,.T.);
#11573=ORIENTED_EDGE('',*,*,#8390,.T.);
#11574=ORIENTED_EDGE('',*,*,#8391,.T.);
#11575=ORIENTED_EDGE('',*,*,#8392,.T.);
#11576=ORIENTED_EDGE('',*,*,#8393,.T.);
#11577=ORIENTED_EDGE('',*,*,#8394,.T.);
#11578=ORIENTED_EDGE('',*,*,#8395,.T.);
#11579=ORIENTED_EDGE('',*,*,#8396,.T.);
#11580=ORIENTED_EDGE('',*,*,#8397,.T.);
#11581=ORIENTED_EDGE('',*,*,#8398,.T.);
#11582=ORIENTED_EDGE('',*,*,#8399,.T.);
#11583=ORIENTED_EDGE('',*,*,#8400,.T.);
#11584=ORIENTED_EDGE('',*,*,#8401,.T.);
#11585=ORIENTED_EDGE('',*,*,#8402,.T.);
#11586=ORIENTED_EDGE('',*,*,#8403,.T.);
#11587=ORIENTED_EDGE('',*,*,#8404,.T.);
#11588=ORIENTED_EDGE('',*,*,#8405,.T.);
#11589=ORIENTED_EDGE('',*,*,#8406,.T.);
#11590=ORIENTED_EDGE('',*,*,#8407,.T.);
#11591=ORIENTED_EDGE('',*,*,#8408,.T.);
#11592=ORIENTED_EDGE('',*,*,#8409,.T.);
#11593=ORIENTED_EDGE('',*,*,#8410,.T.);
#11594=ORIENTED_EDGE('',*,*,#8411,.T.);
#11595=ORIENTED_EDGE('',*,*,#8412,.T.);
#11596=ORIENTED_EDGE('',*,*,#8413,.T.);
#11597=ORIENTED_EDGE('',*,*,#8414,.T.);
#11598=ORIENTED_EDGE('',*,*,#8415,.T.);
#11599=ORIENTED_EDGE('',*,*,#8416,.T.);
#11600=ORIENTED_EDGE('',*,*,#8417,.T.);
#11601=ORIENTED_EDGE('',*,*,#8418,.T.);
#11602=ORIENTED_EDGE('',*,*,#8419,.T.);
#11603=ORIENTED_EDGE('',*,*,#8420,.T.);
#11604=ORIENTED_EDGE('',*,*,#8421,.T.);
#11605=ORIENTED_EDGE('',*,*,#8422,.T.);
#11606=ORIENTED_EDGE('',*,*,#8423,.T.);
#11607=ORIENTED_EDGE('',*,*,#8424,.T.);
#11608=ORIENTED_EDGE('',*,*,#8425,.T.);
#11609=ORIENTED_EDGE('',*,*,#8426,.T.);
#11610=ORIENTED_EDGE('',*,*,#8427,.T.);
#11611=ORIENTED_EDGE('',*,*,#8428,.T.);
#11612=ORIENTED_EDGE('',*,*,#8429,.T.);
#11613=ORIENTED_EDGE('',*,*,#8430,.T.);
#11614=ORIENTED_EDGE('',*,*,#8431,.T.);
#11615=ORIENTED_EDGE('',*,*,#8432,.T.);
#11616=ORIENTED_EDGE('',*,*,#8433,.T.);
#11617=ORIENTED_EDGE('',*,*,#8434,.T.);
#11618=ORIENTED_EDGE('',*,*,#8435,.T.);
#11619=ORIENTED_EDGE('',*,*,#8436,.T.);
#11620=ORIENTED_EDGE('',*,*,#8437,.T.);
#11621=ORIENTED_EDGE('',*,*,#8438,.T.);
#11622=ORIENTED_EDGE('',*,*,#8439,.T.);
#11623=ORIENTED_EDGE('',*,*,#8440,.T.);
#11624=ORIENTED_EDGE('',*,*,#8441,.T.);
#11625=ORIENTED_EDGE('',*,*,#8442,.T.);
#11626=ORIENTED_EDGE('',*,*,#8443,.T.);
#11627=ORIENTED_EDGE('',*,*,#8444,.T.);
#11628=ORIENTED_EDGE('',*,*,#8445,.T.);
#11629=ORIENTED_EDGE('',*,*,#8446,.T.);
#11630=ORIENTED_EDGE('',*,*,#8447,.T.);
#11631=ORIENTED_EDGE('',*,*,#8448,.T.);
#11632=ORIENTED_EDGE('',*,*,#8449,.T.);
#11633=ORIENTED_EDGE('',*,*,#8450,.T.);
#11634=ORIENTED_EDGE('',*,*,#8451,.T.);
#11635=ORIENTED_EDGE('',*,*,#8452,.T.);
#11636=ORIENTED_EDGE('',*,*,#8453,.T.);
#11637=ORIENTED_EDGE('',*,*,#8454,.T.);
#11638=ORIENTED_EDGE('',*,*,#8455,.T.);
#11639=ORIENTED_EDGE('',*,*,#8456,.T.);
#11640=ORIENTED_EDGE('',*,*,#8457,.T.);
#11641=ORIENTED_EDGE('',*,*,#8458,.T.);
#11642=ORIENTED_EDGE('',*,*,#8459,.T.);
#11643=ORIENTED_EDGE('',*,*,#8460,.T.);
#11644=ORIENTED_EDGE('',*,*,#8461,.T.);
#11645=ORIENTED_EDGE('',*,*,#8462,.T.);
#11646=ORIENTED_EDGE('',*,*,#8463,.T.);
#11647=ORIENTED_EDGE('',*,*,#8464,.T.);
#11648=ORIENTED_EDGE('',*,*,#8465,.T.);
#11649=ORIENTED_EDGE('',*,*,#8466,.T.);
#11650=ORIENTED_EDGE('',*,*,#8467,.T.);
#11651=ORIENTED_EDGE('',*,*,#8468,.T.);
#11652=ORIENTED_EDGE('',*,*,#8469,.T.);
#11653=ORIENTED_EDGE('',*,*,#8470,.T.);
#11654=ORIENTED_EDGE('',*,*,#8471,.T.);
#11655=ORIENTED_EDGE('',*,*,#8472,.T.);
#11656=ORIENTED_EDGE('',*,*,#8473,.T.);
#11657=ORIENTED_EDGE('',*,*,#8474,.T.);
#11658=ORIENTED_EDGE('',*,*,#8475,.T.);
#11659=ORIENTED_EDGE('',*,*,#8476,.T.);
#11660=ORIENTED_EDGE('',*,*,#8477,.T.);
#11661=ORIENTED_EDGE('',*,*,#8478,.T.);
#11662=ORIENTED_EDGE('',*,*,#8479,.T.);
#11663=ORIENTED_EDGE('',*,*,#8480,.T.);
#11664=ORIENTED_EDGE('',*,*,#8481,.T.);
#11665=ORIENTED_EDGE('',*,*,#8482,.T.);
#11666=ORIENTED_EDGE('',*,*,#8483,.T.);
#11667=ORIENTED_EDGE('',*,*,#8484,.T.);
#11668=ORIENTED_EDGE('',*,*,#8485,.T.);
#11669=ORIENTED_EDGE('',*,*,#8486,.T.);
#11670=ORIENTED_EDGE('',*,*,#8487,.T.);
#11671=ORIENTED_EDGE('',*,*,#8488,.T.);
#11672=ORIENTED_EDGE('',*,*,#8489,.T.);
#11673=ORIENTED_EDGE('',*,*,#8490,.T.);
#11674=ORIENTED_EDGE('',*,*,#8491,.T.);
#11675=ORIENTED_EDGE('',*,*,#8492,.T.);
#11676=ORIENTED_EDGE('',*,*,#8493,.T.);
#11677=ORIENTED_EDGE('',*,*,#8494,.T.);
#11678=ORIENTED_EDGE('',*,*,#8495,.T.);
#11679=ORIENTED_EDGE('',*,*,#8496,.T.);
#11680=ORIENTED_EDGE('',*,*,#8497,.T.);
#11681=ORIENTED_EDGE('',*,*,#8498,.T.);
#11682=ORIENTED_EDGE('',*,*,#8499,.T.);
#11683=ORIENTED_EDGE('',*,*,#8500,.T.);
#11684=ORIENTED_EDGE('',*,*,#8501,.T.);
#11685=ORIENTED_EDGE('',*,*,#8502,.T.);
#11686=ORIENTED_EDGE('',*,*,#8503,.T.);
#11687=ORIENTED_EDGE('',*,*,#8504,.T.);
#11688=ORIENTED_EDGE('',*,*,#8505,.T.);
#11689=ORIENTED_EDGE('',*,*,#8506,.T.);
#11690=ORIENTED_EDGE('',*,*,#8507,.T.);
#11691=ORIENTED_EDGE('',*,*,#8508,.T.);
#11692=ORIENTED_EDGE('',*,*,#8509,.T.);
#11693=ORIENTED_EDGE('',*,*,#8510,.T.);
#11694=ORIENTED_EDGE('',*,*,#8511,.T.);
#11695=ORIENTED_EDGE('',*,*,#8512,.T.);
#11696=ORIENTED_EDGE('',*,*,#8513,.T.);
#11697=ORIENTED_EDGE('',*,*,#8514,.T.);
#11698=ORIENTED_EDGE('',*,*,#8515,.T.);
#11699=ORIENTED_EDGE('',*,*,#8516,.T.);
#11700=ORIENTED_EDGE('',*,*,#8517,.T.);
#11701=ORIENTED_EDGE('',*,*,#8518,.T.);
#11702=ORIENTED_EDGE('',*,*,#8519,.T.);
#11703=ORIENTED_EDGE('',*,*,#8520,.T.);
#11704=ORIENTED_EDGE('',*,*,#8521,.T.);
#11705=ORIENTED_EDGE('',*,*,#8522,.T.);
#11706=ORIENTED_EDGE('',*,*,#8523,.T.);
#11707=ORIENTED_EDGE('',*,*,#8356,.T.);
#11708=ORIENTED_EDGE('',*,*,#8360,.T.);
#11709=ORIENTED_EDGE('',*,*,#8363,.T.);
#11710=ORIENTED_EDGE('',*,*,#8524,.T.);
#11711=ORIENTED_EDGE('',*,*,#8357,.T.);
#11712=ORIENTED_EDGE('',*,*,#8524,.F.);
#11713=ORIENTED_EDGE('',*,*,#8362,.T.);
#11714=ORIENTED_EDGE('',*,*,#8525,.F.);
#11715=ORIENTED_EDGE('',*,*,#8526,.F.);
#11716=ORIENTED_EDGE('',*,*,#8527,.T.);
#11717=ORIENTED_EDGE('',*,*,#8528,.F.);
#11718=ORIENTED_EDGE('',*,*,#8527,.F.);
#11719=ORIENTED_EDGE('',*,*,#8526,.T.);
#11720=ORIENTED_EDGE('',*,*,#8354,.T.);
#11721=ORIENTED_EDGE('',*,*,#8525,.T.);
#11722=ORIENTED_EDGE('',*,*,#8361,.T.);
#11723=ORIENTED_EDGE('',*,*,#8358,.T.);
#11724=ORIENTED_EDGE('',*,*,#8529,.F.);
#11725=ORIENTED_EDGE('',*,*,#8530,.F.);
#11726=ORIENTED_EDGE('',*,*,#8531,.F.);
#11727=ORIENTED_EDGE('',*,*,#8521,.F.);
#11728=ORIENTED_EDGE('',*,*,#8532,.F.);
#11729=ORIENTED_EDGE('',*,*,#8523,.F.);
#11730=ORIENTED_EDGE('',*,*,#8533,.T.);
#11731=ORIENTED_EDGE('',*,*,#8534,.F.);
#11732=ORIENTED_EDGE('',*,*,#8531,.T.);
#11733=ORIENTED_EDGE('',*,*,#8535,.F.);
#11734=ORIENTED_EDGE('',*,*,#8533,.F.);
#11735=ORIENTED_EDGE('',*,*,#8522,.F.);
#11736=ORIENTED_EDGE('',*,*,#8532,.T.);
#11737=ORIENTED_EDGE('',*,*,#8536,.F.);
#11738=ORIENTED_EDGE('',*,*,#8537,.T.);
#11739=ORIENTED_EDGE('',*,*,#8364,.F.);
#11740=ORIENTED_EDGE('',*,*,#8537,.F.);
#11741=ORIENTED_EDGE('',*,*,#8538,.F.);
#11742=ORIENTED_EDGE('',*,*,#8539,.F.);
#11743=ORIENTED_EDGE('',*,*,#8365,.F.);
#11744=ORIENTED_EDGE('',*,*,#8540,.F.);
#11745=ORIENTED_EDGE('',*,*,#8367,.F.);
#11746=ORIENTED_EDGE('',*,*,#8541,.T.);
#11747=ORIENTED_EDGE('',*,*,#8542,.F.);
#11748=ORIENTED_EDGE('',*,*,#8539,.T.);
#11749=ORIENTED_EDGE('',*,*,#8543,.F.);
#11750=ORIENTED_EDGE('',*,*,#8541,.F.);
#11751=ORIENTED_EDGE('',*,*,#8366,.F.);
#11752=ORIENTED_EDGE('',*,*,#8540,.T.);
#11753=ORIENTED_EDGE('',*,*,#8544,.F.);
#11754=ORIENTED_EDGE('',*,*,#8545,.T.);
#11755=ORIENTED_EDGE('',*,*,#8368,.F.);
#11756=ORIENTED_EDGE('',*,*,#8545,.F.);
#11757=ORIENTED_EDGE('',*,*,#8546,.F.);
#11758=ORIENTED_EDGE('',*,*,#8547,.F.);
#11759=ORIENTED_EDGE('',*,*,#8369,.F.);
#11760=ORIENTED_EDGE('',*,*,#8548,.F.);
#11761=ORIENTED_EDGE('',*,*,#8371,.F.);
#11762=ORIENTED_EDGE('',*,*,#8549,.T.);
#11763=ORIENTED_EDGE('',*,*,#8550,.F.);
#11764=ORIENTED_EDGE('',*,*,#8547,.T.);
#11765=ORIENTED_EDGE('',*,*,#8551,.F.);
#11766=ORIENTED_EDGE('',*,*,#8549,.F.);
#11767=ORIENTED_EDGE('',*,*,#8370,.F.);
#11768=ORIENTED_EDGE('',*,*,#8548,.T.);
#11769=ORIENTED_EDGE('',*,*,#8552,.F.);
#11770=ORIENTED_EDGE('',*,*,#8553,.T.);
#11771=ORIENTED_EDGE('',*,*,#8372,.F.);
#11772=ORIENTED_EDGE('',*,*,#8553,.F.);
#11773=ORIENTED_EDGE('',*,*,#8554,.F.);
#11774=ORIENTED_EDGE('',*,*,#8555,.F.);
#11775=ORIENTED_EDGE('',*,*,#8373,.F.);
#11776=ORIENTED_EDGE('',*,*,#8556,.F.);
#11777=ORIENTED_EDGE('',*,*,#8375,.F.);
#11778=ORIENTED_EDGE('',*,*,#8557,.T.);
#11779=ORIENTED_EDGE('',*,*,#8558,.F.);
#11780=ORIENTED_EDGE('',*,*,#8555,.T.);
#11781=ORIENTED_EDGE('',*,*,#8559,.F.);
#11782=ORIENTED_EDGE('',*,*,#8557,.F.);
#11783=ORIENTED_EDGE('',*,*,#8374,.F.);
#11784=ORIENTED_EDGE('',*,*,#8556,.T.);
#11785=ORIENTED_EDGE('',*,*,#8560,.F.);
#11786=ORIENTED_EDGE('',*,*,#8561,.T.);
#11787=ORIENTED_EDGE('',*,*,#8376,.F.);
#11788=ORIENTED_EDGE('',*,*,#8561,.F.);
#11789=ORIENTED_EDGE('',*,*,#8562,.F.);
#11790=ORIENTED_EDGE('',*,*,#8563,.F.);
#11791=ORIENTED_EDGE('',*,*,#8377,.F.);
#11792=ORIENTED_EDGE('',*,*,#8564,.F.);
#11793=ORIENTED_EDGE('',*,*,#8379,.F.);
#11794=ORIENTED_EDGE('',*,*,#8565,.T.);
#11795=ORIENTED_EDGE('',*,*,#8566,.F.);
#11796=ORIENTED_EDGE('',*,*,#8563,.T.);
#11797=ORIENTED_EDGE('',*,*,#8567,.F.);
#11798=ORIENTED_EDGE('',*,*,#8565,.F.);
#11799=ORIENTED_EDGE('',*,*,#8378,.F.);
#11800=ORIENTED_EDGE('',*,*,#8564,.T.);
#11801=ORIENTED_EDGE('',*,*,#8568,.F.);
#11802=ORIENTED_EDGE('',*,*,#8569,.T.);
#11803=ORIENTED_EDGE('',*,*,#8380,.F.);
#11804=ORIENTED_EDGE('',*,*,#8569,.F.);
#11805=ORIENTED_EDGE('',*,*,#8570,.F.);
#11806=ORIENTED_EDGE('',*,*,#8571,.F.);
#11807=ORIENTED_EDGE('',*,*,#8381,.F.);
#11808=ORIENTED_EDGE('',*,*,#8572,.F.);
#11809=ORIENTED_EDGE('',*,*,#8383,.F.);
#11810=ORIENTED_EDGE('',*,*,#8573,.T.);
#11811=ORIENTED_EDGE('',*,*,#8574,.F.);
#11812=ORIENTED_EDGE('',*,*,#8571,.T.);
#11813=ORIENTED_EDGE('',*,*,#8575,.F.);
#11814=ORIENTED_EDGE('',*,*,#8573,.F.);
#11815=ORIENTED_EDGE('',*,*,#8382,.F.);
#11816=ORIENTED_EDGE('',*,*,#8572,.T.);
#11817=ORIENTED_EDGE('',*,*,#8576,.F.);
#11818=ORIENTED_EDGE('',*,*,#8577,.T.);
#11819=ORIENTED_EDGE('',*,*,#8384,.F.);
#11820=ORIENTED_EDGE('',*,*,#8577,.F.);
#11821=ORIENTED_EDGE('',*,*,#8578,.F.);
#11822=ORIENTED_EDGE('',*,*,#8579,.F.);
#11823=ORIENTED_EDGE('',*,*,#8385,.F.);
#11824=ORIENTED_EDGE('',*,*,#8580,.F.);
#11825=ORIENTED_EDGE('',*,*,#8387,.F.);
#11826=ORIENTED_EDGE('',*,*,#8581,.T.);
#11827=ORIENTED_EDGE('',*,*,#8582,.F.);
#11828=ORIENTED_EDGE('',*,*,#8579,.T.);
#11829=ORIENTED_EDGE('',*,*,#8583,.F.);
#11830=ORIENTED_EDGE('',*,*,#8581,.F.);
#11831=ORIENTED_EDGE('',*,*,#8386,.F.);
#11832=ORIENTED_EDGE('',*,*,#8580,.T.);
#11833=ORIENTED_EDGE('',*,*,#8584,.F.);
#11834=ORIENTED_EDGE('',*,*,#8585,.T.);
#11835=ORIENTED_EDGE('',*,*,#8388,.F.);
#11836=ORIENTED_EDGE('',*,*,#8585,.F.);
#11837=ORIENTED_EDGE('',*,*,#8586,.F.);
#11838=ORIENTED_EDGE('',*,*,#8587,.F.);
#11839=ORIENTED_EDGE('',*,*,#8389,.F.);
#11840=ORIENTED_EDGE('',*,*,#8588,.F.);
#11841=ORIENTED_EDGE('',*,*,#8391,.F.);
#11842=ORIENTED_EDGE('',*,*,#8589,.T.);
#11843=ORIENTED_EDGE('',*,*,#8590,.F.);
#11844=ORIENTED_EDGE('',*,*,#8587,.T.);
#11845=ORIENTED_EDGE('',*,*,#8591,.F.);
#11846=ORIENTED_EDGE('',*,*,#8589,.F.);
#11847=ORIENTED_EDGE('',*,*,#8390,.F.);
#11848=ORIENTED_EDGE('',*,*,#8588,.T.);
#11849=ORIENTED_EDGE('',*,*,#8592,.F.);
#11850=ORIENTED_EDGE('',*,*,#8593,.T.);
#11851=ORIENTED_EDGE('',*,*,#8392,.F.);
#11852=ORIENTED_EDGE('',*,*,#8593,.F.);
#11853=ORIENTED_EDGE('',*,*,#8594,.F.);
#11854=ORIENTED_EDGE('',*,*,#8595,.F.);
#11855=ORIENTED_EDGE('',*,*,#8393,.F.);
#11856=ORIENTED_EDGE('',*,*,#8596,.F.);
#11857=ORIENTED_EDGE('',*,*,#8395,.F.);
#11858=ORIENTED_EDGE('',*,*,#8597,.T.);
#11859=ORIENTED_EDGE('',*,*,#8598,.F.);
#11860=ORIENTED_EDGE('',*,*,#8595,.T.);
#11861=ORIENTED_EDGE('',*,*,#8599,.F.);
#11862=ORIENTED_EDGE('',*,*,#8597,.F.);
#11863=ORIENTED_EDGE('',*,*,#8394,.F.);
#11864=ORIENTED_EDGE('',*,*,#8596,.T.);
#11865=ORIENTED_EDGE('',*,*,#8600,.F.);
#11866=ORIENTED_EDGE('',*,*,#8601,.T.);
#11867=ORIENTED_EDGE('',*,*,#8396,.F.);
#11868=ORIENTED_EDGE('',*,*,#8601,.F.);
#11869=ORIENTED_EDGE('',*,*,#8602,.F.);
#11870=ORIENTED_EDGE('',*,*,#8603,.F.);
#11871=ORIENTED_EDGE('',*,*,#8397,.F.);
#11872=ORIENTED_EDGE('',*,*,#8604,.F.);
#11873=ORIENTED_EDGE('',*,*,#8399,.F.);
#11874=ORIENTED_EDGE('',*,*,#8605,.T.);
#11875=ORIENTED_EDGE('',*,*,#8606,.F.);
#11876=ORIENTED_EDGE('',*,*,#8603,.T.);
#11877=ORIENTED_EDGE('',*,*,#8607,.F.);
#11878=ORIENTED_EDGE('',*,*,#8605,.F.);
#11879=ORIENTED_EDGE('',*,*,#8398,.F.);
#11880=ORIENTED_EDGE('',*,*,#8604,.T.);
#11881=ORIENTED_EDGE('',*,*,#8608,.F.);
#11882=ORIENTED_EDGE('',*,*,#8609,.T.);
#11883=ORIENTED_EDGE('',*,*,#8400,.F.);
#11884=ORIENTED_EDGE('',*,*,#8609,.F.);
#11885=ORIENTED_EDGE('',*,*,#8610,.F.);
#11886=ORIENTED_EDGE('',*,*,#8611,.F.);
#11887=ORIENTED_EDGE('',*,*,#8401,.F.);
#11888=ORIENTED_EDGE('',*,*,#8612,.F.);
#11889=ORIENTED_EDGE('',*,*,#8403,.F.);
#11890=ORIENTED_EDGE('',*,*,#8613,.T.);
#11891=ORIENTED_EDGE('',*,*,#8614,.F.);
#11892=ORIENTED_EDGE('',*,*,#8611,.T.);
#11893=ORIENTED_EDGE('',*,*,#8615,.F.);
#11894=ORIENTED_EDGE('',*,*,#8613,.F.);
#11895=ORIENTED_EDGE('',*,*,#8402,.F.);
#11896=ORIENTED_EDGE('',*,*,#8612,.T.);
#11897=ORIENTED_EDGE('',*,*,#8616,.F.);
#11898=ORIENTED_EDGE('',*,*,#8617,.T.);
#11899=ORIENTED_EDGE('',*,*,#8404,.F.);
#11900=ORIENTED_EDGE('',*,*,#8617,.F.);
#11901=ORIENTED_EDGE('',*,*,#8618,.F.);
#11902=ORIENTED_EDGE('',*,*,#8619,.F.);
#11903=ORIENTED_EDGE('',*,*,#8405,.F.);
#11904=ORIENTED_EDGE('',*,*,#8620,.F.);
#11905=ORIENTED_EDGE('',*,*,#8407,.F.);
#11906=ORIENTED_EDGE('',*,*,#8621,.T.);
#11907=ORIENTED_EDGE('',*,*,#8622,.F.);
#11908=ORIENTED_EDGE('',*,*,#8619,.T.);
#11909=ORIENTED_EDGE('',*,*,#8623,.F.);
#11910=ORIENTED_EDGE('',*,*,#8621,.F.);
#11911=ORIENTED_EDGE('',*,*,#8406,.F.);
#11912=ORIENTED_EDGE('',*,*,#8620,.T.);
#11913=ORIENTED_EDGE('',*,*,#8624,.F.);
#11914=ORIENTED_EDGE('',*,*,#8625,.T.);
#11915=ORIENTED_EDGE('',*,*,#8408,.F.);
#11916=ORIENTED_EDGE('',*,*,#8625,.F.);
#11917=ORIENTED_EDGE('',*,*,#8626,.F.);
#11918=ORIENTED_EDGE('',*,*,#8627,.F.);
#11919=ORIENTED_EDGE('',*,*,#8409,.F.);
#11920=ORIENTED_EDGE('',*,*,#8628,.F.);
#11921=ORIENTED_EDGE('',*,*,#8411,.F.);
#11922=ORIENTED_EDGE('',*,*,#8629,.T.);
#11923=ORIENTED_EDGE('',*,*,#8630,.F.);
#11924=ORIENTED_EDGE('',*,*,#8627,.T.);
#11925=ORIENTED_EDGE('',*,*,#8631,.F.);
#11926=ORIENTED_EDGE('',*,*,#8629,.F.);
#11927=ORIENTED_EDGE('',*,*,#8410,.F.);
#11928=ORIENTED_EDGE('',*,*,#8628,.T.);
#11929=ORIENTED_EDGE('',*,*,#8632,.F.);
#11930=ORIENTED_EDGE('',*,*,#8633,.T.);
#11931=ORIENTED_EDGE('',*,*,#8412,.F.);
#11932=ORIENTED_EDGE('',*,*,#8633,.F.);
#11933=ORIENTED_EDGE('',*,*,#8634,.F.);
#11934=ORIENTED_EDGE('',*,*,#8635,.F.);
#11935=ORIENTED_EDGE('',*,*,#8413,.F.);
#11936=ORIENTED_EDGE('',*,*,#8636,.F.);
#11937=ORIENTED_EDGE('',*,*,#8415,.F.);
#11938=ORIENTED_EDGE('',*,*,#8637,.T.);
#11939=ORIENTED_EDGE('',*,*,#8638,.F.);
#11940=ORIENTED_EDGE('',*,*,#8635,.T.);
#11941=ORIENTED_EDGE('',*,*,#8639,.F.);
#11942=ORIENTED_EDGE('',*,*,#8637,.F.);
#11943=ORIENTED_EDGE('',*,*,#8414,.F.);
#11944=ORIENTED_EDGE('',*,*,#8636,.T.);
#11945=ORIENTED_EDGE('',*,*,#8640,.F.);
#11946=ORIENTED_EDGE('',*,*,#8641,.T.);
#11947=ORIENTED_EDGE('',*,*,#8416,.F.);
#11948=ORIENTED_EDGE('',*,*,#8641,.F.);
#11949=ORIENTED_EDGE('',*,*,#8642,.F.);
#11950=ORIENTED_EDGE('',*,*,#8643,.F.);
#11951=ORIENTED_EDGE('',*,*,#8417,.F.);
#11952=ORIENTED_EDGE('',*,*,#8644,.F.);
#11953=ORIENTED_EDGE('',*,*,#8419,.F.);
#11954=ORIENTED_EDGE('',*,*,#8645,.T.);
#11955=ORIENTED_EDGE('',*,*,#8646,.F.);
#11956=ORIENTED_EDGE('',*,*,#8643,.T.);
#11957=ORIENTED_EDGE('',*,*,#8647,.F.);
#11958=ORIENTED_EDGE('',*,*,#8645,.F.);
#11959=ORIENTED_EDGE('',*,*,#8418,.F.);
#11960=ORIENTED_EDGE('',*,*,#8644,.T.);
#11961=ORIENTED_EDGE('',*,*,#8648,.F.);
#11962=ORIENTED_EDGE('',*,*,#8649,.T.);
#11963=ORIENTED_EDGE('',*,*,#8420,.F.);
#11964=ORIENTED_EDGE('',*,*,#8649,.F.);
#11965=ORIENTED_EDGE('',*,*,#8650,.F.);
#11966=ORIENTED_EDGE('',*,*,#8651,.F.);
#11967=ORIENTED_EDGE('',*,*,#8421,.F.);
#11968=ORIENTED_EDGE('',*,*,#8652,.F.);
#11969=ORIENTED_EDGE('',*,*,#8423,.F.);
#11970=ORIENTED_EDGE('',*,*,#8653,.T.);
#11971=ORIENTED_EDGE('',*,*,#8654,.F.);
#11972=ORIENTED_EDGE('',*,*,#8651,.T.);
#11973=ORIENTED_EDGE('',*,*,#8655,.F.);
#11974=ORIENTED_EDGE('',*,*,#8653,.F.);
#11975=ORIENTED_EDGE('',*,*,#8422,.F.);
#11976=ORIENTED_EDGE('',*,*,#8652,.T.);
#11977=ORIENTED_EDGE('',*,*,#8656,.F.);
#11978=ORIENTED_EDGE('',*,*,#8657,.T.);
#11979=ORIENTED_EDGE('',*,*,#8424,.F.);
#11980=ORIENTED_EDGE('',*,*,#8657,.F.);
#11981=ORIENTED_EDGE('',*,*,#8658,.F.);
#11982=ORIENTED_EDGE('',*,*,#8659,.F.);
#11983=ORIENTED_EDGE('',*,*,#8425,.F.);
#11984=ORIENTED_EDGE('',*,*,#8660,.F.);
#11985=ORIENTED_EDGE('',*,*,#8427,.F.);
#11986=ORIENTED_EDGE('',*,*,#8661,.T.);
#11987=ORIENTED_EDGE('',*,*,#8662,.F.);
#11988=ORIENTED_EDGE('',*,*,#8659,.T.);
#11989=ORIENTED_EDGE('',*,*,#8663,.F.);
#11990=ORIENTED_EDGE('',*,*,#8661,.F.);
#11991=ORIENTED_EDGE('',*,*,#8426,.F.);
#11992=ORIENTED_EDGE('',*,*,#8660,.T.);
#11993=ORIENTED_EDGE('',*,*,#8664,.F.);
#11994=ORIENTED_EDGE('',*,*,#8665,.T.);
#11995=ORIENTED_EDGE('',*,*,#8428,.F.);
#11996=ORIENTED_EDGE('',*,*,#8665,.F.);
#11997=ORIENTED_EDGE('',*,*,#8666,.F.);
#11998=ORIENTED_EDGE('',*,*,#8667,.F.);
#11999=ORIENTED_EDGE('',*,*,#8429,.F.);
#12000=ORIENTED_EDGE('',*,*,#8668,.F.);
#12001=ORIENTED_EDGE('',*,*,#8431,.F.);
#12002=ORIENTED_EDGE('',*,*,#8669,.T.);
#12003=ORIENTED_EDGE('',*,*,#8670,.F.);
#12004=ORIENTED_EDGE('',*,*,#8667,.T.);
#12005=ORIENTED_EDGE('',*,*,#8671,.F.);
#12006=ORIENTED_EDGE('',*,*,#8669,.F.);
#12007=ORIENTED_EDGE('',*,*,#8430,.F.);
#12008=ORIENTED_EDGE('',*,*,#8668,.T.);
#12009=ORIENTED_EDGE('',*,*,#8672,.F.);
#12010=ORIENTED_EDGE('',*,*,#8673,.T.);
#12011=ORIENTED_EDGE('',*,*,#8432,.F.);
#12012=ORIENTED_EDGE('',*,*,#8673,.F.);
#12013=ORIENTED_EDGE('',*,*,#8674,.F.);
#12014=ORIENTED_EDGE('',*,*,#8675,.F.);
#12015=ORIENTED_EDGE('',*,*,#8433,.F.);
#12016=ORIENTED_EDGE('',*,*,#8676,.F.);
#12017=ORIENTED_EDGE('',*,*,#8435,.F.);
#12018=ORIENTED_EDGE('',*,*,#8677,.T.);
#12019=ORIENTED_EDGE('',*,*,#8678,.F.);
#12020=ORIENTED_EDGE('',*,*,#8675,.T.);
#12021=ORIENTED_EDGE('',*,*,#8679,.F.);
#12022=ORIENTED_EDGE('',*,*,#8677,.F.);
#12023=ORIENTED_EDGE('',*,*,#8434,.F.);
#12024=ORIENTED_EDGE('',*,*,#8676,.T.);
#12025=ORIENTED_EDGE('',*,*,#8680,.F.);
#12026=ORIENTED_EDGE('',*,*,#8681,.T.);
#12027=ORIENTED_EDGE('',*,*,#8436,.F.);
#12028=ORIENTED_EDGE('',*,*,#8681,.F.);
#12029=ORIENTED_EDGE('',*,*,#8682,.F.);
#12030=ORIENTED_EDGE('',*,*,#8683,.F.);
#12031=ORIENTED_EDGE('',*,*,#8437,.F.);
#12032=ORIENTED_EDGE('',*,*,#8684,.F.);
#12033=ORIENTED_EDGE('',*,*,#8439,.F.);
#12034=ORIENTED_EDGE('',*,*,#8685,.T.);
#12035=ORIENTED_EDGE('',*,*,#8686,.F.);
#12036=ORIENTED_EDGE('',*,*,#8683,.T.);
#12037=ORIENTED_EDGE('',*,*,#8687,.F.);
#12038=ORIENTED_EDGE('',*,*,#8685,.F.);
#12039=ORIENTED_EDGE('',*,*,#8438,.F.);
#12040=ORIENTED_EDGE('',*,*,#8684,.T.);
#12041=ORIENTED_EDGE('',*,*,#8688,.F.);
#12042=ORIENTED_EDGE('',*,*,#8689,.T.);
#12043=ORIENTED_EDGE('',*,*,#8440,.F.);
#12044=ORIENTED_EDGE('',*,*,#8689,.F.);
#12045=ORIENTED_EDGE('',*,*,#8690,.F.);
#12046=ORIENTED_EDGE('',*,*,#8691,.F.);
#12047=ORIENTED_EDGE('',*,*,#8441,.F.);
#12048=ORIENTED_EDGE('',*,*,#8692,.F.);
#12049=ORIENTED_EDGE('',*,*,#8443,.F.);
#12050=ORIENTED_EDGE('',*,*,#8693,.T.);
#12051=ORIENTED_EDGE('',*,*,#8694,.F.);
#12052=ORIENTED_EDGE('',*,*,#8691,.T.);
#12053=ORIENTED_EDGE('',*,*,#8695,.F.);
#12054=ORIENTED_EDGE('',*,*,#8693,.F.);
#12055=ORIENTED_EDGE('',*,*,#8442,.F.);
#12056=ORIENTED_EDGE('',*,*,#8692,.T.);
#12057=ORIENTED_EDGE('',*,*,#8696,.F.);
#12058=ORIENTED_EDGE('',*,*,#8697,.T.);
#12059=ORIENTED_EDGE('',*,*,#8444,.F.);
#12060=ORIENTED_EDGE('',*,*,#8697,.F.);
#12061=ORIENTED_EDGE('',*,*,#8698,.F.);
#12062=ORIENTED_EDGE('',*,*,#8699,.F.);
#12063=ORIENTED_EDGE('',*,*,#8445,.F.);
#12064=ORIENTED_EDGE('',*,*,#8700,.F.);
#12065=ORIENTED_EDGE('',*,*,#8447,.F.);
#12066=ORIENTED_EDGE('',*,*,#8701,.T.);
#12067=ORIENTED_EDGE('',*,*,#8702,.F.);
#12068=ORIENTED_EDGE('',*,*,#8699,.T.);
#12069=ORIENTED_EDGE('',*,*,#8703,.F.);
#12070=ORIENTED_EDGE('',*,*,#8701,.F.);
#12071=ORIENTED_EDGE('',*,*,#8446,.F.);
#12072=ORIENTED_EDGE('',*,*,#8700,.T.);
#12073=ORIENTED_EDGE('',*,*,#8704,.F.);
#12074=ORIENTED_EDGE('',*,*,#8705,.T.);
#12075=ORIENTED_EDGE('',*,*,#8448,.F.);
#12076=ORIENTED_EDGE('',*,*,#8705,.F.);
#12077=ORIENTED_EDGE('',*,*,#8706,.F.);
#12078=ORIENTED_EDGE('',*,*,#8707,.F.);
#12079=ORIENTED_EDGE('',*,*,#8449,.F.);
#12080=ORIENTED_EDGE('',*,*,#8708,.F.);
#12081=ORIENTED_EDGE('',*,*,#8451,.F.);
#12082=ORIENTED_EDGE('',*,*,#8709,.T.);
#12083=ORIENTED_EDGE('',*,*,#8710,.F.);
#12084=ORIENTED_EDGE('',*,*,#8707,.T.);
#12085=ORIENTED_EDGE('',*,*,#8711,.F.);
#12086=ORIENTED_EDGE('',*,*,#8709,.F.);
#12087=ORIENTED_EDGE('',*,*,#8450,.F.);
#12088=ORIENTED_EDGE('',*,*,#8708,.T.);
#12089=ORIENTED_EDGE('',*,*,#8712,.F.);
#12090=ORIENTED_EDGE('',*,*,#8713,.T.);
#12091=ORIENTED_EDGE('',*,*,#8452,.F.);
#12092=ORIENTED_EDGE('',*,*,#8713,.F.);
#12093=ORIENTED_EDGE('',*,*,#8714,.F.);
#12094=ORIENTED_EDGE('',*,*,#8715,.F.);
#12095=ORIENTED_EDGE('',*,*,#8453,.F.);
#12096=ORIENTED_EDGE('',*,*,#8716,.F.);
#12097=ORIENTED_EDGE('',*,*,#8455,.F.);
#12098=ORIENTED_EDGE('',*,*,#8717,.T.);
#12099=ORIENTED_EDGE('',*,*,#8718,.F.);
#12100=ORIENTED_EDGE('',*,*,#8715,.T.);
#12101=ORIENTED_EDGE('',*,*,#8719,.F.);
#12102=ORIENTED_EDGE('',*,*,#8717,.F.);
#12103=ORIENTED_EDGE('',*,*,#8454,.F.);
#12104=ORIENTED_EDGE('',*,*,#8716,.T.);
#12105=ORIENTED_EDGE('',*,*,#8720,.F.);
#12106=ORIENTED_EDGE('',*,*,#8721,.T.);
#12107=ORIENTED_EDGE('',*,*,#8456,.F.);
#12108=ORIENTED_EDGE('',*,*,#8721,.F.);
#12109=ORIENTED_EDGE('',*,*,#8722,.F.);
#12110=ORIENTED_EDGE('',*,*,#8723,.F.);
#12111=ORIENTED_EDGE('',*,*,#8457,.F.);
#12112=ORIENTED_EDGE('',*,*,#8724,.F.);
#12113=ORIENTED_EDGE('',*,*,#8459,.F.);
#12114=ORIENTED_EDGE('',*,*,#8725,.T.);
#12115=ORIENTED_EDGE('',*,*,#8726,.F.);
#12116=ORIENTED_EDGE('',*,*,#8723,.T.);
#12117=ORIENTED_EDGE('',*,*,#8727,.F.);
#12118=ORIENTED_EDGE('',*,*,#8725,.F.);
#12119=ORIENTED_EDGE('',*,*,#8458,.F.);
#12120=ORIENTED_EDGE('',*,*,#8724,.T.);
#12121=ORIENTED_EDGE('',*,*,#8728,.F.);
#12122=ORIENTED_EDGE('',*,*,#8729,.T.);
#12123=ORIENTED_EDGE('',*,*,#8460,.F.);
#12124=ORIENTED_EDGE('',*,*,#8729,.F.);
#12125=ORIENTED_EDGE('',*,*,#8730,.F.);
#12126=ORIENTED_EDGE('',*,*,#8731,.F.);
#12127=ORIENTED_EDGE('',*,*,#8461,.F.);
#12128=ORIENTED_EDGE('',*,*,#8732,.F.);
#12129=ORIENTED_EDGE('',*,*,#8463,.F.);
#12130=ORIENTED_EDGE('',*,*,#8733,.T.);
#12131=ORIENTED_EDGE('',*,*,#8734,.F.);
#12132=ORIENTED_EDGE('',*,*,#8731,.T.);
#12133=ORIENTED_EDGE('',*,*,#8735,.F.);
#12134=ORIENTED_EDGE('',*,*,#8733,.F.);
#12135=ORIENTED_EDGE('',*,*,#8462,.F.);
#12136=ORIENTED_EDGE('',*,*,#8732,.T.);
#12137=ORIENTED_EDGE('',*,*,#8736,.F.);
#12138=ORIENTED_EDGE('',*,*,#8737,.T.);
#12139=ORIENTED_EDGE('',*,*,#8464,.F.);
#12140=ORIENTED_EDGE('',*,*,#8737,.F.);
#12141=ORIENTED_EDGE('',*,*,#8738,.F.);
#12142=ORIENTED_EDGE('',*,*,#8739,.F.);
#12143=ORIENTED_EDGE('',*,*,#8465,.F.);
#12144=ORIENTED_EDGE('',*,*,#8740,.F.);
#12145=ORIENTED_EDGE('',*,*,#8467,.F.);
#12146=ORIENTED_EDGE('',*,*,#8741,.T.);
#12147=ORIENTED_EDGE('',*,*,#8742,.F.);
#12148=ORIENTED_EDGE('',*,*,#8739,.T.);
#12149=ORIENTED_EDGE('',*,*,#8743,.F.);
#12150=ORIENTED_EDGE('',*,*,#8741,.F.);
#12151=ORIENTED_EDGE('',*,*,#8466,.F.);
#12152=ORIENTED_EDGE('',*,*,#8740,.T.);
#12153=ORIENTED_EDGE('',*,*,#8744,.F.);
#12154=ORIENTED_EDGE('',*,*,#8745,.T.);
#12155=ORIENTED_EDGE('',*,*,#8468,.F.);
#12156=ORIENTED_EDGE('',*,*,#8745,.F.);
#12157=ORIENTED_EDGE('',*,*,#8746,.F.);
#12158=ORIENTED_EDGE('',*,*,#8747,.F.);
#12159=ORIENTED_EDGE('',*,*,#8469,.F.);
#12160=ORIENTED_EDGE('',*,*,#8748,.F.);
#12161=ORIENTED_EDGE('',*,*,#8471,.F.);
#12162=ORIENTED_EDGE('',*,*,#8749,.T.);
#12163=ORIENTED_EDGE('',*,*,#8750,.F.);
#12164=ORIENTED_EDGE('',*,*,#8747,.T.);
#12165=ORIENTED_EDGE('',*,*,#8751,.F.);
#12166=ORIENTED_EDGE('',*,*,#8749,.F.);
#12167=ORIENTED_EDGE('',*,*,#8470,.F.);
#12168=ORIENTED_EDGE('',*,*,#8748,.T.);
#12169=ORIENTED_EDGE('',*,*,#8752,.F.);
#12170=ORIENTED_EDGE('',*,*,#8753,.T.);
#12171=ORIENTED_EDGE('',*,*,#8472,.F.);
#12172=ORIENTED_EDGE('',*,*,#8753,.F.);
#12173=ORIENTED_EDGE('',*,*,#8754,.F.);
#12174=ORIENTED_EDGE('',*,*,#8755,.F.);
#12175=ORIENTED_EDGE('',*,*,#8473,.F.);
#12176=ORIENTED_EDGE('',*,*,#8756,.F.);
#12177=ORIENTED_EDGE('',*,*,#8475,.F.);
#12178=ORIENTED_EDGE('',*,*,#8757,.T.);
#12179=ORIENTED_EDGE('',*,*,#8758,.F.);
#12180=ORIENTED_EDGE('',*,*,#8755,.T.);
#12181=ORIENTED_EDGE('',*,*,#8759,.F.);
#12182=ORIENTED_EDGE('',*,*,#8757,.F.);
#12183=ORIENTED_EDGE('',*,*,#8474,.F.);
#12184=ORIENTED_EDGE('',*,*,#8756,.T.);
#12185=ORIENTED_EDGE('',*,*,#8760,.F.);
#12186=ORIENTED_EDGE('',*,*,#8761,.T.);
#12187=ORIENTED_EDGE('',*,*,#8476,.F.);
#12188=ORIENTED_EDGE('',*,*,#8761,.F.);
#12189=ORIENTED_EDGE('',*,*,#8762,.F.);
#12190=ORIENTED_EDGE('',*,*,#8763,.F.);
#12191=ORIENTED_EDGE('',*,*,#8477,.F.);
#12192=ORIENTED_EDGE('',*,*,#8764,.F.);
#12193=ORIENTED_EDGE('',*,*,#8479,.F.);
#12194=ORIENTED_EDGE('',*,*,#8765,.T.);
#12195=ORIENTED_EDGE('',*,*,#8766,.F.);
#12196=ORIENTED_EDGE('',*,*,#8763,.T.);
#12197=ORIENTED_EDGE('',*,*,#8767,.F.);
#12198=ORIENTED_EDGE('',*,*,#8765,.F.);
#12199=ORIENTED_EDGE('',*,*,#8478,.F.);
#12200=ORIENTED_EDGE('',*,*,#8764,.T.);
#12201=ORIENTED_EDGE('',*,*,#8768,.F.);
#12202=ORIENTED_EDGE('',*,*,#8769,.T.);
#12203=ORIENTED_EDGE('',*,*,#8480,.F.);
#12204=ORIENTED_EDGE('',*,*,#8769,.F.);
#12205=ORIENTED_EDGE('',*,*,#8770,.F.);
#12206=ORIENTED_EDGE('',*,*,#8771,.F.);
#12207=ORIENTED_EDGE('',*,*,#8481,.F.);
#12208=ORIENTED_EDGE('',*,*,#8772,.F.);
#12209=ORIENTED_EDGE('',*,*,#8483,.F.);
#12210=ORIENTED_EDGE('',*,*,#8773,.T.);
#12211=ORIENTED_EDGE('',*,*,#8774,.F.);
#12212=ORIENTED_EDGE('',*,*,#8771,.T.);
#12213=ORIENTED_EDGE('',*,*,#8775,.F.);
#12214=ORIENTED_EDGE('',*,*,#8773,.F.);
#12215=ORIENTED_EDGE('',*,*,#8482,.F.);
#12216=ORIENTED_EDGE('',*,*,#8772,.T.);
#12217=ORIENTED_EDGE('',*,*,#8776,.F.);
#12218=ORIENTED_EDGE('',*,*,#8777,.T.);
#12219=ORIENTED_EDGE('',*,*,#8484,.F.);
#12220=ORIENTED_EDGE('',*,*,#8777,.F.);
#12221=ORIENTED_EDGE('',*,*,#8778,.F.);
#12222=ORIENTED_EDGE('',*,*,#8779,.F.);
#12223=ORIENTED_EDGE('',*,*,#8485,.F.);
#12224=ORIENTED_EDGE('',*,*,#8780,.F.);
#12225=ORIENTED_EDGE('',*,*,#8487,.F.);
#12226=ORIENTED_EDGE('',*,*,#8781,.T.);
#12227=ORIENTED_EDGE('',*,*,#8782,.F.);
#12228=ORIENTED_EDGE('',*,*,#8779,.T.);
#12229=ORIENTED_EDGE('',*,*,#8783,.F.);
#12230=ORIENTED_EDGE('',*,*,#8781,.F.);
#12231=ORIENTED_EDGE('',*,*,#8486,.F.);
#12232=ORIENTED_EDGE('',*,*,#8780,.T.);
#12233=ORIENTED_EDGE('',*,*,#8784,.F.);
#12234=ORIENTED_EDGE('',*,*,#8785,.T.);
#12235=ORIENTED_EDGE('',*,*,#8488,.F.);
#12236=ORIENTED_EDGE('',*,*,#8785,.F.);
#12237=ORIENTED_EDGE('',*,*,#8786,.F.);
#12238=ORIENTED_EDGE('',*,*,#8787,.F.);
#12239=ORIENTED_EDGE('',*,*,#8489,.F.);
#12240=ORIENTED_EDGE('',*,*,#8788,.F.);
#12241=ORIENTED_EDGE('',*,*,#8491,.F.);
#12242=ORIENTED_EDGE('',*,*,#8789,.T.);
#12243=ORIENTED_EDGE('',*,*,#8790,.F.);
#12244=ORIENTED_EDGE('',*,*,#8787,.T.);
#12245=ORIENTED_EDGE('',*,*,#8791,.F.);
#12246=ORIENTED_EDGE('',*,*,#8789,.F.);
#12247=ORIENTED_EDGE('',*,*,#8490,.F.);
#12248=ORIENTED_EDGE('',*,*,#8788,.T.);
#12249=ORIENTED_EDGE('',*,*,#8792,.F.);
#12250=ORIENTED_EDGE('',*,*,#8793,.T.);
#12251=ORIENTED_EDGE('',*,*,#8492,.F.);
#12252=ORIENTED_EDGE('',*,*,#8793,.F.);
#12253=ORIENTED_EDGE('',*,*,#8794,.F.);
#12254=ORIENTED_EDGE('',*,*,#8795,.F.);
#12255=ORIENTED_EDGE('',*,*,#8493,.F.);
#12256=ORIENTED_EDGE('',*,*,#8796,.F.);
#12257=ORIENTED_EDGE('',*,*,#8495,.F.);
#12258=ORIENTED_EDGE('',*,*,#8797,.T.);
#12259=ORIENTED_EDGE('',*,*,#8798,.F.);
#12260=ORIENTED_EDGE('',*,*,#8795,.T.);
#12261=ORIENTED_EDGE('',*,*,#8799,.F.);
#12262=ORIENTED_EDGE('',*,*,#8797,.F.);
#12263=ORIENTED_EDGE('',*,*,#8494,.F.);
#12264=ORIENTED_EDGE('',*,*,#8796,.T.);
#12265=ORIENTED_EDGE('',*,*,#8800,.F.);
#12266=ORIENTED_EDGE('',*,*,#8801,.T.);
#12267=ORIENTED_EDGE('',*,*,#8496,.F.);
#12268=ORIENTED_EDGE('',*,*,#8801,.F.);
#12269=ORIENTED_EDGE('',*,*,#8802,.F.);
#12270=ORIENTED_EDGE('',*,*,#8803,.F.);
#12271=ORIENTED_EDGE('',*,*,#8497,.F.);
#12272=ORIENTED_EDGE('',*,*,#8804,.F.);
#12273=ORIENTED_EDGE('',*,*,#8499,.F.);
#12274=ORIENTED_EDGE('',*,*,#8805,.T.);
#12275=ORIENTED_EDGE('',*,*,#8806,.F.);
#12276=ORIENTED_EDGE('',*,*,#8803,.T.);
#12277=ORIENTED_EDGE('',*,*,#8807,.F.);
#12278=ORIENTED_EDGE('',*,*,#8805,.F.);
#12279=ORIENTED_EDGE('',*,*,#8498,.F.);
#12280=ORIENTED_EDGE('',*,*,#8804,.T.);
#12281=ORIENTED_EDGE('',*,*,#8808,.F.);
#12282=ORIENTED_EDGE('',*,*,#8809,.T.);
#12283=ORIENTED_EDGE('',*,*,#8500,.F.);
#12284=ORIENTED_EDGE('',*,*,#8809,.F.);
#12285=ORIENTED_EDGE('',*,*,#8810,.F.);
#12286=ORIENTED_EDGE('',*,*,#8811,.F.);
#12287=ORIENTED_EDGE('',*,*,#8501,.F.);
#12288=ORIENTED_EDGE('',*,*,#8812,.F.);
#12289=ORIENTED_EDGE('',*,*,#8503,.F.);
#12290=ORIENTED_EDGE('',*,*,#8813,.T.);
#12291=ORIENTED_EDGE('',*,*,#8814,.F.);
#12292=ORIENTED_EDGE('',*,*,#8811,.T.);
#12293=ORIENTED_EDGE('',*,*,#8815,.F.);
#12294=ORIENTED_EDGE('',*,*,#8813,.F.);
#12295=ORIENTED_EDGE('',*,*,#8502,.F.);
#12296=ORIENTED_EDGE('',*,*,#8812,.T.);
#12297=ORIENTED_EDGE('',*,*,#8816,.F.);
#12298=ORIENTED_EDGE('',*,*,#8817,.T.);
#12299=ORIENTED_EDGE('',*,*,#8504,.F.);
#12300=ORIENTED_EDGE('',*,*,#8817,.F.);
#12301=ORIENTED_EDGE('',*,*,#8818,.F.);
#12302=ORIENTED_EDGE('',*,*,#8819,.F.);
#12303=ORIENTED_EDGE('',*,*,#8505,.F.);
#12304=ORIENTED_EDGE('',*,*,#8820,.F.);
#12305=ORIENTED_EDGE('',*,*,#8507,.F.);
#12306=ORIENTED_EDGE('',*,*,#8821,.T.);
#12307=ORIENTED_EDGE('',*,*,#8822,.F.);
#12308=ORIENTED_EDGE('',*,*,#8819,.T.);
#12309=ORIENTED_EDGE('',*,*,#8823,.F.);
#12310=ORIENTED_EDGE('',*,*,#8821,.F.);
#12311=ORIENTED_EDGE('',*,*,#8506,.F.);
#12312=ORIENTED_EDGE('',*,*,#8820,.T.);
#12313=ORIENTED_EDGE('',*,*,#8824,.F.);
#12314=ORIENTED_EDGE('',*,*,#8825,.T.);
#12315=ORIENTED_EDGE('',*,*,#8508,.F.);
#12316=ORIENTED_EDGE('',*,*,#8825,.F.);
#12317=ORIENTED_EDGE('',*,*,#8826,.F.);
#12318=ORIENTED_EDGE('',*,*,#8827,.F.);
#12319=ORIENTED_EDGE('',*,*,#8509,.F.);
#12320=ORIENTED_EDGE('',*,*,#8828,.F.);
#12321=ORIENTED_EDGE('',*,*,#8511,.F.);
#12322=ORIENTED_EDGE('',*,*,#8829,.T.);
#12323=ORIENTED_EDGE('',*,*,#8830,.F.);
#12324=ORIENTED_EDGE('',*,*,#8827,.T.);
#12325=ORIENTED_EDGE('',*,*,#8831,.F.);
#12326=ORIENTED_EDGE('',*,*,#8829,.F.);
#12327=ORIENTED_EDGE('',*,*,#8510,.F.);
#12328=ORIENTED_EDGE('',*,*,#8828,.T.);
#12329=ORIENTED_EDGE('',*,*,#8832,.F.);
#12330=ORIENTED_EDGE('',*,*,#8833,.T.);
#12331=ORIENTED_EDGE('',*,*,#8512,.F.);
#12332=ORIENTED_EDGE('',*,*,#8833,.F.);
#12333=ORIENTED_EDGE('',*,*,#8834,.F.);
#12334=ORIENTED_EDGE('',*,*,#8835,.F.);
#12335=ORIENTED_EDGE('',*,*,#8513,.F.);
#12336=ORIENTED_EDGE('',*,*,#8835,.T.);
#12337=ORIENTED_EDGE('',*,*,#8836,.F.);
#12338=ORIENTED_EDGE('',*,*,#8837,.F.);
#12339=ORIENTED_EDGE('',*,*,#8514,.F.);
#12340=ORIENTED_EDGE('',*,*,#8838,.F.);
#12341=ORIENTED_EDGE('',*,*,#8515,.F.);
#12342=ORIENTED_EDGE('',*,*,#8837,.T.);
#12343=ORIENTED_EDGE('',*,*,#8839,.F.);
#12344=ORIENTED_EDGE('',*,*,#8838,.T.);
#12345=ORIENTED_EDGE('',*,*,#8840,.F.);
#12346=ORIENTED_EDGE('',*,*,#8841,.T.);
#12347=ORIENTED_EDGE('',*,*,#8516,.F.);
#12348=ORIENTED_EDGE('',*,*,#8842,.F.);
#12349=ORIENTED_EDGE('',*,*,#8519,.F.);
#12350=ORIENTED_EDGE('',*,*,#8843,.T.);
#12351=ORIENTED_EDGE('',*,*,#8844,.F.);
#12352=ORIENTED_EDGE('',*,*,#8841,.F.);
#12353=ORIENTED_EDGE('',*,*,#8845,.F.);
#12354=ORIENTED_EDGE('',*,*,#8846,.F.);
#12355=ORIENTED_EDGE('',*,*,#8517,.F.);
#12356=ORIENTED_EDGE('',*,*,#8846,.T.);
#12357=ORIENTED_EDGE('',*,*,#8847,.F.);
#12358=ORIENTED_EDGE('',*,*,#8843,.F.);
#12359=ORIENTED_EDGE('',*,*,#8518,.F.);
#12360=ORIENTED_EDGE('',*,*,#8534,.T.);
#12361=ORIENTED_EDGE('',*,*,#8535,.T.);
#12362=ORIENTED_EDGE('',*,*,#8530,.T.);
#12363=ORIENTED_EDGE('',*,*,#8848,.T.);
#12364=ORIENTED_EDGE('',*,*,#8844,.T.);
#12365=ORIENTED_EDGE('',*,*,#8847,.T.);
#12366=ORIENTED_EDGE('',*,*,#8845,.T.);
#12367=ORIENTED_EDGE('',*,*,#8840,.T.);
#12368=ORIENTED_EDGE('',*,*,#8839,.T.);
#12369=ORIENTED_EDGE('',*,*,#8836,.T.);
#12370=ORIENTED_EDGE('',*,*,#8834,.T.);
#12371=ORIENTED_EDGE('',*,*,#8832,.T.);
#12372=ORIENTED_EDGE('',*,*,#8830,.T.);
#12373=ORIENTED_EDGE('',*,*,#8831,.T.);
#12374=ORIENTED_EDGE('',*,*,#8826,.T.);
#12375=ORIENTED_EDGE('',*,*,#8824,.T.);
#12376=ORIENTED_EDGE('',*,*,#8822,.T.);
#12377=ORIENTED_EDGE('',*,*,#8823,.T.);
#12378=ORIENTED_EDGE('',*,*,#8818,.T.);
#12379=ORIENTED_EDGE('',*,*,#8816,.T.);
#12380=ORIENTED_EDGE('',*,*,#8814,.T.);
#12381=ORIENTED_EDGE('',*,*,#8815,.T.);
#12382=ORIENTED_EDGE('',*,*,#8810,.T.);
#12383=ORIENTED_EDGE('',*,*,#8808,.T.);
#12384=ORIENTED_EDGE('',*,*,#8806,.T.);
#12385=ORIENTED_EDGE('',*,*,#8807,.T.);
#12386=ORIENTED_EDGE('',*,*,#8802,.T.);
#12387=ORIENTED_EDGE('',*,*,#8800,.T.);
#12388=ORIENTED_EDGE('',*,*,#8798,.T.);
#12389=ORIENTED_EDGE('',*,*,#8799,.T.);
#12390=ORIENTED_EDGE('',*,*,#8794,.T.);
#12391=ORIENTED_EDGE('',*,*,#8792,.T.);
#12392=ORIENTED_EDGE('',*,*,#8790,.T.);
#12393=ORIENTED_EDGE('',*,*,#8791,.T.);
#12394=ORIENTED_EDGE('',*,*,#8786,.T.);
#12395=ORIENTED_EDGE('',*,*,#8784,.T.);
#12396=ORIENTED_EDGE('',*,*,#8782,.T.);
#12397=ORIENTED_EDGE('',*,*,#8783,.T.);
#12398=ORIENTED_EDGE('',*,*,#8778,.T.);
#12399=ORIENTED_EDGE('',*,*,#8776,.T.);
#12400=ORIENTED_EDGE('',*,*,#8774,.T.);
#12401=ORIENTED_EDGE('',*,*,#8775,.T.);
#12402=ORIENTED_EDGE('',*,*,#8770,.T.);
#12403=ORIENTED_EDGE('',*,*,#8768,.T.);
#12404=ORIENTED_EDGE('',*,*,#8766,.T.);
#12405=ORIENTED_EDGE('',*,*,#8767,.T.);
#12406=ORIENTED_EDGE('',*,*,#8762,.T.);
#12407=ORIENTED_EDGE('',*,*,#8760,.T.);
#12408=ORIENTED_EDGE('',*,*,#8758,.T.);
#12409=ORIENTED_EDGE('',*,*,#8759,.T.);
#12410=ORIENTED_EDGE('',*,*,#8754,.T.);
#12411=ORIENTED_EDGE('',*,*,#8752,.T.);
#12412=ORIENTED_EDGE('',*,*,#8750,.T.);
#12413=ORIENTED_EDGE('',*,*,#8751,.T.);
#12414=ORIENTED_EDGE('',*,*,#8746,.T.);
#12415=ORIENTED_EDGE('',*,*,#8744,.T.);
#12416=ORIENTED_EDGE('',*,*,#8742,.T.);
#12417=ORIENTED_EDGE('',*,*,#8743,.T.);
#12418=ORIENTED_EDGE('',*,*,#8738,.T.);
#12419=ORIENTED_EDGE('',*,*,#8736,.T.);
#12420=ORIENTED_EDGE('',*,*,#8734,.T.);
#12421=ORIENTED_EDGE('',*,*,#8735,.T.);
#12422=ORIENTED_EDGE('',*,*,#8730,.T.);
#12423=ORIENTED_EDGE('',*,*,#8728,.T.);
#12424=ORIENTED_EDGE('',*,*,#8726,.T.);
#12425=ORIENTED_EDGE('',*,*,#8727,.T.);
#12426=ORIENTED_EDGE('',*,*,#8722,.T.);
#12427=ORIENTED_EDGE('',*,*,#8720,.T.);
#12428=ORIENTED_EDGE('',*,*,#8718,.T.);
#12429=ORIENTED_EDGE('',*,*,#8719,.T.);
#12430=ORIENTED_EDGE('',*,*,#8714,.T.);
#12431=ORIENTED_EDGE('',*,*,#8712,.T.);
#12432=ORIENTED_EDGE('',*,*,#8710,.T.);
#12433=ORIENTED_EDGE('',*,*,#8711,.T.);
#12434=ORIENTED_EDGE('',*,*,#8706,.T.);
#12435=ORIENTED_EDGE('',*,*,#8704,.T.);
#12436=ORIENTED_EDGE('',*,*,#8702,.T.);
#12437=ORIENTED_EDGE('',*,*,#8703,.T.);
#12438=ORIENTED_EDGE('',*,*,#8698,.T.);
#12439=ORIENTED_EDGE('',*,*,#8696,.T.);
#12440=ORIENTED_EDGE('',*,*,#8694,.T.);
#12441=ORIENTED_EDGE('',*,*,#8695,.T.);
#12442=ORIENTED_EDGE('',*,*,#8690,.T.);
#12443=ORIENTED_EDGE('',*,*,#8688,.T.);
#12444=ORIENTED_EDGE('',*,*,#8686,.T.);
#12445=ORIENTED_EDGE('',*,*,#8687,.T.);
#12446=ORIENTED_EDGE('',*,*,#8682,.T.);
#12447=ORIENTED_EDGE('',*,*,#8680,.T.);
#12448=ORIENTED_EDGE('',*,*,#8678,.T.);
#12449=ORIENTED_EDGE('',*,*,#8679,.T.);
#12450=ORIENTED_EDGE('',*,*,#8674,.T.);
#12451=ORIENTED_EDGE('',*,*,#8672,.T.);
#12452=ORIENTED_EDGE('',*,*,#8670,.T.);
#12453=ORIENTED_EDGE('',*,*,#8671,.T.);
#12454=ORIENTED_EDGE('',*,*,#8666,.T.);
#12455=ORIENTED_EDGE('',*,*,#8664,.T.);
#12456=ORIENTED_EDGE('',*,*,#8662,.T.);
#12457=ORIENTED_EDGE('',*,*,#8663,.T.);
#12458=ORIENTED_EDGE('',*,*,#8658,.T.);
#12459=ORIENTED_EDGE('',*,*,#8656,.T.);
#12460=ORIENTED_EDGE('',*,*,#8654,.T.);
#12461=ORIENTED_EDGE('',*,*,#8655,.T.);
#12462=ORIENTED_EDGE('',*,*,#8650,.T.);
#12463=ORIENTED_EDGE('',*,*,#8648,.T.);
#12464=ORIENTED_EDGE('',*,*,#8646,.T.);
#12465=ORIENTED_EDGE('',*,*,#8647,.T.);
#12466=ORIENTED_EDGE('',*,*,#8642,.T.);
#12467=ORIENTED_EDGE('',*,*,#8640,.T.);
#12468=ORIENTED_EDGE('',*,*,#8638,.T.);
#12469=ORIENTED_EDGE('',*,*,#8639,.T.);
#12470=ORIENTED_EDGE('',*,*,#8634,.T.);
#12471=ORIENTED_EDGE('',*,*,#8632,.T.);
#12472=ORIENTED_EDGE('',*,*,#8630,.T.);
#12473=ORIENTED_EDGE('',*,*,#8631,.T.);
#12474=ORIENTED_EDGE('',*,*,#8626,.T.);
#12475=ORIENTED_EDGE('',*,*,#8624,.T.);
#12476=ORIENTED_EDGE('',*,*,#8622,.T.);
#12477=ORIENTED_EDGE('',*,*,#8623,.T.);
#12478=ORIENTED_EDGE('',*,*,#8618,.T.);
#12479=ORIENTED_EDGE('',*,*,#8616,.T.);
#12480=ORIENTED_EDGE('',*,*,#8614,.T.);
#12481=ORIENTED_EDGE('',*,*,#8615,.T.);
#12482=ORIENTED_EDGE('',*,*,#8610,.T.);
#12483=ORIENTED_EDGE('',*,*,#8608,.T.);
#12484=ORIENTED_EDGE('',*,*,#8606,.T.);
#12485=ORIENTED_EDGE('',*,*,#8607,.T.);
#12486=ORIENTED_EDGE('',*,*,#8602,.T.);
#12487=ORIENTED_EDGE('',*,*,#8600,.T.);
#12488=ORIENTED_EDGE('',*,*,#8598,.T.);
#12489=ORIENTED_EDGE('',*,*,#8599,.T.);
#12490=ORIENTED_EDGE('',*,*,#8594,.T.);
#12491=ORIENTED_EDGE('',*,*,#8592,.T.);
#12492=ORIENTED_EDGE('',*,*,#8590,.T.);
#12493=ORIENTED_EDGE('',*,*,#8591,.T.);
#12494=ORIENTED_EDGE('',*,*,#8586,.T.);
#12495=ORIENTED_EDGE('',*,*,#8584,.T.);
#12496=ORIENTED_EDGE('',*,*,#8582,.T.);
#12497=ORIENTED_EDGE('',*,*,#8583,.T.);
#12498=ORIENTED_EDGE('',*,*,#8578,.T.);
#12499=ORIENTED_EDGE('',*,*,#8576,.T.);
#12500=ORIENTED_EDGE('',*,*,#8574,.T.);
#12501=ORIENTED_EDGE('',*,*,#8575,.T.);
#12502=ORIENTED_EDGE('',*,*,#8570,.T.);
#12503=ORIENTED_EDGE('',*,*,#8568,.T.);
#12504=ORIENTED_EDGE('',*,*,#8566,.T.);
#12505=ORIENTED_EDGE('',*,*,#8567,.T.);
#12506=ORIENTED_EDGE('',*,*,#8562,.T.);
#12507=ORIENTED_EDGE('',*,*,#8560,.T.);
#12508=ORIENTED_EDGE('',*,*,#8558,.T.);
#12509=ORIENTED_EDGE('',*,*,#8559,.T.);
#12510=ORIENTED_EDGE('',*,*,#8554,.T.);
#12511=ORIENTED_EDGE('',*,*,#8552,.T.);
#12512=ORIENTED_EDGE('',*,*,#8550,.T.);
#12513=ORIENTED_EDGE('',*,*,#8551,.T.);
#12514=ORIENTED_EDGE('',*,*,#8546,.T.);
#12515=ORIENTED_EDGE('',*,*,#8544,.T.);
#12516=ORIENTED_EDGE('',*,*,#8542,.T.);
#12517=ORIENTED_EDGE('',*,*,#8543,.T.);
#12518=ORIENTED_EDGE('',*,*,#8538,.T.);
#12519=ORIENTED_EDGE('',*,*,#8536,.T.);
#12520=ORIENTED_EDGE('',*,*,#8528,.T.);
#12521=ORIENTED_EDGE('',*,*,#8529,.T.);
#12522=ORIENTED_EDGE('',*,*,#8520,.F.);
#12523=ORIENTED_EDGE('',*,*,#8842,.T.);
#12524=ORIENTED_EDGE('',*,*,#8848,.F.);
#12525=ORIENTED_EDGE('',*,*,#8849,.T.);
#12526=ORIENTED_EDGE('',*,*,#8850,.T.);
#12527=ORIENTED_EDGE('',*,*,#8851,.T.);
#12528=ORIENTED_EDGE('',*,*,#8852,.F.);
#12529=ORIENTED_EDGE('',*,*,#8853,.T.);
#12530=ORIENTED_EDGE('',*,*,#8854,.T.);
#12531=ORIENTED_EDGE('',*,*,#8855,.T.);
#12532=ORIENTED_EDGE('',*,*,#8850,.F.);
#12533=ORIENTED_EDGE('',*,*,#8856,.T.);
#12534=ORIENTED_EDGE('',*,*,#8857,.T.);
#12535=ORIENTED_EDGE('',*,*,#8858,.T.);
#12536=ORIENTED_EDGE('',*,*,#8854,.F.);
#12537=ORIENTED_EDGE('',*,*,#8859,.T.);
#12538=ORIENTED_EDGE('',*,*,#8860,.T.);
#12539=ORIENTED_EDGE('',*,*,#8861,.T.);
#12540=ORIENTED_EDGE('',*,*,#8857,.F.);
#12541=ORIENTED_EDGE('',*,*,#8862,.T.);
#12542=ORIENTED_EDGE('',*,*,#8863,.T.);
#12543=ORIENTED_EDGE('',*,*,#8864,.T.);
#12544=ORIENTED_EDGE('',*,*,#8860,.F.);
#12545=ORIENTED_EDGE('',*,*,#8865,.T.);
#12546=ORIENTED_EDGE('',*,*,#8852,.T.);
#12547=ORIENTED_EDGE('',*,*,#8866,.T.);
#12548=ORIENTED_EDGE('',*,*,#8863,.F.);
#12549=ORIENTED_EDGE('',*,*,#8865,.F.);
#12550=ORIENTED_EDGE('',*,*,#8862,.F.);
#12551=ORIENTED_EDGE('',*,*,#8859,.F.);
#12552=ORIENTED_EDGE('',*,*,#8856,.F.);
#12553=ORIENTED_EDGE('',*,*,#8853,.F.);
#12554=ORIENTED_EDGE('',*,*,#8849,.F.);
#12555=ORIENTED_EDGE('',*,*,#8866,.F.);
#12556=ORIENTED_EDGE('',*,*,#8851,.F.);
#12557=ORIENTED_EDGE('',*,*,#8855,.F.);
#12558=ORIENTED_EDGE('',*,*,#8858,.F.);
#12559=ORIENTED_EDGE('',*,*,#8861,.F.);
#12560=ORIENTED_EDGE('',*,*,#8864,.F.);
#12561=ORIENTED_EDGE('',*,*,#8867,.F.);
#12562=ORIENTED_EDGE('',*,*,#8868,.F.);
#12563=ORIENTED_EDGE('',*,*,#8869,.F.);
#12564=ORIENTED_EDGE('',*,*,#8870,.T.);
#12565=ORIENTED_EDGE('',*,*,#8868,.T.);
#12566=ORIENTED_EDGE('',*,*,#8870,.F.);
#12567=ORIENTED_EDGE('',*,*,#8871,.F.);
#12568=ORIENTED_EDGE('',*,*,#8872,.T.);
#12569=ORIENTED_EDGE('',*,*,#8869,.T.);
#12570=ORIENTED_EDGE('',*,*,#8872,.F.);
#12571=ORIENTED_EDGE('',*,*,#8873,.F.);
#12572=ORIENTED_EDGE('',*,*,#8874,.T.);
#12573=ORIENTED_EDGE('',*,*,#8871,.T.);
#12574=ORIENTED_EDGE('',*,*,#8874,.F.);
#12575=ORIENTED_EDGE('',*,*,#8873,.T.);
#12576=ORIENTED_EDGE('',*,*,#8875,.F.);
#12577=ORIENTED_EDGE('',*,*,#8876,.F.);
#12578=ORIENTED_EDGE('',*,*,#8877,.T.);
#12579=ORIENTED_EDGE('',*,*,#8875,.T.);
#12580=ORIENTED_EDGE('',*,*,#8877,.F.);
#12581=ORIENTED_EDGE('',*,*,#8867,.T.);
#12582=ORIENTED_EDGE('',*,*,#8878,.T.);
#12583=ORIENTED_EDGE('',*,*,#8876,.T.);
#12584=ORIENTED_EDGE('',*,*,#8878,.F.);
#12585=CYLINDRICAL_SURFACE('',#14198,0.164999999999999);
#12586=CYLINDRICAL_SURFACE('',#14201,0.164999999999999);
#12587=CYLINDRICAL_SURFACE('',#14204,0.164999999999999);
#12588=CYLINDRICAL_SURFACE('',#14207,0.164999999999999);
#12589=CYLINDRICAL_SURFACE('',#14210,0.21);
#12590=CYLINDRICAL_SURFACE('',#14213,0.21);
#12591=CYLINDRICAL_SURFACE('',#14216,0.21);
#12592=CYLINDRICAL_SURFACE('',#14219,0.21);
#12593=CYLINDRICAL_SURFACE('',#14222,0.164999999999999);
#12594=CYLINDRICAL_SURFACE('',#14225,0.164999999999999);
#12595=CYLINDRICAL_SURFACE('',#14228,0.165);
#12596=CYLINDRICAL_SURFACE('',#14231,0.165);
#12597=CYLINDRICAL_SURFACE('',#14255,0.25);
#12598=CYLINDRICAL_SURFACE('',#14256,0.165);
#12599=CYLINDRICAL_SURFACE('',#14260,0.165);
#12600=CYLINDRICAL_SURFACE('',#14264,0.165);
#12601=CYLINDRICAL_SURFACE('',#14268,0.165);
#12602=CYLINDRICAL_SURFACE('',#14275,0.525);
#12603=CYLINDRICAL_SURFACE('',#14277,0.525);
#12604=CYLINDRICAL_SURFACE('',#14282,0.525);
#12605=CYLINDRICAL_SURFACE('',#14287,0.525);
#12606=CYLINDRICAL_SURFACE('',#14292,2.2);
#12607=CYLINDRICAL_SURFACE('',#14305,0.275);
#12608=CYLINDRICAL_SURFACE('',#14307,0.275);
#12609=CYLINDRICAL_SURFACE('',#14309,0.275);
#12610=CYLINDRICAL_SURFACE('',#14311,0.275);
#12611=CYLINDRICAL_SURFACE('',#14313,1.6);
#12612=CYLINDRICAL_SURFACE('',#14318,3.);
#12613=CYLINDRICAL_SURFACE('',#14320,1.3);
#12614=CYLINDRICAL_SURFACE('',#14325,1.1);
#12615=CYLINDRICAL_SURFACE('',#14328,1.59);
#12616=CYLINDRICAL_SURFACE('',#14334,0.225);
#12617=CYLINDRICAL_SURFACE('',#14337,0.225);
#12618=CYLINDRICAL_SURFACE('',#14340,0.225);
#12619=CYLINDRICAL_SURFACE('',#14343,0.225);
#12620=CYLINDRICAL_SURFACE('',#14352,2.2);
#12621=CYLINDRICAL_SURFACE('',#14354,2.2);
#12622=CYLINDRICAL_SURFACE('',#14356,2.2);
#12623=CYLINDRICAL_SURFACE('',#14358,2.2);
#12624=CYLINDRICAL_SURFACE('',#14360,1.59);
#12625=CYLINDRICAL_SURFACE('',#14364,1.1);
#12626=CYLINDRICAL_SURFACE('',#14368,0.225);
#12627=CYLINDRICAL_SURFACE('',#14371,0.225);
#12628=CYLINDRICAL_SURFACE('',#14374,0.225);
#12629=CYLINDRICAL_SURFACE('',#14377,0.225);
#12630=CYLINDRICAL_SURFACE('',#14380,0.6);
#12631=CYLINDRICAL_SURFACE('',#14384,1.5);
#12632=CYLINDRICAL_SURFACE('',#14392,0.164999999999999);
#12633=CYLINDRICAL_SURFACE('',#14396,1.);
#12634=CYLINDRICAL_SURFACE('',#14422,0.605);
#12635=CYLINDRICAL_SURFACE('',#14424,1.5);
#12636=CYLINDRICAL_SURFACE('',#14433,0.205);
#12637=CYLINDRICAL_SURFACE('',#14436,1.);
#12638=CYLINDRICAL_SURFACE('',#14442,1.);
#12639=CYLINDRICAL_SURFACE('',#14448,0.2);
#12640=CYLINDRICAL_SURFACE('',#14454,0.375);
#12641=CYLINDRICAL_SURFACE('',#14459,0.375);
#12642=CYLINDRICAL_SURFACE('',#14464,0.375);
#12643=CYLINDRICAL_SURFACE('',#14469,0.375);
#12644=CYLINDRICAL_SURFACE('',#14474,0.225);
#12645=CYLINDRICAL_SURFACE('',#14476,0.225);
#12646=CYLINDRICAL_SURFACE('',#14478,0.225);
#12647=CYLINDRICAL_SURFACE('',#14480,0.225000000000001);
#12648=CYLINDRICAL_SURFACE('',#14504,1.070235);
#12649=CYLINDRICAL_SURFACE('',#14506,0.6);
#12650=CYLINDRICAL_SURFACE('',#14512,1.070235);
#12651=CYLINDRICAL_SURFACE('',#14524,1.129765);
#12652=CYLINDRICAL_SURFACE('',#14531,1.6);
#12653=CYLINDRICAL_SURFACE('',#14536,1.129765);
#12654=CYLINDRICAL_SURFACE('',#14556,1.123812);
#12655=CYLINDRICAL_SURFACE('',#14592,1.076188);
#12656=CYLINDRICAL_SURFACE('',#14606,1.119765);
#12657=CYLINDRICAL_SURFACE('',#14610,1.085235);
#12658=CYLINDRICAL_SURFACE('',#14614,1.119765);
#12659=CYLINDRICAL_SURFACE('',#14618,1.085235);
#12660=CYLINDRICAL_SURFACE('',#14629,0.35);
#12661=CYLINDRICAL_SURFACE('',#14637,0.1954);
#12662=CYLINDRICAL_SURFACE('',#14652,0.21);
#12663=CYLINDRICAL_SURFACE('',#14655,0.21);
#12664=CYLINDRICAL_SURFACE('',#14658,0.210000000000001);
#12665=CYLINDRICAL_SURFACE('',#14661,0.210000000000001);
#12666=CYLINDRICAL_SURFACE('',#14664,0.164999999999999);
#12667=CYLINDRICAL_SURFACE('',#14672,0.275);
#12668=CYLINDRICAL_SURFACE('',#14675,0.275);
#12669=CYLINDRICAL_SURFACE('',#14678,0.275);
#12670=CYLINDRICAL_SURFACE('',#14681,0.275);
#12671=CYLINDRICAL_SURFACE('',#14684,2.42);
#12672=CYLINDRICAL_SURFACE('',#14702,0.25);
#12673=CYLINDRICAL_SURFACE('',#14703,0.165);
#12674=CYLINDRICAL_SURFACE('',#14707,0.165);
#12675=CYLINDRICAL_SURFACE('',#14711,0.164999999999999);
#12676=CYLINDRICAL_SURFACE('',#14715,0.165);
#12677=CYLINDRICAL_SURFACE('',#14719,0.525);
#12678=CYLINDRICAL_SURFACE('',#14724,0.525);
#12679=CYLINDRICAL_SURFACE('',#14729,0.525);
#12680=CYLINDRICAL_SURFACE('',#14734,0.525);
#12681=CYLINDRICAL_SURFACE('',#14739,0.275);
#12682=CYLINDRICAL_SURFACE('',#14752,0.275);
#12683=CYLINDRICAL_SURFACE('',#14754,0.275);
#12684=CYLINDRICAL_SURFACE('',#14756,0.275);
#12685=CYLINDRICAL_SURFACE('',#14758,3.);
#12686=CYLINDRICAL_SURFACE('',#14760,2.35);
#12687=CYLINDRICAL_SURFACE('',#14765,3.5);
#12688=CYLINDRICAL_SURFACE('',#14767,1.6);
#12689=CYLINDRICAL_SURFACE('',#14772,1.7);
#12690=CYLINDRICAL_SURFACE('',#14775,2.34);
#12691=CYLINDRICAL_SURFACE('',#14781,0.225);
#12692=CYLINDRICAL_SURFACE('',#14784,0.225);
#12693=CYLINDRICAL_SURFACE('',#14787,0.225);
#12694=CYLINDRICAL_SURFACE('',#14790,0.225000000000001);
#12695=CYLINDRICAL_SURFACE('',#14793,1.7);
#12696=CYLINDRICAL_SURFACE('',#14796,3.);
#12697=CYLINDRICAL_SURFACE('',#14805,0.21);
#12698=CYLINDRICAL_SURFACE('',#14811,0.21);
#12699=CYLINDRICAL_SURFACE('',#14817,0.21);
#12700=CYLINDRICAL_SURFACE('',#14823,0.21);
#12701=CYLINDRICAL_SURFACE('',#14878,0.1954);
#12702=CYLINDRICAL_SURFACE('',#14898,0.425);
#12703=CYLINDRICAL_SURFACE('',#14906,0.24505);
#12704=CYLINDRICAL_SURFACE('',#14915,1.63531);
#12705=CYLINDRICAL_SURFACE('',#14917,1.);
#12706=CYLINDRICAL_SURFACE('',#14923,1.63531);
#12707=CYLINDRICAL_SURFACE('',#14935,1.71469);
#12708=CYLINDRICAL_SURFACE('',#14942,2.35);
#12709=CYLINDRICAL_SURFACE('',#14947,1.71469);
#12710=CYLINDRICAL_SURFACE('',#14969,1.706752);
#12711=CYLINDRICAL_SURFACE('',#15009,1.643248);
#12712=CYLINDRICAL_SURFACE('',#15023,1.70469);
#12713=CYLINDRICAL_SURFACE('',#15027,1.65031);
#12714=CYLINDRICAL_SURFACE('',#15031,1.70469);
#12715=CYLINDRICAL_SURFACE('',#15035,1.65031);
#12716=CYLINDRICAL_SURFACE('',#15043,0.165);
#12717=CYLINDRICAL_SURFACE('',#15060,0.8);
#12718=CYLINDRICAL_SURFACE('',#15061,0.6);
#12719=CYLINDRICAL_SURFACE('',#15063,0.6);
#12720=CYLINDRICAL_SURFACE('',#15068,0.605);
#12721=CYLINDRICAL_SURFACE('',#15071,0.8);
#12722=CYLINDRICAL_SURFACE('',#15077,0.605);
#12723=CYLINDRICAL_SURFACE('',#15080,0.8);
#12724=CYLINDRICAL_SURFACE('',#15086,0.605);
#12725=CYLINDRICAL_SURFACE('',#15089,0.8);
#12726=CYLINDRICAL_SURFACE('',#15101,0.165);
#12727=CYLINDRICAL_SURFACE('',#15104,0.605);
#12728=CYLINDRICAL_SURFACE('',#15107,1.2);
#12729=CYLINDRICAL_SURFACE('',#15120,0.225);
#12730=CYLINDRICAL_SURFACE('',#15123,0.9);
#12731=CYLINDRICAL_SURFACE('',#15154,0.6);
#12732=CYLINDRICAL_SURFACE('',#15156,1.4);
#12733=CYLINDRICAL_SURFACE('',#15161,1.75);
#12734=CYLINDRICAL_SURFACE('',#15164,1.75);
#12735=CYLINDRICAL_SURFACE('',#15167,1.75);
#12736=CYLINDRICAL_SURFACE('',#15170,1.75);
#12737=CYLINDRICAL_SURFACE('',#15173,1.75);
#12738=CYLINDRICAL_SURFACE('',#15176,1.75);
#12739=CYLINDRICAL_SURFACE('',#15179,1.75);
#12740=CYLINDRICAL_SURFACE('',#15182,1.75);
#12741=CYLINDRICAL_SURFACE('',#15185,1.75);
#12742=CYLINDRICAL_SURFACE('',#15188,1.75);
#12743=CYLINDRICAL_SURFACE('',#15191,1.75);
#12744=CYLINDRICAL_SURFACE('',#15194,1.75);
#12745=CYLINDRICAL_SURFACE('',#15197,1.75);
#12746=CYLINDRICAL_SURFACE('',#15200,1.75);
#12747=CYLINDRICAL_SURFACE('',#15203,1.75);
#12748=CYLINDRICAL_SURFACE('',#15206,1.75);
#12749=CYLINDRICAL_SURFACE('',#15209,1.75);
#12750=CYLINDRICAL_SURFACE('',#15212,1.75);
#12751=CYLINDRICAL_SURFACE('',#15215,1.75);
#12752=CYLINDRICAL_SURFACE('',#15220,1.75);
#12753=CYLINDRICAL_SURFACE('',#15223,0.165);
#12754=CYLINDRICAL_SURFACE('',#15240,1.2);
#12755=CYLINDRICAL_SURFACE('',#15241,1.);
#12756=CYLINDRICAL_SURFACE('',#15243,1.);
#12757=CYLINDRICAL_SURFACE('',#15248,1.005);
#12758=CYLINDRICAL_SURFACE('',#15251,1.2);
#12759=CYLINDRICAL_SURFACE('',#15257,1.005);
#12760=CYLINDRICAL_SURFACE('',#15260,1.2);
#12761=CYLINDRICAL_SURFACE('',#15266,0.165);
#12762=CYLINDRICAL_SURFACE('',#15267,1.005);
#12763=CYLINDRICAL_SURFACE('',#15270,1.5);
#12764=CYLINDRICAL_SURFACE('',#15283,0.225);
#12765=CYLINDRICAL_SURFACE('',#15286,1.3);
#12766=CYLINDRICAL_SURFACE('',#15305,0.1954);
#12767=CYLINDRICAL_SURFACE('',#15352,1.);
#12768=CYLINDRICAL_SURFACE('',#15354,2.);
#12769=CYLINDRICAL_SURFACE('',#15359,3.75);
#12770=CYLINDRICAL_SURFACE('',#15362,3.75);
#12771=CYLINDRICAL_SURFACE('',#15365,3.75);
#12772=CYLINDRICAL_SURFACE('',#15368,3.75);
#12773=CYLINDRICAL_SURFACE('',#15371,3.75);
#12774=CYLINDRICAL_SURFACE('',#15374,3.75);
#12775=CYLINDRICAL_SURFACE('',#15377,3.75);
#12776=CYLINDRICAL_SURFACE('',#15380,3.75);
#12777=CYLINDRICAL_SURFACE('',#15383,3.75);
#12778=CYLINDRICAL_SURFACE('',#15386,3.75);
#12779=CYLINDRICAL_SURFACE('',#15389,3.75);
#12780=CYLINDRICAL_SURFACE('',#15392,3.75);
#12781=CYLINDRICAL_SURFACE('',#15395,3.75);
#12782=CYLINDRICAL_SURFACE('',#15398,3.75);
#12783=CYLINDRICAL_SURFACE('',#15401,3.75);
#12784=CYLINDRICAL_SURFACE('',#15404,3.75);
#12785=CYLINDRICAL_SURFACE('',#15407,3.75);
#12786=CYLINDRICAL_SURFACE('',#15410,3.75);
#12787=CYLINDRICAL_SURFACE('',#15413,3.75);
#12788=CYLINDRICAL_SURFACE('',#15416,3.75);
#12789=CYLINDRICAL_SURFACE('',#15419,3.75);
#12790=CYLINDRICAL_SURFACE('',#15422,3.75);
#12791=CYLINDRICAL_SURFACE('',#15425,3.75);
#12792=CYLINDRICAL_SURFACE('',#15428,3.75);
#12793=CYLINDRICAL_SURFACE('',#15431,3.75);
#12794=CYLINDRICAL_SURFACE('',#15434,3.75);
#12795=CYLINDRICAL_SURFACE('',#15437,3.75);
#12796=CYLINDRICAL_SURFACE('',#15440,3.75);
#12797=CYLINDRICAL_SURFACE('',#15443,3.75);
#12798=CYLINDRICAL_SURFACE('',#15446,3.75);
#12799=CYLINDRICAL_SURFACE('',#15449,3.75);
#12800=CYLINDRICAL_SURFACE('',#15452,3.75);
#12801=CYLINDRICAL_SURFACE('',#15455,3.75);
#12802=CYLINDRICAL_SURFACE('',#15458,3.75);
#12803=CYLINDRICAL_SURFACE('',#15461,3.75);
#12804=CYLINDRICAL_SURFACE('',#15464,3.75);
#12805=CYLINDRICAL_SURFACE('',#15467,3.75);
#12806=CYLINDRICAL_SURFACE('',#15470,3.75);
#12807=CYLINDRICAL_SURFACE('',#15473,3.75);
#12808=CYLINDRICAL_SURFACE('',#15478,3.75);
#12809=CYLINDRICAL_SURFACE('',#15494,0.35);
#12810=CYLINDRICAL_SURFACE('',#15502,0.1954);
#12811=ADVANCED_FACE('',(#1694),#12585,.F.);
#12812=ADVANCED_FACE('',(#1695),#12586,.F.);
#12813=ADVANCED_FACE('',(#1696),#12587,.F.);
#12814=ADVANCED_FACE('',(#1697),#12588,.F.);
#12815=ADVANCED_FACE('',(#1698),#12589,.F.);
#12816=ADVANCED_FACE('',(#1699),#12590,.F.);
#12817=ADVANCED_FACE('',(#1700),#12591,.F.);
#12818=ADVANCED_FACE('',(#1701),#12592,.F.);
#12819=ADVANCED_FACE('',(#1702),#12593,.F.);
#12820=ADVANCED_FACE('',(#1703),#12594,.F.);
#12821=ADVANCED_FACE('',(#1704),#12595,.F.);
#12822=ADVANCED_FACE('',(#1705),#12596,.F.);
#12823=ADVANCED_FACE('',(#1706),#1330,.T.);
#12824=ADVANCED_FACE('',(#1707),#1331,.T.);
#12825=ADVANCED_FACE('',(#1708),#1332,.T.);
#12826=ADVANCED_FACE('',(#1709),#1333,.T.);
#12827=ADVANCED_FACE('',(#1710,#1143,#1144,#1145,#1146,#1147,#1148,#1149,
#1150,#1151,#1152,#1153,#1154),#1334,.T.);
#12828=ADVANCED_FACE('',(#1711,#1155,#1156,#1157,#1158,#1159,#1160,#1161,
#1162,#1163,#1164,#1165,#1166),#1335,.F.);
#12829=ADVANCED_FACE('',(#1712),#1336,.T.);
#12830=ADVANCED_FACE('',(#1713),#1337,.T.);
#12831=ADVANCED_FACE('',(#1714),#1338,.T.);
#12832=ADVANCED_FACE('',(#1715),#1339,.T.);
#12833=ADVANCED_FACE('',(#1716),#1340,.T.);
#12834=ADVANCED_FACE('',(#1717),#1341,.F.);
#12835=ADVANCED_FACE('',(#1718),#1342,.T.);
#12836=ADVANCED_FACE('',(#1719),#1343,.T.);
#12837=ADVANCED_FACE('',(#1720),#1344,.T.);
#12838=ADVANCED_FACE('',(#1721),#1345,.T.);
#12839=ADVANCED_FACE('',(#1722),#1346,.T.);
#12840=ADVANCED_FACE('',(#1723),#1347,.F.);
#12841=ADVANCED_FACE('',(#1724),#12597,.F.);
#12842=ADVANCED_FACE('',(#1725),#12598,.F.);
#12843=ADVANCED_FACE('',(#1726),#1348,.T.);
#12844=ADVANCED_FACE('',(#1727),#12599,.F.);
#12845=ADVANCED_FACE('',(#1728),#1349,.T.);
#12846=ADVANCED_FACE('',(#1729),#12600,.F.);
#12847=ADVANCED_FACE('',(#1730),#1350,.T.);
#12848=ADVANCED_FACE('',(#1731),#12601,.F.);
#12849=ADVANCED_FACE('',(#1732),#1351,.T.);
#12850=ADVANCED_FACE('',(#1733),#1352,.F.);
#12851=ADVANCED_FACE('',(#1734),#12602,.F.);
#12852=ADVANCED_FACE('',(#1735),#12603,.F.);
#12853=ADVANCED_FACE('',(#1736),#1353,.F.);
#12854=ADVANCED_FACE('',(#1737),#12604,.F.);
#12855=ADVANCED_FACE('',(#1738),#1354,.F.);
#12856=ADVANCED_FACE('',(#1739),#12605,.F.);
#12857=ADVANCED_FACE('',(#1740),#1355,.F.);
#12858=ADVANCED_FACE('',(#1741,#1167),#12606,.T.);
#12859=ADVANCED_FACE('',(#1742,#1168,#1169,#1170,#1171,#1172),#1356,.T.);
#12860=ADVANCED_FACE('',(#1743),#12607,.F.);
#12861=ADVANCED_FACE('',(#1744),#12608,.F.);
#12862=ADVANCED_FACE('',(#1745),#12609,.F.);
#12863=ADVANCED_FACE('',(#1746),#12610,.F.);
#12864=ADVANCED_FACE('',(#1747),#12611,.F.);
#12865=ADVANCED_FACE('',(#1748,#1173),#1357,.T.);
#12866=ADVANCED_FACE('',(#1749),#12612,.T.);
#12867=ADVANCED_FACE('',(#1750,#1174),#12613,.F.);
#12868=ADVANCED_FACE('',(#1751,#1175,#1176,#1177,#1178,#1179),#1358,.T.);
#12869=ADVANCED_FACE('',(#1752,#1180,#1181,#1182,#1183,#1184),#1359,.F.);
#12870=ADVANCED_FACE('',(#1753),#12614,.F.);
#12871=ADVANCED_FACE('',(#1754),#12615,.T.);
#12872=ADVANCED_FACE('',(#1755,#1185),#1360,.T.);
#12873=ADVANCED_FACE('',(#1756,#1186),#1361,.F.);
#12874=ADVANCED_FACE('',(#1757),#12616,.F.);
#12875=ADVANCED_FACE('',(#1758),#12617,.F.);
#12876=ADVANCED_FACE('',(#1759),#12618,.F.);
#12877=ADVANCED_FACE('',(#1760),#12619,.F.);
#12878=ADVANCED_FACE('',(#1761,#1187),#1362,.F.);
#12879=ADVANCED_FACE('',(#1762),#12620,.T.);
#12880=ADVANCED_FACE('',(#1763),#12621,.T.);
#12881=ADVANCED_FACE('',(#1764),#12622,.T.);
#12882=ADVANCED_FACE('',(#1765),#12623,.T.);
#12883=ADVANCED_FACE('',(#1766),#12624,.T.);
#12884=ADVANCED_FACE('',(#1767,#1188),#1363,.F.);
#12885=ADVANCED_FACE('',(#1768),#12625,.F.);
#12886=ADVANCED_FACE('',(#1769,#1189),#1364,.T.);
#12887=ADVANCED_FACE('',(#1770),#12626,.F.);
#12888=ADVANCED_FACE('',(#1771),#12627,.F.);
#12889=ADVANCED_FACE('',(#1772),#12628,.F.);
#12890=ADVANCED_FACE('',(#1773),#12629,.F.);
#12891=ADVANCED_FACE('',(#1774),#12630,.T.);
#12892=ADVANCED_FACE('',(#1775),#1365,.T.);
#12893=ADVANCED_FACE('',(#1776),#12631,.T.);
#12894=ADVANCED_FACE('',(#1777,#1190,#1191,#1192,#1193,#1194),#1366,.T.);
#12895=ADVANCED_FACE('',(#1778,#1195,#1196,#1197,#1198),#1367,.F.);
#12896=ADVANCED_FACE('',(#1779),#1368,.T.);
#12897=ADVANCED_FACE('',(#1780),#12632,.F.);
#12898=ADVANCED_FACE('',(#1781),#1369,.T.);
#12899=ADVANCED_FACE('',(#1782),#12633,.F.);
#12900=ADVANCED_FACE('',(#1783),#1370,.F.);
#12901=ADVANCED_FACE('',(#1784),#1371,.T.);
#12902=ADVANCED_FACE('',(#1785),#1372,.T.);
#12903=ADVANCED_FACE('',(#1786),#1373,.T.);
#12904=ADVANCED_FACE('',(#1787),#1374,.F.);
#12905=ADVANCED_FACE('',(#1788),#1375,.F.);
#12906=ADVANCED_FACE('',(#1789),#1376,.T.);
#12907=ADVANCED_FACE('',(#1790),#1377,.T.);
#12908=ADVANCED_FACE('',(#1791),#1378,.T.);
#12909=ADVANCED_FACE('',(#1792),#1379,.T.);
#12910=ADVANCED_FACE('',(#1793),#1380,.T.);
#12911=ADVANCED_FACE('',(#1794),#1381,.T.);
#12912=ADVANCED_FACE('',(#1795,#1199),#1382,.T.);
#12913=ADVANCED_FACE('',(#1796,#1200),#12634,.F.);
#12914=ADVANCED_FACE('',(#1797),#12635,.T.);
#12915=ADVANCED_FACE('',(#1798),#1383,.T.);
#12916=ADVANCED_FACE('',(#1799),#1384,.T.);
#12917=ADVANCED_FACE('',(#1800),#1385,.T.);
#12918=ADVANCED_FACE('',(#1801,#1201),#1386,.T.);
#12919=ADVANCED_FACE('',(#1802),#1387,.T.);
#12920=ADVANCED_FACE('',(#1803,#1202),#1388,.F.);
#12921=ADVANCED_FACE('',(#1804),#12636,.F.);
#12922=ADVANCED_FACE('',(#1805),#12637,.T.);
#12923=ADVANCED_FACE('',(#1806,#1203),#1389,.T.);
#12924=ADVANCED_FACE('',(#1807,#1204),#1390,.F.);
#12925=ADVANCED_FACE('',(#1808),#12638,.T.);
#12926=ADVANCED_FACE('',(#1809),#1391,.T.);
#12927=ADVANCED_FACE('',(#1810),#1392,.F.);
#12928=ADVANCED_FACE('',(#1811),#12639,.T.);
#12929=ADVANCED_FACE('',(#1812),#1393,.T.);
#12930=ADVANCED_FACE('',(#1813),#1394,.F.);
#12931=ADVANCED_FACE('',(#1814),#12640,.F.);
#12932=ADVANCED_FACE('',(#1815,#1205),#1395,.T.);
#12933=ADVANCED_FACE('',(#1816),#12641,.F.);
#12934=ADVANCED_FACE('',(#1817,#1206),#1396,.T.);
#12935=ADVANCED_FACE('',(#1818),#12642,.F.);
#12936=ADVANCED_FACE('',(#1819,#1207),#1397,.T.);
#12937=ADVANCED_FACE('',(#1820),#12643,.F.);
#12938=ADVANCED_FACE('',(#1821,#1208),#1398,.T.);
#12939=ADVANCED_FACE('',(#1822),#12644,.F.);
#12940=ADVANCED_FACE('',(#1823),#12645,.F.);
#12941=ADVANCED_FACE('',(#1824),#12646,.F.);
#12942=ADVANCED_FACE('',(#1825),#12647,.F.);
#12943=ADVANCED_FACE('',(#1826),#1399,.T.);
#12944=ADVANCED_FACE('',(#1827),#1400,.T.);
#12945=ADVANCED_FACE('',(#1828),#1401,.T.);
#12946=ADVANCED_FACE('',(#1829),#1402,.T.);
#12947=ADVANCED_FACE('',(#1830,#1209,#1210,#1211,#1212),#1403,.T.);
#12948=ADVANCED_FACE('',(#1831),#1404,.T.);
#12949=ADVANCED_FACE('',(#1832),#1405,.T.);
#12950=ADVANCED_FACE('',(#1833),#1406,.T.);
#12951=ADVANCED_FACE('',(#1834),#1407,.T.);
#12952=ADVANCED_FACE('',(#1835),#1408,.T.);
#12953=ADVANCED_FACE('',(#1836,#1213,#1214,#1215,#1216),#1409,.T.);
#12954=ADVANCED_FACE('',(#1837),#1410,.T.);
#12955=ADVANCED_FACE('',(#1838),#1411,.T.);
#12956=ADVANCED_FACE('',(#1839),#1412,.F.);
#12957=ADVANCED_FACE('',(#1840),#780,.F.);
#12958=ADVANCED_FACE('',(#1841),#12648,.T.);
#12959=ADVANCED_FACE('',(#1842),#12649,.F.);
#12960=ADVANCED_FACE('',(#1843),#759,.F.);
#12961=ADVANCED_FACE('',(#1844,#1217),#1413,.T.);
#12962=ADVANCED_FACE('',(#1845),#12650,.T.);
#12963=ADVANCED_FACE('',(#1846,#1218),#1414,.T.);
#12964=ADVANCED_FACE('',(#1847),#760,.F.);
#12965=ADVANCED_FACE('',(#1848),#781,.F.);
#12966=ADVANCED_FACE('',(#1849),#12651,.F.);
#12967=ADVANCED_FACE('',(#1850,#1219),#1415,.T.);
#12968=ADVANCED_FACE('',(#1851),#761,.T.);
#12969=ADVANCED_FACE('',(#1852),#12652,.T.);
#12970=ADVANCED_FACE('',(#1853),#762,.T.);
#12971=ADVANCED_FACE('',(#1854,#1220),#1416,.T.);
#12972=ADVANCED_FACE('',(#1855),#12653,.F.);
#12973=ADVANCED_FACE('',(#1856),#729,.T.);
#12974=ADVANCED_FACE('',(#1857),#730,.T.);
#12975=ADVANCED_FACE('',(#1858),#731,.T.);
#12976=ADVANCED_FACE('',(#1859),#732,.T.);
#12977=ADVANCED_FACE('',(#1860),#733,.T.);
#12978=ADVANCED_FACE('',(#1861),#734,.T.);
#12979=ADVANCED_FACE('',(#1862),#735,.T.);
#12980=ADVANCED_FACE('',(#1863),#736,.F.);
#12981=ADVANCED_FACE('',(#1864),#12654,.T.);
#12982=ADVANCED_FACE('',(#1865),#1417,.T.);
#12983=ADVANCED_FACE('',(#1866),#737,.F.);
#12984=ADVANCED_FACE('',(#1867),#1418,.T.);
#12985=ADVANCED_FACE('',(#1868),#738,.F.);
#12986=ADVANCED_FACE('',(#1869),#1419,.T.);
#12987=ADVANCED_FACE('',(#1870),#739,.F.);
#12988=ADVANCED_FACE('',(#1871),#1420,.T.);
#12989=ADVANCED_FACE('',(#1872),#740,.F.);
#12990=ADVANCED_FACE('',(#1873),#1421,.T.);
#12991=ADVANCED_FACE('',(#1874),#741,.F.);
#12992=ADVANCED_FACE('',(#1875),#12655,.F.);
#12993=ADVANCED_FACE('',(#1876),#1422,.T.);
#12994=ADVANCED_FACE('',(#1877),#742,.F.);
#12995=ADVANCED_FACE('',(#1878,#1221),#1423,.T.);
#12996=ADVANCED_FACE('',(#1879),#1424,.T.);
#12997=ADVANCED_FACE('',(#1880,#1222),#1425,.T.);
#12998=ADVANCED_FACE('',(#1881),#12656,.T.);
#12999=ADVANCED_FACE('',(#1882,#1223),#1426,.T.);
#13000=ADVANCED_FACE('',(#1883),#12657,.F.);
#13001=ADVANCED_FACE('',(#1884,#1224),#1427,.T.);
#13002=ADVANCED_FACE('',(#1885),#12658,.T.);
#13003=ADVANCED_FACE('',(#1886,#1225),#1428,.T.);
#13004=ADVANCED_FACE('',(#1887),#12659,.F.);
#13005=ADVANCED_FACE('',(#1888),#1429,.T.);
#13006=ADVANCED_FACE('',(#1889),#763,.T.);
#13007=ADVANCED_FACE('',(#1890),#12660,.T.);
#13008=ADVANCED_FACE('',(#1891),#764,.T.);
#13009=ADVANCED_FACE('',(#1892,#1226),#1430,.T.);
#13010=ADVANCED_FACE('',(#1893),#765,.T.);
#13011=ADVANCED_FACE('',(#1894),#12661,.T.);
#13012=ADVANCED_FACE('',(#1895),#766,.T.);
#13013=ADVANCED_FACE('',(#1896),#1431,.T.);
#13014=ADVANCED_FACE('',(#1897),#1432,.F.);
#13015=ADVANCED_FACE('',(#1898),#1433,.F.);
#13016=ADVANCED_FACE('',(#1899),#1434,.F.);
#13017=ADVANCED_FACE('',(#1900),#1435,.F.);
#13018=ADVANCED_FACE('',(#1901),#1436,.F.);
#13019=ADVANCED_FACE('',(#1902),#1437,.F.);
#13020=ADVANCED_FACE('',(#1903),#1438,.F.);
#13021=ADVANCED_FACE('',(#1904),#1439,.F.);
#13022=ADVANCED_FACE('',(#1905),#12662,.F.);
#13023=ADVANCED_FACE('',(#1906),#12663,.F.);
#13024=ADVANCED_FACE('',(#1907),#12664,.F.);
#13025=ADVANCED_FACE('',(#1908),#12665,.F.);
#13026=ADVANCED_FACE('',(#1909),#12666,.F.);
#13027=ADVANCED_FACE('',(#1910,#1227),#1440,.T.);
#13028=ADVANCED_FACE('',(#1911),#1441,.T.);
#13029=ADVANCED_FACE('',(#1912,#1228),#1442,.T.);
#13030=ADVANCED_FACE('',(#1913),#1443,.T.);
#13031=ADVANCED_FACE('',(#1914),#1444,.F.);
#13032=ADVANCED_FACE('',(#1915),#12667,.F.);
#13033=ADVANCED_FACE('',(#1916),#12668,.F.);
#13034=ADVANCED_FACE('',(#1917),#12669,.F.);
#13035=ADVANCED_FACE('',(#1918),#12670,.F.);
#13036=ADVANCED_FACE('',(#1919),#12671,.F.);
#13037=ADVANCED_FACE('',(#1920,#1229,#1230,#1231,#1232,#1233,#1234,#1235,
#1236),#1445,.T.);
#13038=ADVANCED_FACE('',(#1921),#1446,.T.);
#13039=ADVANCED_FACE('',(#1922),#1447,.T.);
#13040=ADVANCED_FACE('',(#1923),#1448,.T.);
#13041=ADVANCED_FACE('',(#1924),#1449,.T.);
#13042=ADVANCED_FACE('',(#1925),#1450,.T.);
#13043=ADVANCED_FACE('',(#1926,#1237,#1238,#1239,#1240,#1241,#1242,#1243,
#1244,#1245),#1451,.F.);
#13044=ADVANCED_FACE('',(#1927),#1452,.T.);
#13045=ADVANCED_FACE('',(#1928),#1453,.T.);
#13046=ADVANCED_FACE('',(#1929),#1454,.T.);
#13047=ADVANCED_FACE('',(#1930),#1455,.T.);
#13048=ADVANCED_FACE('',(#1931),#1456,.T.);
#13049=ADVANCED_FACE('',(#1932),#1457,.F.);
#13050=ADVANCED_FACE('',(#1933),#12672,.F.);
#13051=ADVANCED_FACE('',(#1934),#12673,.F.);
#13052=ADVANCED_FACE('',(#1935),#1458,.T.);
#13053=ADVANCED_FACE('',(#1936),#12674,.F.);
#13054=ADVANCED_FACE('',(#1937),#1459,.T.);
#13055=ADVANCED_FACE('',(#1938),#12675,.F.);
#13056=ADVANCED_FACE('',(#1939),#1460,.T.);
#13057=ADVANCED_FACE('',(#1940),#12676,.F.);
#13058=ADVANCED_FACE('',(#1941),#1461,.T.);
#13059=ADVANCED_FACE('',(#1942),#12677,.F.);
#13060=ADVANCED_FACE('',(#1943),#1462,.F.);
#13061=ADVANCED_FACE('',(#1944),#12678,.F.);
#13062=ADVANCED_FACE('',(#1945),#1463,.F.);
#13063=ADVANCED_FACE('',(#1946),#12679,.F.);
#13064=ADVANCED_FACE('',(#1947),#1464,.F.);
#13065=ADVANCED_FACE('',(#1948),#12680,.F.);
#13066=ADVANCED_FACE('',(#1949),#1465,.F.);
#13067=ADVANCED_FACE('',(#1950),#12681,.F.);
#13068=ADVANCED_FACE('',(#1951,#1246,#1247,#1248,#1249,#1250),#1466,.T.);
#13069=ADVANCED_FACE('',(#1952),#12682,.F.);
#13070=ADVANCED_FACE('',(#1953),#12683,.F.);
#13071=ADVANCED_FACE('',(#1954),#12684,.F.);
#13072=ADVANCED_FACE('',(#1955,#1251),#12685,.T.);
#13073=ADVANCED_FACE('',(#1956),#12686,.F.);
#13074=ADVANCED_FACE('',(#1957,#1252),#1467,.T.);
#13075=ADVANCED_FACE('',(#1958),#12687,.T.);
#13076=ADVANCED_FACE('',(#1959,#1253),#12688,.F.);
#13077=ADVANCED_FACE('',(#1960,#1254,#1255,#1256,#1257,#1258),#1468,.T.);
#13078=ADVANCED_FACE('',(#1961,#1259,#1260,#1261,#1262,#1263),#1469,.F.);
#13079=ADVANCED_FACE('',(#1962),#12689,.F.);
#13080=ADVANCED_FACE('',(#1963),#12690,.T.);
#13081=ADVANCED_FACE('',(#1964,#1264),#1470,.T.);
#13082=ADVANCED_FACE('',(#1965,#1265),#1471,.F.);
#13083=ADVANCED_FACE('',(#1966),#12691,.F.);
#13084=ADVANCED_FACE('',(#1967),#12692,.F.);
#13085=ADVANCED_FACE('',(#1968),#12693,.F.);
#13086=ADVANCED_FACE('',(#1969),#12694,.F.);
#13087=ADVANCED_FACE('',(#1970),#12695,.F.);
#13088=ADVANCED_FACE('',(#1971),#12696,.T.);
#13089=ADVANCED_FACE('',(#1972,#1266,#1267,#1268,#1269,#1270),#1472,.T.);
#13090=ADVANCED_FACE('',(#1973,#1271,#1272,#1273,#1274,#1275),#1473,.F.);
#13091=ADVANCED_FACE('',(#1974),#1474,.T.);
#13092=ADVANCED_FACE('',(#1975),#12697,.F.);
#13093=ADVANCED_FACE('',(#1976),#1475,.T.);
#13094=ADVANCED_FACE('',(#1977),#12698,.F.);
#13095=ADVANCED_FACE('',(#1978),#1476,.T.);
#13096=ADVANCED_FACE('',(#1979),#12699,.F.);
#13097=ADVANCED_FACE('',(#1980),#1477,.T.);
#13098=ADVANCED_FACE('',(#1981),#12700,.F.);
#13099=ADVANCED_FACE('',(#1982),#1478,.T.);
#13100=ADVANCED_FACE('',(#1983),#1479,.T.);
#13101=ADVANCED_FACE('',(#1984),#1480,.T.);
#13102=ADVANCED_FACE('',(#1985),#1481,.T.);
#13103=ADVANCED_FACE('',(#1986),#1482,.T.);
#13104=ADVANCED_FACE('',(#1987,#1276,#1277,#1278,#1279),#1483,.T.);
#13105=ADVANCED_FACE('',(#1988),#1484,.T.);
#13106=ADVANCED_FACE('',(#1989),#1485,.T.);
#13107=ADVANCED_FACE('',(#1990),#1486,.T.);
#13108=ADVANCED_FACE('',(#1991),#1487,.T.);
#13109=ADVANCED_FACE('',(#1992),#1488,.T.);
#13110=ADVANCED_FACE('',(#1993),#1489,.T.);
#13111=ADVANCED_FACE('',(#1994),#1490,.T.);
#13112=ADVANCED_FACE('',(#1995),#1491,.T.);
#13113=ADVANCED_FACE('',(#1996),#1492,.T.);
#13114=ADVANCED_FACE('',(#1997),#1493,.T.);
#13115=ADVANCED_FACE('',(#1998),#1494,.T.);
#13116=ADVANCED_FACE('',(#1999),#1495,.T.);
#13117=ADVANCED_FACE('',(#2000),#1496,.T.);
#13118=ADVANCED_FACE('',(#2001),#1497,.T.);
#13119=ADVANCED_FACE('',(#2002),#1498,.T.);
#13120=ADVANCED_FACE('',(#2003),#1499,.T.);
#13121=ADVANCED_FACE('',(#2004),#1500,.T.);
#13122=ADVANCED_FACE('',(#2005),#1501,.F.);
#13123=ADVANCED_FACE('',(#2006),#1502,.T.);
#13124=ADVANCED_FACE('',(#2007),#1503,.T.);
#13125=ADVANCED_FACE('',(#2008),#1504,.T.);
#13126=ADVANCED_FACE('',(#2009),#1505,.T.);
#13127=ADVANCED_FACE('',(#2010),#1506,.T.);
#13128=ADVANCED_FACE('',(#2011),#1507,.T.);
#13129=ADVANCED_FACE('',(#2012),#1508,.T.);
#13130=ADVANCED_FACE('',(#2013),#1509,.T.);
#13131=ADVANCED_FACE('',(#2014),#1510,.T.);
#13132=ADVANCED_FACE('',(#2015),#1511,.T.);
#13133=ADVANCED_FACE('',(#2016),#1512,.F.);
#13134=ADVANCED_FACE('',(#2017),#1513,.F.);
#13135=ADVANCED_FACE('',(#2018),#1514,.F.);
#13136=ADVANCED_FACE('',(#2019),#1515,.F.);
#13137=ADVANCED_FACE('',(#2020),#1516,.F.);
#13138=ADVANCED_FACE('',(#2021),#1517,.F.);
#13139=ADVANCED_FACE('',(#2022),#1518,.F.);
#13140=ADVANCED_FACE('',(#2023,#1280),#1519,.T.);
#13141=ADVANCED_FACE('',(#2024),#767,.T.);
#13142=ADVANCED_FACE('',(#2025),#12701,.T.);
#13143=ADVANCED_FACE('',(#2026),#768,.T.);
#13144=ADVANCED_FACE('',(#2027),#1520,.T.);
#13145=ADVANCED_FACE('',(#2028),#1521,.F.);
#13146=ADVANCED_FACE('',(#2029),#1522,.F.);
#13147=ADVANCED_FACE('',(#2030),#1523,.F.);
#13148=ADVANCED_FACE('',(#2031),#1524,.F.);
#13149=ADVANCED_FACE('',(#2032),#1525,.F.);
#13150=ADVANCED_FACE('',(#2033),#1526,.F.);
#13151=ADVANCED_FACE('',(#2034),#1527,.F.);
#13152=ADVANCED_FACE('',(#2035),#1528,.F.);
#13153=ADVANCED_FACE('',(#2036),#1529,.F.);
#13154=ADVANCED_FACE('',(#2037),#1530,.T.);
#13155=ADVANCED_FACE('',(#2038),#769,.T.);
#13156=ADVANCED_FACE('',(#2039),#12702,.T.);
#13157=ADVANCED_FACE('',(#2040),#770,.T.);
#13158=ADVANCED_FACE('',(#2041,#1281),#1531,.T.);
#13159=ADVANCED_FACE('',(#2042),#771,.T.);
#13160=ADVANCED_FACE('',(#2043),#12703,.T.);
#13161=ADVANCED_FACE('',(#2044),#782,.F.);
#13162=ADVANCED_FACE('',(#2045),#12704,.T.);
#13163=ADVANCED_FACE('',(#2046),#12705,.F.);
#13164=ADVANCED_FACE('',(#2047),#772,.F.);
#13165=ADVANCED_FACE('',(#2048,#1282),#1532,.T.);
#13166=ADVANCED_FACE('',(#2049),#12706,.T.);
#13167=ADVANCED_FACE('',(#2050,#1283),#1533,.T.);
#13168=ADVANCED_FACE('',(#2051),#773,.F.);
#13169=ADVANCED_FACE('',(#2052),#783,.F.);
#13170=ADVANCED_FACE('',(#2053),#12707,.F.);
#13171=ADVANCED_FACE('',(#2054,#1284),#1534,.T.);
#13172=ADVANCED_FACE('',(#2055),#774,.T.);
#13173=ADVANCED_FACE('',(#2056),#12708,.T.);
#13174=ADVANCED_FACE('',(#2057),#775,.T.);
#13175=ADVANCED_FACE('',(#2058,#1285),#1535,.T.);
#13176=ADVANCED_FACE('',(#2059),#12709,.F.);
#13177=ADVANCED_FACE('',(#2060),#743,.T.);
#13178=ADVANCED_FACE('',(#2061),#744,.T.);
#13179=ADVANCED_FACE('',(#2062),#745,.T.);
#13180=ADVANCED_FACE('',(#2063),#746,.T.);
#13181=ADVANCED_FACE('',(#2064),#747,.T.);
#13182=ADVANCED_FACE('',(#2065),#748,.T.);
#13183=ADVANCED_FACE('',(#2066),#749,.T.);
#13184=ADVANCED_FACE('',(#2067),#750,.T.);
#13185=ADVANCED_FACE('',(#2068),#751,.F.);
#13186=ADVANCED_FACE('',(#2069),#12710,.T.);
#13187=ADVANCED_FACE('',(#2070),#1536,.T.);
#13188=ADVANCED_FACE('',(#2071),#752,.F.);
#13189=ADVANCED_FACE('',(#2072),#1537,.T.);
#13190=ADVANCED_FACE('',(#2073),#753,.F.);
#13191=ADVANCED_FACE('',(#2074),#1538,.T.);
#13192=ADVANCED_FACE('',(#2075),#754,.F.);
#13193=ADVANCED_FACE('',(#2076),#1539,.T.);
#13194=ADVANCED_FACE('',(#2077),#755,.F.);
#13195=ADVANCED_FACE('',(#2078),#1540,.T.);
#13196=ADVANCED_FACE('',(#2079),#756,.F.);
#13197=ADVANCED_FACE('',(#2080),#1541,.T.);
#13198=ADVANCED_FACE('',(#2081),#757,.F.);
#13199=ADVANCED_FACE('',(#2082),#12711,.F.);
#13200=ADVANCED_FACE('',(#2083),#1542,.T.);
#13201=ADVANCED_FACE('',(#2084),#758,.F.);
#13202=ADVANCED_FACE('',(#2085,#1286),#1543,.T.);
#13203=ADVANCED_FACE('',(#2086),#1544,.T.);
#13204=ADVANCED_FACE('',(#2087,#1287),#1545,.T.);
#13205=ADVANCED_FACE('',(#2088),#12712,.T.);
#13206=ADVANCED_FACE('',(#2089,#1288),#1546,.T.);
#13207=ADVANCED_FACE('',(#2090),#12713,.F.);
#13208=ADVANCED_FACE('',(#2091,#1289),#1547,.T.);
#13209=ADVANCED_FACE('',(#2092),#12714,.T.);
#13210=ADVANCED_FACE('',(#2093,#1290),#1548,.T.);
#13211=ADVANCED_FACE('',(#2094),#12715,.F.);
#13212=ADVANCED_FACE('',(#2095),#12716,.F.);
#13213=ADVANCED_FACE('',(#2096),#1549,.T.);
#13214=ADVANCED_FACE('',(#2097),#1550,.F.);
#13215=ADVANCED_FACE('',(#2098),#1551,.T.);
#13216=ADVANCED_FACE('',(#2099),#1552,.F.);
#13217=ADVANCED_FACE('',(#2100),#1553,.F.);
#13218=ADVANCED_FACE('',(#2101),#1554,.F.);
#13219=ADVANCED_FACE('',(#2102,#1291),#1555,.T.);
#13220=ADVANCED_FACE('',(#2103,#1292),#1556,.F.);
#13221=ADVANCED_FACE('',(#2104),#12717,.T.);
#13222=ADVANCED_FACE('',(#2105),#12718,.T.);
#13223=ADVANCED_FACE('',(#2106,#1293),#12719,.T.);
#13224=ADVANCED_FACE('',(#2107,#1294),#1557,.T.);
#13225=ADVANCED_FACE('',(#2108),#1558,.F.);
#13226=ADVANCED_FACE('',(#2109),#12720,.F.);
#13227=ADVANCED_FACE('',(#2110),#12721,.T.);
#13228=ADVANCED_FACE('',(#2111,#1295),#1559,.T.);
#13229=ADVANCED_FACE('',(#2112,#1296),#1560,.F.);
#13230=ADVANCED_FACE('',(#2113),#12722,.F.);
#13231=ADVANCED_FACE('',(#2114),#12723,.T.);
#13232=ADVANCED_FACE('',(#2115,#1297),#1561,.T.);
#13233=ADVANCED_FACE('',(#2116,#1298),#1562,.F.);
#13234=ADVANCED_FACE('',(#2117),#12724,.F.);
#13235=ADVANCED_FACE('',(#2118),#12725,.T.);
#13236=ADVANCED_FACE('',(#2119,#1299),#1563,.T.);
#13237=ADVANCED_FACE('',(#2120,#1300),#1564,.F.);
#13238=ADVANCED_FACE('',(#2121),#1565,.T.);
#13239=ADVANCED_FACE('',(#2122),#1566,.F.);
#13240=ADVANCED_FACE('',(#2123),#12726,.F.);
#13241=ADVANCED_FACE('',(#2124),#1567,.T.);
#13242=ADVANCED_FACE('',(#2125,#1301),#12727,.F.);
#13243=ADVANCED_FACE('',(#2126,#1302,#1303),#12728,.T.);
#13244=ADVANCED_FACE('',(#2127,#1304),#1568,.T.);
#13245=ADVANCED_FACE('',(#2128,#1305),#1569,.F.);
#13246=ADVANCED_FACE('',(#2129),#1570,.T.);
#13247=ADVANCED_FACE('',(#2130),#1571,.T.);
#13248=ADVANCED_FACE('',(#2131),#1572,.T.);
#13249=ADVANCED_FACE('',(#2132),#1573,.T.);
#13250=ADVANCED_FACE('',(#2133),#1574,.T.);
#13251=ADVANCED_FACE('',(#2134),#1575,.F.);
#13252=ADVANCED_FACE('',(#2135),#12729,.F.);
#13253=ADVANCED_FACE('',(#2136),#12730,.T.);
#13254=ADVANCED_FACE('',(#2137,#1306),#1576,.T.);
#13255=ADVANCED_FACE('',(#2138,#1307),#1577,.F.);
#13256=ADVANCED_FACE('',(#2139),#1578,.F.);
#13257=ADVANCED_FACE('',(#2140),#1579,.F.);
#13258=ADVANCED_FACE('',(#2141),#1580,.F.);
#13259=ADVANCED_FACE('',(#2142,#1308),#1581,.F.);
#13260=ADVANCED_FACE('',(#2143),#12731,.F.);
#13261=ADVANCED_FACE('',(#2144),#12732,.T.);
#13262=ADVANCED_FACE('',(#2145,#1309),#1582,.T.);
#13263=ADVANCED_FACE('',(#2146),#11,.T.);
#13264=ADVANCED_FACE('',(#2147),#1583,.T.);
#13265=ADVANCED_FACE('',(#2148),#12,.T.);
#13266=ADVANCED_FACE('',(#2149),#12733,.T.);
#13267=ADVANCED_FACE('',(#2150),#13,.T.);
#13268=ADVANCED_FACE('',(#2151),#1584,.T.);
#13269=ADVANCED_FACE('',(#2152),#14,.T.);
#13270=ADVANCED_FACE('',(#2153),#12734,.T.);
#13271=ADVANCED_FACE('',(#2154),#15,.T.);
#13272=ADVANCED_FACE('',(#2155),#1585,.T.);
#13273=ADVANCED_FACE('',(#2156),#16,.T.);
#13274=ADVANCED_FACE('',(#2157),#12735,.T.);
#13275=ADVANCED_FACE('',(#2158),#17,.T.);
#13276=ADVANCED_FACE('',(#2159),#1586,.T.);
#13277=ADVANCED_FACE('',(#2160),#18,.T.);
#13278=ADVANCED_FACE('',(#2161),#12736,.T.);
#13279=ADVANCED_FACE('',(#2162),#19,.T.);
#13280=ADVANCED_FACE('',(#2163),#1587,.T.);
#13281=ADVANCED_FACE('',(#2164),#20,.T.);
#13282=ADVANCED_FACE('',(#2165),#12737,.T.);
#13283=ADVANCED_FACE('',(#2166),#21,.T.);
#13284=ADVANCED_FACE('',(#2167),#1588,.T.);
#13285=ADVANCED_FACE('',(#2168),#22,.T.);
#13286=ADVANCED_FACE('',(#2169),#12738,.T.);
#13287=ADVANCED_FACE('',(#2170),#23,.T.);
#13288=ADVANCED_FACE('',(#2171),#1589,.T.);
#13289=ADVANCED_FACE('',(#2172),#24,.T.);
#13290=ADVANCED_FACE('',(#2173),#12739,.T.);
#13291=ADVANCED_FACE('',(#2174),#25,.T.);
#13292=ADVANCED_FACE('',(#2175),#1590,.T.);
#13293=ADVANCED_FACE('',(#2176),#26,.T.);
#13294=ADVANCED_FACE('',(#2177),#12740,.T.);
#13295=ADVANCED_FACE('',(#2178),#27,.T.);
#13296=ADVANCED_FACE('',(#2179),#1591,.T.);
#13297=ADVANCED_FACE('',(#2180),#28,.T.);
#13298=ADVANCED_FACE('',(#2181),#12741,.T.);
#13299=ADVANCED_FACE('',(#2182),#29,.T.);
#13300=ADVANCED_FACE('',(#2183),#1592,.T.);
#13301=ADVANCED_FACE('',(#2184),#30,.T.);
#13302=ADVANCED_FACE('',(#2185),#12742,.T.);
#13303=ADVANCED_FACE('',(#2186),#31,.T.);
#13304=ADVANCED_FACE('',(#2187),#1593,.T.);
#13305=ADVANCED_FACE('',(#2188),#32,.T.);
#13306=ADVANCED_FACE('',(#2189),#12743,.T.);
#13307=ADVANCED_FACE('',(#2190),#33,.T.);
#13308=ADVANCED_FACE('',(#2191),#1594,.T.);
#13309=ADVANCED_FACE('',(#2192),#34,.T.);
#13310=ADVANCED_FACE('',(#2193),#12744,.T.);
#13311=ADVANCED_FACE('',(#2194),#35,.T.);
#13312=ADVANCED_FACE('',(#2195),#1595,.T.);
#13313=ADVANCED_FACE('',(#2196),#36,.T.);
#13314=ADVANCED_FACE('',(#2197),#12745,.T.);
#13315=ADVANCED_FACE('',(#2198),#37,.T.);
#13316=ADVANCED_FACE('',(#2199),#1596,.T.);
#13317=ADVANCED_FACE('',(#2200),#38,.T.);
#13318=ADVANCED_FACE('',(#2201),#12746,.T.);
#13319=ADVANCED_FACE('',(#2202),#39,.T.);
#13320=ADVANCED_FACE('',(#2203),#1597,.T.);
#13321=ADVANCED_FACE('',(#2204),#40,.T.);
#13322=ADVANCED_FACE('',(#2205),#12747,.T.);
#13323=ADVANCED_FACE('',(#2206),#41,.T.);
#13324=ADVANCED_FACE('',(#2207),#1598,.T.);
#13325=ADVANCED_FACE('',(#2208),#42,.T.);
#13326=ADVANCED_FACE('',(#2209),#12748,.T.);
#13327=ADVANCED_FACE('',(#2210),#43,.T.);
#13328=ADVANCED_FACE('',(#2211),#1599,.T.);
#13329=ADVANCED_FACE('',(#2212),#44,.T.);
#13330=ADVANCED_FACE('',(#2213),#12749,.T.);
#13331=ADVANCED_FACE('',(#2214),#45,.T.);
#13332=ADVANCED_FACE('',(#2215),#1600,.T.);
#13333=ADVANCED_FACE('',(#2216),#46,.T.);
#13334=ADVANCED_FACE('',(#2217),#12750,.T.);
#13335=ADVANCED_FACE('',(#2218),#47,.T.);
#13336=ADVANCED_FACE('',(#2219),#1601,.T.);
#13337=ADVANCED_FACE('',(#2220),#48,.T.);
#13338=ADVANCED_FACE('',(#2221),#12751,.T.);
#13339=ADVANCED_FACE('',(#2222),#49,.T.);
#13340=ADVANCED_FACE('',(#2223),#1602,.T.);
#13341=ADVANCED_FACE('',(#2224),#50,.T.);
#13342=ADVANCED_FACE('',(#2225,#1310),#1603,.T.);
#13343=ADVANCED_FACE('',(#2226),#12752,.T.);
#13344=ADVANCED_FACE('',(#2227),#12753,.F.);
#13345=ADVANCED_FACE('',(#2228),#1604,.T.);
#13346=ADVANCED_FACE('',(#2229),#1605,.F.);
#13347=ADVANCED_FACE('',(#2230),#1606,.T.);
#13348=ADVANCED_FACE('',(#2231),#1607,.F.);
#13349=ADVANCED_FACE('',(#2232),#1608,.F.);
#13350=ADVANCED_FACE('',(#2233),#1609,.F.);
#13351=ADVANCED_FACE('',(#2234,#1311),#1610,.T.);
#13352=ADVANCED_FACE('',(#2235,#1312),#1611,.F.);
#13353=ADVANCED_FACE('',(#2236),#12754,.T.);
#13354=ADVANCED_FACE('',(#2237),#12755,.T.);
#13355=ADVANCED_FACE('',(#2238,#1313),#12756,.T.);
#13356=ADVANCED_FACE('',(#2239,#1314),#1612,.T.);
#13357=ADVANCED_FACE('',(#2240),#1613,.F.);
#13358=ADVANCED_FACE('',(#2241),#12757,.F.);
#13359=ADVANCED_FACE('',(#2242),#12758,.T.);
#13360=ADVANCED_FACE('',(#2243,#1315),#1614,.T.);
#13361=ADVANCED_FACE('',(#2244,#1316),#1615,.F.);
#13362=ADVANCED_FACE('',(#2245),#12759,.F.);
#13363=ADVANCED_FACE('',(#2246),#12760,.T.);
#13364=ADVANCED_FACE('',(#2247,#1317),#1616,.T.);
#13365=ADVANCED_FACE('',(#2248,#1318),#1617,.F.);
#13366=ADVANCED_FACE('',(#2249),#12761,.F.);
#13367=ADVANCED_FACE('',(#2250,#1319),#12762,.F.);
#13368=ADVANCED_FACE('',(#2251,#1320),#12763,.T.);
#13369=ADVANCED_FACE('',(#2252,#1321),#1618,.T.);
#13370=ADVANCED_FACE('',(#2253,#1322),#1619,.F.);
#13371=ADVANCED_FACE('',(#2254),#1620,.T.);
#13372=ADVANCED_FACE('',(#2255),#1621,.T.);
#13373=ADVANCED_FACE('',(#2256),#1622,.T.);
#13374=ADVANCED_FACE('',(#2257),#1623,.T.);
#13375=ADVANCED_FACE('',(#2258),#1624,.T.);
#13376=ADVANCED_FACE('',(#2259),#1625,.F.);
#13377=ADVANCED_FACE('',(#2260),#12764,.F.);
#13378=ADVANCED_FACE('',(#2261),#12765,.T.);
#13379=ADVANCED_FACE('',(#2262,#1323),#1626,.T.);
#13380=ADVANCED_FACE('',(#2263,#1324),#1627,.F.);
#13381=ADVANCED_FACE('',(#2264),#1628,.F.);
#13382=ADVANCED_FACE('',(#2265),#1629,.F.);
#13383=ADVANCED_FACE('',(#2266),#1630,.F.);
#13384=ADVANCED_FACE('',(#2267),#1631,.F.);
#13385=ADVANCED_FACE('',(#2268),#1632,.F.);
#13386=ADVANCED_FACE('',(#2269),#1633,.F.);
#13387=ADVANCED_FACE('',(#2270),#1634,.F.);
#13388=ADVANCED_FACE('',(#2271),#1635,.F.);
#13389=ADVANCED_FACE('',(#2272,#1325),#1636,.T.);
#13390=ADVANCED_FACE('',(#2273),#776,.T.);
#13391=ADVANCED_FACE('',(#2274),#12766,.T.);
#13392=ADVANCED_FACE('',(#2275),#1637,.F.);
#13393=ADVANCED_FACE('',(#2276),#1638,.F.);
#13394=ADVANCED_FACE('',(#2277),#1639,.F.);
#13395=ADVANCED_FACE('',(#2278,#1326),#1640,.F.);
#13396=ADVANCED_FACE('',(#2279),#12767,.F.);
#13397=ADVANCED_FACE('',(#2280),#12768,.T.);
#13398=ADVANCED_FACE('',(#2281,#1327),#1641,.T.);
#13399=ADVANCED_FACE('',(#2282),#51,.T.);
#13400=ADVANCED_FACE('',(#2283),#52,.T.);
#13401=ADVANCED_FACE('',(#2284),#1642,.T.);
#13402=ADVANCED_FACE('',(#2285),#12769,.T.);
#13403=ADVANCED_FACE('',(#2286),#53,.T.);
#13404=ADVANCED_FACE('',(#2287),#54,.T.);
#13405=ADVANCED_FACE('',(#2288),#1643,.T.);
#13406=ADVANCED_FACE('',(#2289),#12770,.T.);
#13407=ADVANCED_FACE('',(#2290),#55,.T.);
#13408=ADVANCED_FACE('',(#2291),#56,.T.);
#13409=ADVANCED_FACE('',(#2292),#1644,.T.);
#13410=ADVANCED_FACE('',(#2293),#12771,.T.);
#13411=ADVANCED_FACE('',(#2294),#57,.T.);
#13412=ADVANCED_FACE('',(#2295),#58,.T.);
#13413=ADVANCED_FACE('',(#2296),#1645,.T.);
#13414=ADVANCED_FACE('',(#2297),#12772,.T.);
#13415=ADVANCED_FACE('',(#2298),#59,.T.);
#13416=ADVANCED_FACE('',(#2299),#60,.T.);
#13417=ADVANCED_FACE('',(#2300),#1646,.T.);
#13418=ADVANCED_FACE('',(#2301),#12773,.T.);
#13419=ADVANCED_FACE('',(#2302),#61,.T.);
#13420=ADVANCED_FACE('',(#2303),#62,.T.);
#13421=ADVANCED_FACE('',(#2304),#1647,.T.);
#13422=ADVANCED_FACE('',(#2305),#12774,.T.);
#13423=ADVANCED_FACE('',(#2306),#63,.T.);
#13424=ADVANCED_FACE('',(#2307),#64,.T.);
#13425=ADVANCED_FACE('',(#2308),#1648,.T.);
#13426=ADVANCED_FACE('',(#2309),#12775,.T.);
#13427=ADVANCED_FACE('',(#2310),#65,.T.);
#13428=ADVANCED_FACE('',(#2311),#66,.T.);
#13429=ADVANCED_FACE('',(#2312),#1649,.T.);
#13430=ADVANCED_FACE('',(#2313),#12776,.T.);
#13431=ADVANCED_FACE('',(#2314),#67,.T.);
#13432=ADVANCED_FACE('',(#2315),#68,.T.);
#13433=ADVANCED_FACE('',(#2316),#1650,.T.);
#13434=ADVANCED_FACE('',(#2317),#12777,.T.);
#13435=ADVANCED_FACE('',(#2318),#69,.T.);
#13436=ADVANCED_FACE('',(#2319),#70,.T.);
#13437=ADVANCED_FACE('',(#2320),#1651,.T.);
#13438=ADVANCED_FACE('',(#2321),#12778,.T.);
#13439=ADVANCED_FACE('',(#2322),#71,.T.);
#13440=ADVANCED_FACE('',(#2323),#72,.T.);
#13441=ADVANCED_FACE('',(#2324),#1652,.T.);
#13442=ADVANCED_FACE('',(#2325),#12779,.T.);
#13443=ADVANCED_FACE('',(#2326),#73,.T.);
#13444=ADVANCED_FACE('',(#2327),#74,.T.);
#13445=ADVANCED_FACE('',(#2328),#1653,.T.);
#13446=ADVANCED_FACE('',(#2329),#12780,.T.);
#13447=ADVANCED_FACE('',(#2330),#75,.T.);
#13448=ADVANCED_FACE('',(#2331),#76,.T.);
#13449=ADVANCED_FACE('',(#2332),#1654,.T.);
#13450=ADVANCED_FACE('',(#2333),#12781,.T.);
#13451=ADVANCED_FACE('',(#2334),#77,.T.);
#13452=ADVANCED_FACE('',(#2335),#78,.T.);
#13453=ADVANCED_FACE('',(#2336),#1655,.T.);
#13454=ADVANCED_FACE('',(#2337),#12782,.T.);
#13455=ADVANCED_FACE('',(#2338),#79,.T.);
#13456=ADVANCED_FACE('',(#2339),#80,.T.);
#13457=ADVANCED_FACE('',(#2340),#1656,.T.);
#13458=ADVANCED_FACE('',(#2341),#12783,.T.);
#13459=ADVANCED_FACE('',(#2342),#81,.T.);
#13460=ADVANCED_FACE('',(#2343),#82,.T.);
#13461=ADVANCED_FACE('',(#2344),#1657,.T.);
#13462=ADVANCED_FACE('',(#2345),#12784,.T.);
#13463=ADVANCED_FACE('',(#2346),#83,.T.);
#13464=ADVANCED_FACE('',(#2347),#84,.T.);
#13465=ADVANCED_FACE('',(#2348),#1658,.T.);
#13466=ADVANCED_FACE('',(#2349),#12785,.T.);
#13467=ADVANCED_FACE('',(#2350),#85,.T.);
#13468=ADVANCED_FACE('',(#2351),#86,.T.);
#13469=ADVANCED_FACE('',(#2352),#1659,.T.);
#13470=ADVANCED_FACE('',(#2353),#12786,.T.);
#13471=ADVANCED_FACE('',(#2354),#87,.T.);
#13472=ADVANCED_FACE('',(#2355),#88,.T.);
#13473=ADVANCED_FACE('',(#2356),#1660,.T.);
#13474=ADVANCED_FACE('',(#2357),#12787,.T.);
#13475=ADVANCED_FACE('',(#2358),#89,.T.);
#13476=ADVANCED_FACE('',(#2359),#90,.T.);
#13477=ADVANCED_FACE('',(#2360),#1661,.T.);
#13478=ADVANCED_FACE('',(#2361),#12788,.T.);
#13479=ADVANCED_FACE('',(#2362),#91,.T.);
#13480=ADVANCED_FACE('',(#2363),#92,.T.);
#13481=ADVANCED_FACE('',(#2364),#1662,.T.);
#13482=ADVANCED_FACE('',(#2365),#12789,.T.);
#13483=ADVANCED_FACE('',(#2366),#93,.T.);
#13484=ADVANCED_FACE('',(#2367),#94,.T.);
#13485=ADVANCED_FACE('',(#2368),#1663,.T.);
#13486=ADVANCED_FACE('',(#2369),#12790,.T.);
#13487=ADVANCED_FACE('',(#2370),#95,.T.);
#13488=ADVANCED_FACE('',(#2371),#96,.T.);
#13489=ADVANCED_FACE('',(#2372),#1664,.T.);
#13490=ADVANCED_FACE('',(#2373),#12791,.T.);
#13491=ADVANCED_FACE('',(#2374),#97,.T.);
#13492=ADVANCED_FACE('',(#2375),#98,.T.);
#13493=ADVANCED_FACE('',(#2376),#1665,.T.);
#13494=ADVANCED_FACE('',(#2377),#12792,.T.);
#13495=ADVANCED_FACE('',(#2378),#99,.T.);
#13496=ADVANCED_FACE('',(#2379),#100,.T.);
#13497=ADVANCED_FACE('',(#2380),#1666,.T.);
#13498=ADVANCED_FACE('',(#2381),#12793,.T.);
#13499=ADVANCED_FACE('',(#2382),#101,.T.);
#13500=ADVANCED_FACE('',(#2383),#102,.T.);
#13501=ADVANCED_FACE('',(#2384),#1667,.T.);
#13502=ADVANCED_FACE('',(#2385),#12794,.T.);
#13503=ADVANCED_FACE('',(#2386),#103,.T.);
#13504=ADVANCED_FACE('',(#2387),#104,.T.);
#13505=ADVANCED_FACE('',(#2388),#1668,.T.);
#13506=ADVANCED_FACE('',(#2389),#12795,.T.);
#13507=ADVANCED_FACE('',(#2390),#105,.T.);
#13508=ADVANCED_FACE('',(#2391),#106,.T.);
#13509=ADVANCED_FACE('',(#2392),#1669,.T.);
#13510=ADVANCED_FACE('',(#2393),#12796,.T.);
#13511=ADVANCED_FACE('',(#2394),#107,.T.);
#13512=ADVANCED_FACE('',(#2395),#108,.T.);
#13513=ADVANCED_FACE('',(#2396),#1670,.T.);
#13514=ADVANCED_FACE('',(#2397),#12797,.T.);
#13515=ADVANCED_FACE('',(#2398),#109,.T.);
#13516=ADVANCED_FACE('',(#2399),#110,.T.);
#13517=ADVANCED_FACE('',(#2400),#1671,.T.);
#13518=ADVANCED_FACE('',(#2401),#12798,.T.);
#13519=ADVANCED_FACE('',(#2402),#111,.T.);
#13520=ADVANCED_FACE('',(#2403),#112,.T.);
#13521=ADVANCED_FACE('',(#2404),#1672,.T.);
#13522=ADVANCED_FACE('',(#2405),#12799,.T.);
#13523=ADVANCED_FACE('',(#2406),#113,.T.);
#13524=ADVANCED_FACE('',(#2407),#114,.T.);
#13525=ADVANCED_FACE('',(#2408),#1673,.T.);
#13526=ADVANCED_FACE('',(#2409),#12800,.T.);
#13527=ADVANCED_FACE('',(#2410),#115,.T.);
#13528=ADVANCED_FACE('',(#2411),#116,.T.);
#13529=ADVANCED_FACE('',(#2412),#1674,.T.);
#13530=ADVANCED_FACE('',(#2413),#12801,.T.);
#13531=ADVANCED_FACE('',(#2414),#117,.T.);
#13532=ADVANCED_FACE('',(#2415),#118,.T.);
#13533=ADVANCED_FACE('',(#2416),#1675,.T.);
#13534=ADVANCED_FACE('',(#2417),#12802,.T.);
#13535=ADVANCED_FACE('',(#2418),#119,.T.);
#13536=ADVANCED_FACE('',(#2419),#120,.T.);
#13537=ADVANCED_FACE('',(#2420),#1676,.T.);
#13538=ADVANCED_FACE('',(#2421),#12803,.T.);
#13539=ADVANCED_FACE('',(#2422),#121,.T.);
#13540=ADVANCED_FACE('',(#2423),#122,.T.);
#13541=ADVANCED_FACE('',(#2424),#1677,.T.);
#13542=ADVANCED_FACE('',(#2425),#12804,.T.);
#13543=ADVANCED_FACE('',(#2426),#123,.T.);
#13544=ADVANCED_FACE('',(#2427),#124,.T.);
#13545=ADVANCED_FACE('',(#2428),#1678,.T.);
#13546=ADVANCED_FACE('',(#2429),#12805,.T.);
#13547=ADVANCED_FACE('',(#2430),#125,.T.);
#13548=ADVANCED_FACE('',(#2431),#126,.T.);
#13549=ADVANCED_FACE('',(#2432),#1679,.T.);
#13550=ADVANCED_FACE('',(#2433),#12806,.T.);
#13551=ADVANCED_FACE('',(#2434),#127,.T.);
#13552=ADVANCED_FACE('',(#2435),#1680,.T.);
#13553=ADVANCED_FACE('',(#2436),#128,.T.);
#13554=ADVANCED_FACE('',(#2437),#12807,.T.);
#13555=ADVANCED_FACE('',(#2438),#129,.T.);
#13556=ADVANCED_FACE('',(#2439),#130,.T.);
#13557=ADVANCED_FACE('',(#2440),#1681,.T.);
#13558=ADVANCED_FACE('',(#2441,#1328),#1682,.T.);
#13559=ADVANCED_FACE('',(#2442),#12808,.T.);
#13560=ADVANCED_FACE('',(#2443),#1683,.F.);
#13561=ADVANCED_FACE('',(#2444),#1684,.F.);
#13562=ADVANCED_FACE('',(#2445),#1685,.F.);
#13563=ADVANCED_FACE('',(#2446),#1686,.F.);
#13564=ADVANCED_FACE('',(#2447),#1687,.F.);
#13565=ADVANCED_FACE('',(#2448),#1688,.F.);
#13566=ADVANCED_FACE('',(#2449),#1689,.F.);
#13567=ADVANCED_FACE('',(#2450),#1690,.F.);
#13568=ADVANCED_FACE('',(#2451),#1691,.F.);
#13569=ADVANCED_FACE('',(#2452),#1692,.T.);
#13570=ADVANCED_FACE('',(#2453),#777,.T.);
#13571=ADVANCED_FACE('',(#2454),#12809,.T.);
#13572=ADVANCED_FACE('',(#2455),#778,.T.);
#13573=ADVANCED_FACE('',(#2456,#1329),#1693,.T.);
#13574=ADVANCED_FACE('',(#2457),#779,.T.);
#13575=ADVANCED_FACE('',(#2458),#12810,.T.);
#13576=CLOSED_SHELL('',(#12811,#12812,#12813,#12814,#12815,#12816,#12817,
#12818,#12819,#12820,#12821,#12822,#12823,#12824,#12825,#12826,#12827,#12828));
#13577=CLOSED_SHELL('',(#12829,#12830,#12831,#12832,#12833,#12834));
#13578=CLOSED_SHELL('',(#12835,#12836,#12837,#12838,#12839,#12840));
#13579=CLOSED_SHELL('',(#12841,#12842,#12843,#12844,#12845,#12846,#12847,
#12848,#12849,#12850,#12851,#12852,#12853,#12854,#12855,#12856,#12857,#12858,
#12859,#12860,#12861,#12862,#12863,#12864,#12865,#12866,#12867,#12868,#12869));
#13580=CLOSED_SHELL('',(#12870,#12871,#12872,#12873));
#13581=CLOSED_SHELL('',(#12874,#12875,#12876,#12877,#12878,#12879,#12880,
#12881,#12882,#12883,#12884,#12885,#12886));
#13582=CLOSED_SHELL('',(#12887,#12888,#12889,#12890,#12891,#12892,#12893,
#12894,#12895));
#13583=CLOSED_SHELL('',(#12896,#12897,#12898,#12899,#12900,#12901,#12902,
#12903,#12904,#12905,#12906,#12907,#12908,#12909,#12910,#12911,#12912,#12913,
#12914,#12915,#12916,#12917,#12918,#12919,#12920));
#13584=CLOSED_SHELL('',(#12921,#12922,#12923,#12924));
#13585=CLOSED_SHELL('',(#12925,#12926,#12927));
#13586=CLOSED_SHELL('',(#12928,#12929,#12930));
#13587=CLOSED_SHELL('',(#12931,#12932,#12933,#12934,#12935,#12936,#12937,
#12938,#12939,#12940,#12941,#12942,#12943,#12944,#12945,#12946,#12947,#12948,
#12949,#12950,#12951,#12952,#12953,#12954,#12955,#12956));
#13588=CLOSED_SHELL('',(#12957,#12958,#12959,#12960,#12961,#12962,#12963,
#12964));
#13589=CLOSED_SHELL('',(#12965,#12966,#12967,#12968,#12969,#12970,#12971,
#12972));
#13590=CLOSED_SHELL('',(#12973));
#13591=CLOSED_SHELL('',(#12974));
#13592=CLOSED_SHELL('',(#12975));
#13593=CLOSED_SHELL('',(#12976));
#13594=CLOSED_SHELL('',(#12977));
#13595=CLOSED_SHELL('',(#12978));
#13596=CLOSED_SHELL('',(#12979));
#13597=CLOSED_SHELL('',(#12980,#12981,#12982,#12983,#12984,#12985,#12986,
#12987,#12988,#12989,#12990,#12991,#12992,#12993,#12994,#12995,#12996));
#13598=CLOSED_SHELL('',(#12997,#12998,#12999,#13000));
#13599=CLOSED_SHELL('',(#13001,#13002,#13003,#13004));
#13600=CLOSED_SHELL('',(#13005,#13006,#13007,#13008,#13009,#13010,#13011,
#13012,#13013));
#13601=CLOSED_SHELL('',(#13014,#13015,#13016,#13017,#13018,#13019,#13020,
#13021));
#13602=CLOSED_SHELL('',(#13022,#13023,#13024,#13025,#13026,#13027,#13028,
#13029,#13030,#13031,#13032,#13033,#13034,#13035,#13036,#13037,#13038,#13039,
#13040,#13041,#13042,#13043));
#13603=CLOSED_SHELL('',(#13044,#13045,#13046,#13047,#13048,#13049));
#13604=CLOSED_SHELL('',(#13050,#13051,#13052,#13053,#13054,#13055,#13056,
#13057,#13058,#13059,#13060,#13061,#13062,#13063,#13064,#13065,#13066,#13067,
#13068,#13069,#13070,#13071,#13072,#13073,#13074,#13075,#13076,#13077,#13078));
#13605=CLOSED_SHELL('',(#13079,#13080,#13081,#13082));
#13606=CLOSED_SHELL('',(#13083,#13084,#13085,#13086,#13087,#13088,#13089,
#13090));
#13607=CLOSED_SHELL('',(#13091,#13092,#13093,#13094,#13095,#13096,#13097,
#13098,#13099,#13100,#13101,#13102,#13103,#13104,#13105,#13106,#13107,#13108,
#13109,#13110,#13111,#13112));
#13608=CLOSED_SHELL('',(#13113,#13114,#13115,#13116,#13117,#13118,#13119,
#13120,#13121,#13122));
#13609=CLOSED_SHELL('',(#13123,#13124,#13125,#13126,#13127,#13128,#13129,
#13130,#13131,#13132));
#13610=CLOSED_SHELL('',(#13133,#13134,#13135,#13136,#13137,#13138,#13139,
#13140,#13141,#13142,#13143,#13144));
#13611=CLOSED_SHELL('',(#13145,#13146,#13147,#13148,#13149,#13150,#13151,
#13152));
#13612=CLOSED_SHELL('',(#13153,#13154,#13155,#13156,#13157,#13158,#13159,
#13160));
#13613=CLOSED_SHELL('',(#13161,#13162,#13163,#13164,#13165,#13166,#13167,
#13168));
#13614=CLOSED_SHELL('',(#13169,#13170,#13171,#13172,#13173,#13174,#13175,
#13176));
#13615=CLOSED_SHELL('',(#13177));
#13616=CLOSED_SHELL('',(#13178));
#13617=CLOSED_SHELL('',(#13179));
#13618=CLOSED_SHELL('',(#13180));
#13619=CLOSED_SHELL('',(#13181));
#13620=CLOSED_SHELL('',(#13182));
#13621=CLOSED_SHELL('',(#13183));
#13622=CLOSED_SHELL('',(#13184));
#13623=CLOSED_SHELL('',(#13185,#13186,#13187,#13188,#13189,#13190,#13191,
#13192,#13193,#13194,#13195,#13196,#13197,#13198,#13199,#13200,#13201,#13202,
#13203));
#13624=CLOSED_SHELL('',(#13204,#13205,#13206,#13207));
#13625=CLOSED_SHELL('',(#13208,#13209,#13210,#13211));
#13626=CLOSED_SHELL('',(#13212,#13213,#13214,#13215,#13216,#13217,#13218,
#13219,#13220,#13221,#13222,#13223,#13224,#13225));
#13627=CLOSED_SHELL('',(#13226,#13227,#13228,#13229));
#13628=CLOSED_SHELL('',(#13230,#13231,#13232,#13233));
#13629=CLOSED_SHELL('',(#13234,#13235,#13236,#13237));
#13630=CLOSED_SHELL('',(#13238,#13239,#13240,#13241,#13242,#13243,#13244,
#13245));
#13631=CLOSED_SHELL('',(#13246,#13247,#13248,#13249,#13250,#13251));
#13632=CLOSED_SHELL('',(#13252,#13253,#13254,#13255));
#13633=CLOSED_SHELL('',(#13256,#13257,#13258,#13259,#13260,#13261,#13262,
#13263,#13264,#13265,#13266,#13267,#13268,#13269,#13270,#13271,#13272,#13273,
#13274,#13275,#13276,#13277,#13278,#13279,#13280,#13281,#13282,#13283,#13284,
#13285,#13286,#13287,#13288,#13289,#13290,#13291,#13292,#13293,#13294,#13295,
#13296,#13297,#13298,#13299,#13300,#13301,#13302,#13303,#13304,#13305,#13306,
#13307,#13308,#13309,#13310,#13311,#13312,#13313,#13314,#13315,#13316,#13317,
#13318,#13319,#13320,#13321,#13322,#13323,#13324,#13325,#13326,#13327,#13328,
#13329,#13330,#13331,#13332,#13333,#13334,#13335,#13336,#13337,#13338,#13339,
#13340,#13341,#13342,#13343));
#13634=CLOSED_SHELL('',(#13344,#13345,#13346,#13347,#13348,#13349,#13350,
#13351,#13352,#13353,#13354,#13355,#13356,#13357));
#13635=CLOSED_SHELL('',(#13358,#13359,#13360,#13361));
#13636=CLOSED_SHELL('',(#13362,#13363,#13364,#13365));
#13637=CLOSED_SHELL('',(#13366,#13367,#13368,#13369,#13370));
#13638=CLOSED_SHELL('',(#13371,#13372,#13373,#13374,#13375,#13376));
#13639=CLOSED_SHELL('',(#13377,#13378,#13379,#13380));
#13640=CLOSED_SHELL('',(#13381,#13382,#13383,#13384,#13385,#13386,#13387,
#13388,#13389,#13390,#13391));
#13641=CLOSED_SHELL('',(#13392,#13393,#13394,#13395,#13396,#13397,#13398,
#13399,#13400,#13401,#13402,#13403,#13404,#13405,#13406,#13407,#13408,#13409,
#13410,#13411,#13412,#13413,#13414,#13415,#13416,#13417,#13418,#13419,#13420,
#13421,#13422,#13423,#13424,#13425,#13426,#13427,#13428,#13429,#13430,#13431,
#13432,#13433,#13434,#13435,#13436,#13437,#13438,#13439,#13440,#13441,#13442,
#13443,#13444,#13445,#13446,#13447,#13448,#13449,#13450,#13451,#13452,#13453,
#13454,#13455,#13456,#13457,#13458,#13459,#13460,#13461,#13462,#13463,#13464,
#13465,#13466,#13467,#13468,#13469,#13470,#13471,#13472,#13473,#13474,#13475,
#13476,#13477,#13478,#13479,#13480,#13481,#13482,#13483,#13484,#13485,#13486,
#13487,#13488,#13489,#13490,#13491,#13492,#13493,#13494,#13495,#13496,#13497,
#13498,#13499,#13500,#13501,#13502,#13503,#13504,#13505,#13506,#13507,#13508,
#13509,#13510,#13511,#13512,#13513,#13514,#13515,#13516,#13517,#13518,#13519,
#13520,#13521,#13522,#13523,#13524,#13525,#13526,#13527,#13528,#13529,#13530,
#13531,#13532,#13533,#13534,#13535,#13536,#13537,#13538,#13539,#13540,#13541,
#13542,#13543,#13544,#13545,#13546,#13547,#13548,#13549,#13550,#13551,#13552,
#13553,#13554,#13555,#13556,#13557,#13558,#13559));
#13642=CLOSED_SHELL('',(#13560,#13561,#13562,#13563,#13564,#13565,#13566,
#13567));
#13643=CLOSED_SHELL('',(#13568,#13569,#13570,#13571,#13572,#13573,#13574,
#13575));
#13644=DERIVED_UNIT_ELEMENT(#13744,1.);
#13645=DERIVED_UNIT_ELEMENT(#57902,-3.);
#13646=DERIVED_UNIT_ELEMENT(#13744,1.);
#13647=DERIVED_UNIT_ELEMENT(#57902,-3.);
#13648=DERIVED_UNIT_ELEMENT(#13744,1.);
#13649=DERIVED_UNIT_ELEMENT(#57902,-3.);
#13650=DERIVED_UNIT_ELEMENT(#13744,1.);
#13651=DERIVED_UNIT_ELEMENT(#57902,-3.);
#13652=DERIVED_UNIT_ELEMENT(#13744,1.);
#13653=DERIVED_UNIT_ELEMENT(#57902,-3.);
#13654=DERIVED_UNIT_ELEMENT(#13744,1.);
#13655=DERIVED_UNIT_ELEMENT(#57902,-3.);
#13656=DERIVED_UNIT_ELEMENT(#13744,1.);
#13657=DERIVED_UNIT_ELEMENT(#57902,-3.);
#13658=DERIVED_UNIT_ELEMENT(#13744,1.);
#13659=DERIVED_UNIT_ELEMENT(#57902,-3.);
#13660=DERIVED_UNIT_ELEMENT(#13744,1.);
#13661=DERIVED_UNIT_ELEMENT(#57902,-3.);
#13662=DERIVED_UNIT_ELEMENT(#13744,1.);
#13663=DERIVED_UNIT_ELEMENT(#57902,-3.);
#13664=DERIVED_UNIT_ELEMENT(#13744,1.);
#13665=DERIVED_UNIT_ELEMENT(#57902,-3.);
#13666=DERIVED_UNIT_ELEMENT(#13744,1.);
#13667=DERIVED_UNIT_ELEMENT(#57902,-3.);
#13668=DERIVED_UNIT_ELEMENT(#13744,1.);
#13669=DERIVED_UNIT_ELEMENT(#57902,-3.);
#13670=DERIVED_UNIT_ELEMENT(#13744,1.);
#13671=DERIVED_UNIT_ELEMENT(#57902,-3.);
#13672=DERIVED_UNIT_ELEMENT(#13744,1.);
#13673=DERIVED_UNIT_ELEMENT(#57902,-3.);
#13674=DERIVED_UNIT_ELEMENT(#13744,1.);
#13675=DERIVED_UNIT_ELEMENT(#57902,-3.);
#13676=DERIVED_UNIT_ELEMENT(#13744,1.);
#13677=DERIVED_UNIT_ELEMENT(#57902,-3.);
#13678=DERIVED_UNIT_ELEMENT(#13744,1.);
#13679=DERIVED_UNIT_ELEMENT(#57902,-3.);
#13680=DERIVED_UNIT_ELEMENT(#13744,1.);
#13681=DERIVED_UNIT_ELEMENT(#57902,-3.);
#13682=DERIVED_UNIT_ELEMENT(#13744,1.);
#13683=DERIVED_UNIT_ELEMENT(#57902,-3.);
#13684=DERIVED_UNIT_ELEMENT(#13744,1.);
#13685=DERIVED_UNIT_ELEMENT(#57902,-3.);
#13686=DERIVED_UNIT_ELEMENT(#13744,1.);
#13687=DERIVED_UNIT_ELEMENT(#57902,-3.);
#13688=DERIVED_UNIT_ELEMENT(#13744,1.);
#13689=DERIVED_UNIT_ELEMENT(#57902,-3.);
#13690=DERIVED_UNIT_ELEMENT(#13744,1.);
#13691=DERIVED_UNIT_ELEMENT(#57902,-3.);
#13692=DERIVED_UNIT_ELEMENT(#13744,1.);
#13693=DERIVED_UNIT_ELEMENT(#57902,-3.);
#13694=DERIVED_UNIT_ELEMENT(#13744,1.);
#13695=DERIVED_UNIT_ELEMENT(#57902,-3.);
#13696=DERIVED_UNIT_ELEMENT(#13744,1.);
#13697=DERIVED_UNIT_ELEMENT(#57902,-3.);
#13698=DERIVED_UNIT_ELEMENT(#13744,1.);
#13699=DERIVED_UNIT_ELEMENT(#57902,-3.);
#13700=DERIVED_UNIT_ELEMENT(#13744,1.);
#13701=DERIVED_UNIT_ELEMENT(#57902,-3.);
#13702=DERIVED_UNIT_ELEMENT(#13744,1.);
#13703=DERIVED_UNIT_ELEMENT(#57902,-3.);
#13704=DERIVED_UNIT_ELEMENT(#13744,1.);
#13705=DERIVED_UNIT_ELEMENT(#57902,-3.);
#13706=DERIVED_UNIT_ELEMENT(#13744,1.);
#13707=DERIVED_UNIT_ELEMENT(#57902,-3.);
#13708=DERIVED_UNIT_ELEMENT(#13744,1.);
#13709=DERIVED_UNIT_ELEMENT(#57902,-3.);
#13710=DERIVED_UNIT_ELEMENT(#13744,1.);
#13711=DERIVED_UNIT_ELEMENT(#57902,-3.);
#13712=DERIVED_UNIT_ELEMENT(#13744,1.);
#13713=DERIVED_UNIT_ELEMENT(#57902,-3.);
#13714=DERIVED_UNIT_ELEMENT(#13744,1.);
#13715=DERIVED_UNIT_ELEMENT(#57902,-3.);
#13716=DERIVED_UNIT_ELEMENT(#13744,1.);
#13717=DERIVED_UNIT_ELEMENT(#57902,-3.);
#13718=DERIVED_UNIT_ELEMENT(#13744,1.);
#13719=DERIVED_UNIT_ELEMENT(#57902,-3.);
#13720=DERIVED_UNIT_ELEMENT(#13744,1.);
#13721=DERIVED_UNIT_ELEMENT(#57902,-3.);
#13722=DERIVED_UNIT_ELEMENT(#13744,1.);
#13723=DERIVED_UNIT_ELEMENT(#57902,-3.);
#13724=DERIVED_UNIT_ELEMENT(#13744,1.);
#13725=DERIVED_UNIT_ELEMENT(#57902,-3.);
#13726=DERIVED_UNIT_ELEMENT(#13744,1.);
#13727=DERIVED_UNIT_ELEMENT(#57902,-3.);
#13728=DERIVED_UNIT_ELEMENT(#13744,1.);
#13729=DERIVED_UNIT_ELEMENT(#57902,-3.);
#13730=DERIVED_UNIT_ELEMENT(#13744,1.);
#13731=DERIVED_UNIT_ELEMENT(#57902,-3.);
#13732=DERIVED_UNIT_ELEMENT(#13744,1.);
#13733=DERIVED_UNIT_ELEMENT(#57902,-3.);
#13734=DERIVED_UNIT_ELEMENT(#13744,1.);
#13735=DERIVED_UNIT_ELEMENT(#57902,-3.);
#13736=DERIVED_UNIT_ELEMENT(#13744,1.);
#13737=DERIVED_UNIT_ELEMENT(#57902,-3.);
#13738=DERIVED_UNIT_ELEMENT(#13744,1.);
#13739=DERIVED_UNIT_ELEMENT(#57902,-3.);
#13740=DERIVED_UNIT_ELEMENT(#13744,1.);
#13741=DERIVED_UNIT_ELEMENT(#57902,-3.);
#13742=DERIVED_UNIT_ELEMENT(#13744,1.);
#13743=DERIVED_UNIT_ELEMENT(#57902,-3.);
#13744=(
MASS_UNIT()
NAMED_UNIT(*)
SI_UNIT(.KILO.,.GRAM.)
);
#13745=DERIVED_UNIT((#13644,#13645));
#13746=DERIVED_UNIT((#13646,#13647));
#13747=DERIVED_UNIT((#13648,#13649));
#13748=DERIVED_UNIT((#13650,#13651));
#13749=DERIVED_UNIT((#13652,#13653));
#13750=DERIVED_UNIT((#13654,#13655));
#13751=DERIVED_UNIT((#13656,#13657));
#13752=DERIVED_UNIT((#13658,#13659));
#13753=DERIVED_UNIT((#13660,#13661));
#13754=DERIVED_UNIT((#13662,#13663));
#13755=DERIVED_UNIT((#13664,#13665));
#13756=DERIVED_UNIT((#13666,#13667));
#13757=DERIVED_UNIT((#13668,#13669));
#13758=DERIVED_UNIT((#13670,#13671));
#13759=DERIVED_UNIT((#13672,#13673));
#13760=DERIVED_UNIT((#13674,#13675));
#13761=DERIVED_UNIT((#13676,#13677));
#13762=DERIVED_UNIT((#13678,#13679));
#13763=DERIVED_UNIT((#13680,#13681));
#13764=DERIVED_UNIT((#13682,#13683));
#13765=DERIVED_UNIT((#13684,#13685));
#13766=DERIVED_UNIT((#13686,#13687));
#13767=DERIVED_UNIT((#13688,#13689));
#13768=DERIVED_UNIT((#13690,#13691));
#13769=DERIVED_UNIT((#13692,#13693));
#13770=DERIVED_UNIT((#13694,#13695));
#13771=DERIVED_UNIT((#13696,#13697));
#13772=DERIVED_UNIT((#13698,#13699));
#13773=DERIVED_UNIT((#13700,#13701));
#13774=DERIVED_UNIT((#13702,#13703));
#13775=DERIVED_UNIT((#13704,#13705));
#13776=DERIVED_UNIT((#13706,#13707));
#13777=DERIVED_UNIT((#13708,#13709));
#13778=DERIVED_UNIT((#13710,#13711));
#13779=DERIVED_UNIT((#13712,#13713));
#13780=DERIVED_UNIT((#13714,#13715));
#13781=DERIVED_UNIT((#13716,#13717));
#13782=DERIVED_UNIT((#13718,#13719));
#13783=DERIVED_UNIT((#13720,#13721));
#13784=DERIVED_UNIT((#13722,#13723));
#13785=DERIVED_UNIT((#13724,#13725));
#13786=DERIVED_UNIT((#13726,#13727));
#13787=DERIVED_UNIT((#13728,#13729));
#13788=DERIVED_UNIT((#13730,#13731));
#13789=DERIVED_UNIT((#13732,#13733));
#13790=DERIVED_UNIT((#13734,#13735));
#13791=DERIVED_UNIT((#13736,#13737));
#13792=DERIVED_UNIT((#13738,#13739));
#13793=DERIVED_UNIT((#13740,#13741));
#13794=DERIVED_UNIT((#13742,#13743));
#13795=MEASURE_REPRESENTATION_ITEM('density measure',
POSITIVE_RATIO_MEASURE(7850.),#13745);
#13796=MEASURE_REPRESENTATION_ITEM('density measure',
POSITIVE_RATIO_MEASURE(7850.),#13746);
#13797=MEASURE_REPRESENTATION_ITEM('density measure',
POSITIVE_RATIO_MEASURE(7850.),#13747);
#13798=MEASURE_REPRESENTATION_ITEM('density measure',
POSITIVE_RATIO_MEASURE(7850.),#13748);
#13799=MEASURE_REPRESENTATION_ITEM('density measure',
POSITIVE_RATIO_MEASURE(7850.),#13749);
#13800=MEASURE_REPRESENTATION_ITEM('density measure',
POSITIVE_RATIO_MEASURE(7850.),#13750);
#13801=MEASURE_REPRESENTATION_ITEM('density measure',
POSITIVE_RATIO_MEASURE(7850.),#13751);
#13802=MEASURE_REPRESENTATION_ITEM('density measure',
POSITIVE_RATIO_MEASURE(7850.),#13752);
#13803=MEASURE_REPRESENTATION_ITEM('density measure',
POSITIVE_RATIO_MEASURE(7850.),#13753);
#13804=MEASURE_REPRESENTATION_ITEM('density measure',
POSITIVE_RATIO_MEASURE(7850.),#13754);
#13805=MEASURE_REPRESENTATION_ITEM('density measure',
POSITIVE_RATIO_MEASURE(7850.),#13755);
#13806=MEASURE_REPRESENTATION_ITEM('density measure',
POSITIVE_RATIO_MEASURE(7850.),#13756);
#13807=MEASURE_REPRESENTATION_ITEM('density measure',
POSITIVE_RATIO_MEASURE(7850.),#13757);
#13808=MEASURE_REPRESENTATION_ITEM('density measure',
POSITIVE_RATIO_MEASURE(7850.),#13758);
#13809=MEASURE_REPRESENTATION_ITEM('density measure',
POSITIVE_RATIO_MEASURE(7850.),#13759);
#13810=MEASURE_REPRESENTATION_ITEM('density measure',
POSITIVE_RATIO_MEASURE(7850.),#13760);
#13811=MEASURE_REPRESENTATION_ITEM('density measure',
POSITIVE_RATIO_MEASURE(7850.),#13761);
#13812=MEASURE_REPRESENTATION_ITEM('density measure',
POSITIVE_RATIO_MEASURE(7850.),#13762);
#13813=MEASURE_REPRESENTATION_ITEM('density measure',
POSITIVE_RATIO_MEASURE(7850.),#13763);
#13814=MEASURE_REPRESENTATION_ITEM('density measure',
POSITIVE_RATIO_MEASURE(7850.),#13764);
#13815=MEASURE_REPRESENTATION_ITEM('density measure',
POSITIVE_RATIO_MEASURE(7850.),#13765);
#13816=MEASURE_REPRESENTATION_ITEM('density measure',
POSITIVE_RATIO_MEASURE(7850.),#13766);
#13817=MEASURE_REPRESENTATION_ITEM('density measure',
POSITIVE_RATIO_MEASURE(7850.),#13767);
#13818=MEASURE_REPRESENTATION_ITEM('density measure',
POSITIVE_RATIO_MEASURE(7850.),#13768);
#13819=MEASURE_REPRESENTATION_ITEM('density measure',
POSITIVE_RATIO_MEASURE(7850.),#13769);
#13820=MEASURE_REPRESENTATION_ITEM('density measure',
POSITIVE_RATIO_MEASURE(7850.),#13770);
#13821=MEASURE_REPRESENTATION_ITEM('density measure',
POSITIVE_RATIO_MEASURE(7850.),#13771);
#13822=MEASURE_REPRESENTATION_ITEM('density measure',
POSITIVE_RATIO_MEASURE(7850.),#13772);
#13823=MEASURE_REPRESENTATION_ITEM('density measure',
POSITIVE_RATIO_MEASURE(7850.),#13773);
#13824=MEASURE_REPRESENTATION_ITEM('density measure',
POSITIVE_RATIO_MEASURE(7850.),#13774);
#13825=MEASURE_REPRESENTATION_ITEM('density measure',
POSITIVE_RATIO_MEASURE(7850.),#13775);
#13826=MEASURE_REPRESENTATION_ITEM('density measure',
POSITIVE_RATIO_MEASURE(7850.),#13776);
#13827=MEASURE_REPRESENTATION_ITEM('density measure',
POSITIVE_RATIO_MEASURE(7850.),#13777);
#13828=MEASURE_REPRESENTATION_ITEM('density measure',
POSITIVE_RATIO_MEASURE(7850.),#13778);
#13829=MEASURE_REPRESENTATION_ITEM('density measure',
POSITIVE_RATIO_MEASURE(7850.),#13779);
#13830=MEASURE_REPRESENTATION_ITEM('density measure',
POSITIVE_RATIO_MEASURE(7850.),#13780);
#13831=MEASURE_REPRESENTATION_ITEM('density measure',
POSITIVE_RATIO_MEASURE(7850.),#13781);
#13832=MEASURE_REPRESENTATION_ITEM('density measure',
POSITIVE_RATIO_MEASURE(7850.),#13782);
#13833=MEASURE_REPRESENTATION_ITEM('density measure',
POSITIVE_RATIO_MEASURE(7850.),#13783);
#13834=MEASURE_REPRESENTATION_ITEM('density measure',
POSITIVE_RATIO_MEASURE(7850.),#13784);
#13835=MEASURE_REPRESENTATION_ITEM('density measure',
POSITIVE_RATIO_MEASURE(7850.),#13785);
#13836=MEASURE_REPRESENTATION_ITEM('density measure',
POSITIVE_RATIO_MEASURE(7850.),#13786);
#13837=MEASURE_REPRESENTATION_ITEM('density measure',
POSITIVE_RATIO_MEASURE(7850.),#13787);
#13838=MEASURE_REPRESENTATION_ITEM('density measure',
POSITIVE_RATIO_MEASURE(7850.),#13788);
#13839=MEASURE_REPRESENTATION_ITEM('density measure',
POSITIVE_RATIO_MEASURE(7850.),#13789);
#13840=MEASURE_REPRESENTATION_ITEM('density measure',
POSITIVE_RATIO_MEASURE(7850.),#13790);
#13841=MEASURE_REPRESENTATION_ITEM('density measure',
POSITIVE_RATIO_MEASURE(7850.),#13791);
#13842=MEASURE_REPRESENTATION_ITEM('density measure',
POSITIVE_RATIO_MEASURE(7850.),#13792);
#13843=MEASURE_REPRESENTATION_ITEM('density measure',
POSITIVE_RATIO_MEASURE(7850.),#13793);
#13844=MEASURE_REPRESENTATION_ITEM('density measure',
POSITIVE_RATIO_MEASURE(7850.),#13794);
#13845=PROPERTY_DEFINITION_REPRESENTATION(#14095,#13945);
#13846=PROPERTY_DEFINITION_REPRESENTATION(#14096,#13946);
#13847=PROPERTY_DEFINITION_REPRESENTATION(#14097,#13947);
#13848=PROPERTY_DEFINITION_REPRESENTATION(#14098,#13948);
#13849=PROPERTY_DEFINITION_REPRESENTATION(#14099,#13949);
#13850=PROPERTY_DEFINITION_REPRESENTATION(#14100,#13950);
#13851=PROPERTY_DEFINITION_REPRESENTATION(#14101,#13951);
#13852=PROPERTY_DEFINITION_REPRESENTATION(#14102,#13952);
#13853=PROPERTY_DEFINITION_REPRESENTATION(#14103,#13953);
#13854=PROPERTY_DEFINITION_REPRESENTATION(#14104,#13954);
#13855=PROPERTY_DEFINITION_REPRESENTATION(#14105,#13955);
#13856=PROPERTY_DEFINITION_REPRESENTATION(#14106,#13956);
#13857=PROPERTY_DEFINITION_REPRESENTATION(#14107,#13957);
#13858=PROPERTY_DEFINITION_REPRESENTATION(#14108,#13958);
#13859=PROPERTY_DEFINITION_REPRESENTATION(#14109,#13959);
#13860=PROPERTY_DEFINITION_REPRESENTATION(#14110,#13960);
#13861=PROPERTY_DEFINITION_REPRESENTATION(#14111,#13961);
#13862=PROPERTY_DEFINITION_REPRESENTATION(#14112,#13962);
#13863=PROPERTY_DEFINITION_REPRESENTATION(#14113,#13963);
#13864=PROPERTY_DEFINITION_REPRESENTATION(#14114,#13964);
#13865=PROPERTY_DEFINITION_REPRESENTATION(#14115,#13965);
#13866=PROPERTY_DEFINITION_REPRESENTATION(#14116,#13966);
#13867=PROPERTY_DEFINITION_REPRESENTATION(#14117,#13967);
#13868=PROPERTY_DEFINITION_REPRESENTATION(#14118,#13968);
#13869=PROPERTY_DEFINITION_REPRESENTATION(#14119,#13969);
#13870=PROPERTY_DEFINITION_REPRESENTATION(#14120,#13970);
#13871=PROPERTY_DEFINITION_REPRESENTATION(#14121,#13971);
#13872=PROPERTY_DEFINITION_REPRESENTATION(#14122,#13972);
#13873=PROPERTY_DEFINITION_REPRESENTATION(#14123,#13973);
#13874=PROPERTY_DEFINITION_REPRESENTATION(#14124,#13974);
#13875=PROPERTY_DEFINITION_REPRESENTATION(#14125,#13975);
#13876=PROPERTY_DEFINITION_REPRESENTATION(#14126,#13976);
#13877=PROPERTY_DEFINITION_REPRESENTATION(#14127,#13977);
#13878=PROPERTY_DEFINITION_REPRESENTATION(#14128,#13978);
#13879=PROPERTY_DEFINITION_REPRESENTATION(#14129,#13979);
#13880=PROPERTY_DEFINITION_REPRESENTATION(#14130,#13980);
#13881=PROPERTY_DEFINITION_REPRESENTATION(#14131,#13981);
#13882=PROPERTY_DEFINITION_REPRESENTATION(#14132,#13982);
#13883=PROPERTY_DEFINITION_REPRESENTATION(#14133,#13983);
#13884=PROPERTY_DEFINITION_REPRESENTATION(#14134,#13984);
#13885=PROPERTY_DEFINITION_REPRESENTATION(#14135,#13985);
#13886=PROPERTY_DEFINITION_REPRESENTATION(#14136,#13986);
#13887=PROPERTY_DEFINITION_REPRESENTATION(#14137,#13987);
#13888=PROPERTY_DEFINITION_REPRESENTATION(#14138,#13988);
#13889=PROPERTY_DEFINITION_REPRESENTATION(#14139,#13989);
#13890=PROPERTY_DEFINITION_REPRESENTATION(#14140,#13990);
#13891=PROPERTY_DEFINITION_REPRESENTATION(#14141,#13991);
#13892=PROPERTY_DEFINITION_REPRESENTATION(#14142,#13992);
#13893=PROPERTY_DEFINITION_REPRESENTATION(#14143,#13993);
#13894=PROPERTY_DEFINITION_REPRESENTATION(#14144,#13994);
#13895=PROPERTY_DEFINITION_REPRESENTATION(#14145,#13995);
#13896=PROPERTY_DEFINITION_REPRESENTATION(#14146,#13996);
#13897=PROPERTY_DEFINITION_REPRESENTATION(#14147,#13997);
#13898=PROPERTY_DEFINITION_REPRESENTATION(#14148,#13998);
#13899=PROPERTY_DEFINITION_REPRESENTATION(#14149,#13999);
#13900=PROPERTY_DEFINITION_REPRESENTATION(#14150,#14000);
#13901=PROPERTY_DEFINITION_REPRESENTATION(#14151,#14001);
#13902=PROPERTY_DEFINITION_REPRESENTATION(#14152,#14002);
#13903=PROPERTY_DEFINITION_REPRESENTATION(#14153,#14003);
#13904=PROPERTY_DEFINITION_REPRESENTATION(#14154,#14004);
#13905=PROPERTY_DEFINITION_REPRESENTATION(#14155,#14005);
#13906=PROPERTY_DEFINITION_REPRESENTATION(#14156,#14006);
#13907=PROPERTY_DEFINITION_REPRESENTATION(#14157,#14007);
#13908=PROPERTY_DEFINITION_REPRESENTATION(#14158,#14008);
#13909=PROPERTY_DEFINITION_REPRESENTATION(#14159,#14009);
#13910=PROPERTY_DEFINITION_REPRESENTATION(#14160,#14010);
#13911=PROPERTY_DEFINITION_REPRESENTATION(#14161,#14011);
#13912=PROPERTY_DEFINITION_REPRESENTATION(#14162,#14012);
#13913=PROPERTY_DEFINITION_REPRESENTATION(#14163,#14013);
#13914=PROPERTY_DEFINITION_REPRESENTATION(#14164,#14014);
#13915=PROPERTY_DEFINITION_REPRESENTATION(#14165,#14015);
#13916=PROPERTY_DEFINITION_REPRESENTATION(#14166,#14016);
#13917=PROPERTY_DEFINITION_REPRESENTATION(#14167,#14017);
#13918=PROPERTY_DEFINITION_REPRESENTATION(#14168,#14018);
#13919=PROPERTY_DEFINITION_REPRESENTATION(#14169,#14019);
#13920=PROPERTY_DEFINITION_REPRESENTATION(#14170,#14020);
#13921=PROPERTY_DEFINITION_REPRESENTATION(#14171,#14021);
#13922=PROPERTY_DEFINITION_REPRESENTATION(#14172,#14022);
#13923=PROPERTY_DEFINITION_REPRESENTATION(#14173,#14023);
#13924=PROPERTY_DEFINITION_REPRESENTATION(#14174,#14024);
#13925=PROPERTY_DEFINITION_REPRESENTATION(#14175,#14025);
#13926=PROPERTY_DEFINITION_REPRESENTATION(#14176,#14026);
#13927=PROPERTY_DEFINITION_REPRESENTATION(#14177,#14027);
#13928=PROPERTY_DEFINITION_REPRESENTATION(#14178,#14028);
#13929=PROPERTY_DEFINITION_REPRESENTATION(#14179,#14029);
#13930=PROPERTY_DEFINITION_REPRESENTATION(#14180,#14030);
#13931=PROPERTY_DEFINITION_REPRESENTATION(#14181,#14031);
#13932=PROPERTY_DEFINITION_REPRESENTATION(#14182,#14032);
#13933=PROPERTY_DEFINITION_REPRESENTATION(#14183,#14033);
#13934=PROPERTY_DEFINITION_REPRESENTATION(#14184,#14034);
#13935=PROPERTY_DEFINITION_REPRESENTATION(#14185,#14035);
#13936=PROPERTY_DEFINITION_REPRESENTATION(#14186,#14036);
#13937=PROPERTY_DEFINITION_REPRESENTATION(#14187,#14037);
#13938=PROPERTY_DEFINITION_REPRESENTATION(#14188,#14038);
#13939=PROPERTY_DEFINITION_REPRESENTATION(#14189,#14039);
#13940=PROPERTY_DEFINITION_REPRESENTATION(#14190,#14040);
#13941=PROPERTY_DEFINITION_REPRESENTATION(#14191,#14041);
#13942=PROPERTY_DEFINITION_REPRESENTATION(#14192,#14042);
#13943=PROPERTY_DEFINITION_REPRESENTATION(#14193,#14043);
#13944=PROPERTY_DEFINITION_REPRESENTATION(#14194,#14044);
#13945=REPRESENTATION('material name',(#14045),#57844);
#13946=REPRESENTATION('density',(#13795),#57844);
#13947=REPRESENTATION('material name',(#14046),#57845);
#13948=REPRESENTATION('density',(#13796),#57845);
#13949=REPRESENTATION('material name',(#14047),#57846);
#13950=REPRESENTATION('density',(#13797),#57846);
#13951=REPRESENTATION('material name',(#14048),#57847);
#13952=REPRESENTATION('density',(#13798),#57847);
#13953=REPRESENTATION('material name',(#14049),#57848);
#13954=REPRESENTATION('density',(#13799),#57848);
#13955=REPRESENTATION('material name',(#14050),#57849);
#13956=REPRESENTATION('density',(#13800),#57849);
#13957=REPRESENTATION('material name',(#14051),#57850);
#13958=REPRESENTATION('density',(#13801),#57850);
#13959=REPRESENTATION('material name',(#14052),#57851);
#13960=REPRESENTATION('density',(#13802),#57851);
#13961=REPRESENTATION('material name',(#14053),#57852);
#13962=REPRESENTATION('density',(#13803),#57852);
#13963=REPRESENTATION('material name',(#14054),#57853);
#13964=REPRESENTATION('density',(#13804),#57853);
#13965=REPRESENTATION('material name',(#14055),#57854);
#13966=REPRESENTATION('density',(#13805),#57854);
#13967=REPRESENTATION('material name',(#14056),#57855);
#13968=REPRESENTATION('density',(#13806),#57855);
#13969=REPRESENTATION('material name',(#14057),#57857);
#13970=REPRESENTATION('density',(#13807),#57857);
#13971=REPRESENTATION('material name',(#14058),#57858);
#13972=REPRESENTATION('density',(#13808),#57858);
#13973=REPRESENTATION('material name',(#14059),#57859);
#13974=REPRESENTATION('density',(#13809),#57859);
#13975=REPRESENTATION('material name',(#14060),#57860);
#13976=REPRESENTATION('density',(#13810),#57860);
#13977=REPRESENTATION('material name',(#14061),#57861);
#13978=REPRESENTATION('density',(#13811),#57861);
#13979=REPRESENTATION('material name',(#14062),#57862);
#13980=REPRESENTATION('density',(#13812),#57862);
#13981=REPRESENTATION('material name',(#14063),#57864);
#13982=REPRESENTATION('density',(#13813),#57864);
#13983=REPRESENTATION('material name',(#14064),#57865);
#13984=REPRESENTATION('density',(#13814),#57865);
#13985=REPRESENTATION('material name',(#14065),#57866);
#13986=REPRESENTATION('density',(#13815),#57866);
#13987=REPRESENTATION('material name',(#14066),#57867);
#13988=REPRESENTATION('density',(#13816),#57867);
#13989=REPRESENTATION('material name',(#14067),#57868);
#13990=REPRESENTATION('density',(#13817),#57868);
#13991=REPRESENTATION('material name',(#14068),#57870);
#13992=REPRESENTATION('density',(#13818),#57870);
#13993=REPRESENTATION('material name',(#14069),#57871);
#13994=REPRESENTATION('density',(#13819),#57871);
#13995=REPRESENTATION('material name',(#14070),#57872);
#13996=REPRESENTATION('density',(#13820),#57872);
#13997=REPRESENTATION('material name',(#14071),#57873);
#13998=REPRESENTATION('density',(#13821),#57873);
#13999=REPRESENTATION('material name',(#14072),#57874);
#14000=REPRESENTATION('density',(#13822),#57874);
#14001=REPRESENTATION('material name',(#14073),#57876);
#14002=REPRESENTATION('density',(#13823),#57876);
#14003=REPRESENTATION('material name',(#14074),#57877);
#14004=REPRESENTATION('density',(#13824),#57877);
#14005=REPRESENTATION('material name',(#14075),#57878);
#14006=REPRESENTATION('density',(#13825),#57878);
#14007=REPRESENTATION('material name',(#14076),#57879);
#14008=REPRESENTATION('density',(#13826),#57879);
#14009=REPRESENTATION('material name',(#14077),#57880);
#14010=REPRESENTATION('density',(#13827),#57880);
#14011=REPRESENTATION('material name',(#14078),#57882);
#14012=REPRESENTATION('density',(#13828),#57882);
#14013=REPRESENTATION('material name',(#14079),#57883);
#14014=REPRESENTATION('density',(#13829),#57883);
#14015=REPRESENTATION('material name',(#14080),#57884);
#14016=REPRESENTATION('density',(#13830),#57884);
#14017=REPRESENTATION('material name',(#14081),#57885);
#14018=REPRESENTATION('density',(#13831),#57885);
#14019=REPRESENTATION('material name',(#14082),#57886);
#14020=REPRESENTATION('density',(#13832),#57886);
#14021=REPRESENTATION('material name',(#14083),#57887);
#14022=REPRESENTATION('density',(#13833),#57887);
#14023=REPRESENTATION('material name',(#14084),#57888);
#14024=REPRESENTATION('density',(#13834),#57888);
#14025=REPRESENTATION('material name',(#14085),#57889);
#14026=REPRESENTATION('density',(#13835),#57889);
#14027=REPRESENTATION('material name',(#14086),#57891);
#14028=REPRESENTATION('density',(#13836),#57891);
#14029=REPRESENTATION('material name',(#14087),#57892);
#14030=REPRESENTATION('density',(#13837),#57892);
#14031=REPRESENTATION('material name',(#14088),#57893);
#14032=REPRESENTATION('density',(#13838),#57893);
#14033=REPRESENTATION('material name',(#14089),#57894);
#14034=REPRESENTATION('density',(#13839),#57894);
#14035=REPRESENTATION('material name',(#14090),#57895);
#14036=REPRESENTATION('density',(#13840),#57895);
#14037=REPRESENTATION('material name',(#14091),#57896);
#14038=REPRESENTATION('density',(#13841),#57896);
#14039=REPRESENTATION('material name',(#14092),#57897);
#14040=REPRESENTATION('density',(#13842),#57897);
#14041=REPRESENTATION('material name',(#14093),#57898);
#14042=REPRESENTATION('density',(#13843),#57898);
#14043=REPRESENTATION('material name',(#14094),#57899);
#14044=REPRESENTATION('density',(#13844),#57899);
#14045=DESCRIPTIVE_REPRESENTATION_ITEM('Steel','Steel');
#14046=DESCRIPTIVE_REPRESENTATION_ITEM('Steel','Steel');
#14047=DESCRIPTIVE_REPRESENTATION_ITEM('Steel','Steel');
#14048=DESCRIPTIVE_REPRESENTATION_ITEM('Steel','Steel');
#14049=DESCRIPTIVE_REPRESENTATION_ITEM('Steel','Steel');
#14050=DESCRIPTIVE_REPRESENTATION_ITEM('Steel','Steel');
#14051=DESCRIPTIVE_REPRESENTATION_ITEM('Steel','Steel');
#14052=DESCRIPTIVE_REPRESENTATION_ITEM('Steel','Steel');
#14053=DESCRIPTIVE_REPRESENTATION_ITEM('Steel','Steel');
#14054=DESCRIPTIVE_REPRESENTATION_ITEM('Steel','Steel');
#14055=DESCRIPTIVE_REPRESENTATION_ITEM('Steel','Steel');
#14056=DESCRIPTIVE_REPRESENTATION_ITEM('Steel','Steel');
#14057=DESCRIPTIVE_REPRESENTATION_ITEM('Steel','Steel');
#14058=DESCRIPTIVE_REPRESENTATION_ITEM('Steel','Steel');
#14059=DESCRIPTIVE_REPRESENTATION_ITEM('Steel','Steel');
#14060=DESCRIPTIVE_REPRESENTATION_ITEM('Steel','Steel');
#14061=DESCRIPTIVE_REPRESENTATION_ITEM('Steel','Steel');
#14062=DESCRIPTIVE_REPRESENTATION_ITEM('Steel','Steel');
#14063=DESCRIPTIVE_REPRESENTATION_ITEM('Steel','Steel');
#14064=DESCRIPTIVE_REPRESENTATION_ITEM('Steel','Steel');
#14065=DESCRIPTIVE_REPRESENTATION_ITEM('Steel','Steel');
#14066=DESCRIPTIVE_REPRESENTATION_ITEM('Steel','Steel');
#14067=DESCRIPTIVE_REPRESENTATION_ITEM('Steel','Steel');
#14068=DESCRIPTIVE_REPRESENTATION_ITEM('Steel','Steel');
#14069=DESCRIPTIVE_REPRESENTATION_ITEM('Steel','Steel');
#14070=DESCRIPTIVE_REPRESENTATION_ITEM('Steel','Steel');
#14071=DESCRIPTIVE_REPRESENTATION_ITEM('Steel','Steel');
#14072=DESCRIPTIVE_REPRESENTATION_ITEM('Steel','Steel');
#14073=DESCRIPTIVE_REPRESENTATION_ITEM('Steel','Steel');
#14074=DESCRIPTIVE_REPRESENTATION_ITEM('Steel','Steel');
#14075=DESCRIPTIVE_REPRESENTATION_ITEM('Steel','Steel');
#14076=DESCRIPTIVE_REPRESENTATION_ITEM('Steel','Steel');
#14077=DESCRIPTIVE_REPRESENTATION_ITEM('Steel','Steel');
#14078=DESCRIPTIVE_REPRESENTATION_ITEM('Steel','Steel');
#14079=DESCRIPTIVE_REPRESENTATION_ITEM('Steel','Steel');
#14080=DESCRIPTIVE_REPRESENTATION_ITEM('Steel','Steel');
#14081=DESCRIPTIVE_REPRESENTATION_ITEM('Steel','Steel');
#14082=DESCRIPTIVE_REPRESENTATION_ITEM('Steel','Steel');
#14083=DESCRIPTIVE_REPRESENTATION_ITEM('Steel','Steel');
#14084=DESCRIPTIVE_REPRESENTATION_ITEM('Steel','Steel');
#14085=DESCRIPTIVE_REPRESENTATION_ITEM('Steel','Steel');
#14086=DESCRIPTIVE_REPRESENTATION_ITEM('Steel','Steel');
#14087=DESCRIPTIVE_REPRESENTATION_ITEM('Steel','Steel');
#14088=DESCRIPTIVE_REPRESENTATION_ITEM('Steel','Steel');
#14089=DESCRIPTIVE_REPRESENTATION_ITEM('Steel','Steel');
#14090=DESCRIPTIVE_REPRESENTATION_ITEM('Steel','Steel');
#14091=DESCRIPTIVE_REPRESENTATION_ITEM('Steel','Steel');
#14092=DESCRIPTIVE_REPRESENTATION_ITEM('Steel','Steel');
#14093=DESCRIPTIVE_REPRESENTATION_ITEM('Steel','Steel');
#14094=DESCRIPTIVE_REPRESENTATION_ITEM('Steel','Steel');
#14095=PROPERTY_DEFINITION('material property','material name',#58170);
#14096=PROPERTY_DEFINITION('material property','density of part',#58170);
#14097=PROPERTY_DEFINITION('material property','material name',#58171);
#14098=PROPERTY_DEFINITION('material property','density of part',#58171);
#14099=PROPERTY_DEFINITION('material property','material name',#58172);
#14100=PROPERTY_DEFINITION('material property','density of part',#58172);
#14101=PROPERTY_DEFINITION('material property','material name',#58173);
#14102=PROPERTY_DEFINITION('material property','density of part',#58173);
#14103=PROPERTY_DEFINITION('material property','material name',#58174);
#14104=PROPERTY_DEFINITION('material property','density of part',#58174);
#14105=PROPERTY_DEFINITION('material property','material name',#58175);
#14106=PROPERTY_DEFINITION('material property','density of part',#58175);
#14107=PROPERTY_DEFINITION('material property','material name',#58176);
#14108=PROPERTY_DEFINITION('material property','density of part',#58176);
#14109=PROPERTY_DEFINITION('material property','material name',#58177);
#14110=PROPERTY_DEFINITION('material property','density of part',#58177);
#14111=PROPERTY_DEFINITION('material property','material name',#58178);
#14112=PROPERTY_DEFINITION('material property','density of part',#58178);
#14113=PROPERTY_DEFINITION('material property','material name',#58179);
#14114=PROPERTY_DEFINITION('material property','density of part',#58179);
#14115=PROPERTY_DEFINITION('material property','material name',#58180);
#14116=PROPERTY_DEFINITION('material property','density of part',#58180);
#14117=PROPERTY_DEFINITION('material property','material name',#58181);
#14118=PROPERTY_DEFINITION('material property','density of part',#58181);
#14119=PROPERTY_DEFINITION('material property','material name',#58183);
#14120=PROPERTY_DEFINITION('material property','density of part',#58183);
#14121=PROPERTY_DEFINITION('material property','material name',#58184);
#14122=PROPERTY_DEFINITION('material property','density of part',#58184);
#14123=PROPERTY_DEFINITION('material property','material name',#58185);
#14124=PROPERTY_DEFINITION('material property','density of part',#58185);
#14125=PROPERTY_DEFINITION('material property','material name',#58186);
#14126=PROPERTY_DEFINITION('material property','density of part',#58186);
#14127=PROPERTY_DEFINITION('material property','material name',#58187);
#14128=PROPERTY_DEFINITION('material property','density of part',#58187);
#14129=PROPERTY_DEFINITION('material property','material name',#58188);
#14130=PROPERTY_DEFINITION('material property','density of part',#58188);
#14131=PROPERTY_DEFINITION('material property','material name',#58190);
#14132=PROPERTY_DEFINITION('material property','density of part',#58190);
#14133=PROPERTY_DEFINITION('material property','material name',#58191);
#14134=PROPERTY_DEFINITION('material property','density of part',#58191);
#14135=PROPERTY_DEFINITION('material property','material name',#58192);
#14136=PROPERTY_DEFINITION('material property','density of part',#58192);
#14137=PROPERTY_DEFINITION('material property','material name',#58193);
#14138=PROPERTY_DEFINITION('material property','density of part',#58193);
#14139=PROPERTY_DEFINITION('material property','material name',#58194);
#14140=PROPERTY_DEFINITION('material property','density of part',#58194);
#14141=PROPERTY_DEFINITION('material property','material name',#58196);
#14142=PROPERTY_DEFINITION('material property','density of part',#58196);
#14143=PROPERTY_DEFINITION('material property','material name',#58197);
#14144=PROPERTY_DEFINITION('material property','density of part',#58197);
#14145=PROPERTY_DEFINITION('material property','material name',#58198);
#14146=PROPERTY_DEFINITION('material property','density of part',#58198);
#14147=PROPERTY_DEFINITION('material property','material name',#58199);
#14148=PROPERTY_DEFINITION('material property','density of part',#58199);
#14149=PROPERTY_DEFINITION('material property','material name',#58200);
#14150=PROPERTY_DEFINITION('material property','density of part',#58200);
#14151=PROPERTY_DEFINITION('material property','material name',#58202);
#14152=PROPERTY_DEFINITION('material property','density of part',#58202);
#14153=PROPERTY_DEFINITION('material property','material name',#58203);
#14154=PROPERTY_DEFINITION('material property','density of part',#58203);
#14155=PROPERTY_DEFINITION('material property','material name',#58204);
#14156=PROPERTY_DEFINITION('material property','density of part',#58204);
#14157=PROPERTY_DEFINITION('material property','material name',#58205);
#14158=PROPERTY_DEFINITION('material property','density of part',#58205);
#14159=PROPERTY_DEFINITION('material property','material name',#58206);
#14160=PROPERTY_DEFINITION('material property','density of part',#58206);
#14161=PROPERTY_DEFINITION('material property','material name',#58208);
#14162=PROPERTY_DEFINITION('material property','density of part',#58208);
#14163=PROPERTY_DEFINITION('material property','material name',#58209);
#14164=PROPERTY_DEFINITION('material property','density of part',#58209);
#14165=PROPERTY_DEFINITION('material property','material name',#58210);
#14166=PROPERTY_DEFINITION('material property','density of part',#58210);
#14167=PROPERTY_DEFINITION('material property','material name',#58211);
#14168=PROPERTY_DEFINITION('material property','density of part',#58211);
#14169=PROPERTY_DEFINITION('material property','material name',#58212);
#14170=PROPERTY_DEFINITION('material property','density of part',#58212);
#14171=PROPERTY_DEFINITION('material property','material name',#58213);
#14172=PROPERTY_DEFINITION('material property','density of part',#58213);
#14173=PROPERTY_DEFINITION('material property','material name',#58214);
#14174=PROPERTY_DEFINITION('material property','density of part',#58214);
#14175=PROPERTY_DEFINITION('material property','material name',#58215);
#14176=PROPERTY_DEFINITION('material property','density of part',#58215);
#14177=PROPERTY_DEFINITION('material property','material name',#58217);
#14178=PROPERTY_DEFINITION('material property','density of part',#58217);
#14179=PROPERTY_DEFINITION('material property','material name',#58218);
#14180=PROPERTY_DEFINITION('material property','density of part',#58218);
#14181=PROPERTY_DEFINITION('material property','material name',#58219);
#14182=PROPERTY_DEFINITION('material property','density of part',#58219);
#14183=PROPERTY_DEFINITION('material property','material name',#58220);
#14184=PROPERTY_DEFINITION('material property','density of part',#58220);
#14185=PROPERTY_DEFINITION('material property','material name',#58221);
#14186=PROPERTY_DEFINITION('material property','density of part',#58221);
#14187=PROPERTY_DEFINITION('material property','material name',#58222);
#14188=PROPERTY_DEFINITION('material property','density of part',#58222);
#14189=PROPERTY_DEFINITION('material property','material name',#58223);
#14190=PROPERTY_DEFINITION('material property','density of part',#58223);
#14191=PROPERTY_DEFINITION('material property','material name',#58224);
#14192=PROPERTY_DEFINITION('material property','density of part',#58224);
#14193=PROPERTY_DEFINITION('material property','material name',#58225);
#14194=PROPERTY_DEFINITION('material property','density of part',#58225);
#14195=AXIS2_PLACEMENT_3D('',#19233,#15578,#15579);
#14196=AXIS2_PLACEMENT_3D('',#19234,#15580,#15581);
#14197=AXIS2_PLACEMENT_3D('',#19235,#15582,#15583);
#14198=AXIS2_PLACEMENT_3D('',#19236,#15584,#15585);
#14199=AXIS2_PLACEMENT_3D('',#19238,#15586,#15587);
#14200=AXIS2_PLACEMENT_3D('',#19241,#15589,#15590);
#14201=AXIS2_PLACEMENT_3D('',#19242,#15591,#15592);
#14202=AXIS2_PLACEMENT_3D('',#19244,#15593,#15594);
#14203=AXIS2_PLACEMENT_3D('',#19247,#15596,#15597);
#14204=AXIS2_PLACEMENT_3D('',#19248,#15598,#15599);
#14205=AXIS2_PLACEMENT_3D('',#19250,#15600,#15601);
#14206=AXIS2_PLACEMENT_3D('',#19253,#15603,#15604);
#14207=AXIS2_PLACEMENT_3D('',#19254,#15605,#15606);
#14208=AXIS2_PLACEMENT_3D('',#19256,#15607,#15608);
#14209=AXIS2_PLACEMENT_3D('',#19259,#15610,#15611);
#14210=AXIS2_PLACEMENT_3D('',#19260,#15612,#15613);
#14211=AXIS2_PLACEMENT_3D('',#19262,#15614,#15615);
#14212=AXIS2_PLACEMENT_3D('',#19265,#15617,#15618);
#14213=AXIS2_PLACEMENT_3D('',#19266,#15619,#15620);
#14214=AXIS2_PLACEMENT_3D('',#19268,#15621,#15622);
#14215=AXIS2_PLACEMENT_3D('',#19271,#15624,#15625);
#14216=AXIS2_PLACEMENT_3D('',#19272,#15626,#15627);
#14217=AXIS2_PLACEMENT_3D('',#19274,#15628,#15629);
#14218=AXIS2_PLACEMENT_3D('',#19277,#15631,#15632);
#14219=AXIS2_PLACEMENT_3D('',#19278,#15633,#15634);
#14220=AXIS2_PLACEMENT_3D('',#19280,#15635,#15636);
#14221=AXIS2_PLACEMENT_3D('',#19283,#15638,#15639);
#14222=AXIS2_PLACEMENT_3D('',#19284,#15640,#15641);
#14223=AXIS2_PLACEMENT_3D('',#19286,#15642,#15643);
#14224=AXIS2_PLACEMENT_3D('',#19289,#15645,#15646);
#14225=AXIS2_PLACEMENT_3D('',#19290,#15647,#15648);
#14226=AXIS2_PLACEMENT_3D('',#19292,#15649,#15650);
#14227=AXIS2_PLACEMENT_3D('',#19295,#15652,#15653);
#14228=AXIS2_PLACEMENT_3D('',#19296,#15654,#15655);
#14229=AXIS2_PLACEMENT_3D('',#19298,#15656,#15657);
#14230=AXIS2_PLACEMENT_3D('',#19301,#15659,#15660);
#14231=AXIS2_PLACEMENT_3D('',#19302,#15661,#15662);
#14232=AXIS2_PLACEMENT_3D('',#19304,#15663,#15664);
#14233=AXIS2_PLACEMENT_3D('',#19307,#15666,#15667);
#14234=AXIS2_PLACEMENT_3D('',#19308,#15668,#15669);
#14235=AXIS2_PLACEMENT_3D('',#19317,#15674,#15675);
#14236=AXIS2_PLACEMENT_3D('',#19323,#15679,#15680);
#14237=AXIS2_PLACEMENT_3D('',#19329,#15684,#15685);
#14238=AXIS2_PLACEMENT_3D('',#19332,#15688,#15689);
#14239=AXIS2_PLACEMENT_3D('',#19333,#15690,#15691);
#14240=AXIS2_PLACEMENT_3D('',#19334,#15692,#15693);
#14241=AXIS2_PLACEMENT_3D('',#19335,#15694,#15695);
#14242=AXIS2_PLACEMENT_3D('',#19344,#15700,#15701);
#14243=AXIS2_PLACEMENT_3D('',#19350,#15705,#15706);
#14244=AXIS2_PLACEMENT_3D('',#19356,#15710,#15711);
#14245=AXIS2_PLACEMENT_3D('',#19359,#15714,#15715);
#14246=AXIS2_PLACEMENT_3D('',#19360,#15716,#15717);
#14247=AXIS2_PLACEMENT_3D('',#19361,#15718,#15719);
#14248=AXIS2_PLACEMENT_3D('',#19362,#15720,#15721);
#14249=AXIS2_PLACEMENT_3D('',#19371,#15726,#15727);
#14250=AXIS2_PLACEMENT_3D('',#19377,#15731,#15732);
#14251=AXIS2_PLACEMENT_3D('',#19383,#15736,#15737);
#14252=AXIS2_PLACEMENT_3D('',#19386,#15740,#15741);
#14253=AXIS2_PLACEMENT_3D('',#19387,#15742,#15743);
#14254=AXIS2_PLACEMENT_3D('',#19388,#15744,#15745);
#14255=AXIS2_PLACEMENT_3D('',#19389,#15746,#15747);
#14256=AXIS2_PLACEMENT_3D('',#19467,#15749,#15750);
#14257=AXIS2_PLACEMENT_3D('',#19469,#15751,#15752);
#14258=AXIS2_PLACEMENT_3D('',#19472,#15754,#15755);
#14259=AXIS2_PLACEMENT_3D('',#19473,#15756,#15757);
#14260=AXIS2_PLACEMENT_3D('',#19474,#15758,#15759);
#14261=AXIS2_PLACEMENT_3D('',#19476,#15760,#15761);
#14262=AXIS2_PLACEMENT_3D('',#19479,#15763,#15764);
#14263=AXIS2_PLACEMENT_3D('',#19480,#15765,#15766);
#14264=AXIS2_PLACEMENT_3D('',#19481,#15767,#15768);
#14265=AXIS2_PLACEMENT_3D('',#19483,#15769,#15770);
#14266=AXIS2_PLACEMENT_3D('',#19486,#15772,#15773);
#14267=AXIS2_PLACEMENT_3D('',#19487,#15774,#15775);
#14268=AXIS2_PLACEMENT_3D('',#19488,#15776,#15777);
#14269=AXIS2_PLACEMENT_3D('',#19490,#15778,#15779);
#14270=AXIS2_PLACEMENT_3D('',#19493,#15781,#15782);
#14271=AXIS2_PLACEMENT_3D('',#19494,#15783,#15784);
#14272=AXIS2_PLACEMENT_3D('',#19495,#15785,#15786);
#14273=AXIS2_PLACEMENT_3D('',#19498,#15787,#15788);
#14274=AXIS2_PLACEMENT_3D('',#19499,#15789,#15790);
#14275=AXIS2_PLACEMENT_3D('',#19500,#15791,#15792);
#14276=AXIS2_PLACEMENT_3D('',#19504,#15794,#15795);
#14277=AXIS2_PLACEMENT_3D('',#19506,#15797,#15798);
#14278=AXIS2_PLACEMENT_3D('',#19511,#15800,#15801);
#14279=AXIS2_PLACEMENT_3D('',#19514,#15803,#15804);
#14280=AXIS2_PLACEMENT_3D('',#19515,#15805,#15806);
#14281=AXIS2_PLACEMENT_3D('',#19516,#15807,#15808);
#14282=AXIS2_PLACEMENT_3D('',#19517,#15809,#15810);
#14283=AXIS2_PLACEMENT_3D('',#19522,#15812,#15813);
#14284=AXIS2_PLACEMENT_3D('',#19525,#15815,#15816);
#14285=AXIS2_PLACEMENT_3D('',#19526,#15817,#15818);
#14286=AXIS2_PLACEMENT_3D('',#19527,#15819,#15820);
#14287=AXIS2_PLACEMENT_3D('',#19528,#15821,#15822);
#14288=AXIS2_PLACEMENT_3D('',#19533,#15824,#15825);
#14289=AXIS2_PLACEMENT_3D('',#19536,#15827,#15828);
#14290=AXIS2_PLACEMENT_3D('',#19537,#15829,#15830);
#14291=AXIS2_PLACEMENT_3D('',#19538,#15831,#15832);
#14292=AXIS2_PLACEMENT_3D('',#19539,#15833,#15834);
#14293=AXIS2_PLACEMENT_3D('',#19541,#15835,#15836);
#14294=AXIS2_PLACEMENT_3D('',#19544,#15838,#15839);
#14295=AXIS2_PLACEMENT_3D('',#19545,#15840,#15841);
#14296=AXIS2_PLACEMENT_3D('',#19546,#15842,#15843);
#14297=AXIS2_PLACEMENT_3D('',#19547,#15844,#15845);
#14298=AXIS2_PLACEMENT_3D('',#19548,#15846,#15847);
#14299=AXIS2_PLACEMENT_3D('',#19549,#15848,#15849);
#14300=AXIS2_PLACEMENT_3D('',#19551,#15850,#15851);
#14301=AXIS2_PLACEMENT_3D('',#19553,#15852,#15853);
#14302=AXIS2_PLACEMENT_3D('',#19555,#15854,#15855);
#14303=AXIS2_PLACEMENT_3D('',#19557,#15856,#15857);
#14304=AXIS2_PLACEMENT_3D('',#19559,#15858,#15859);
#14305=AXIS2_PLACEMENT_3D('',#19560,#15860,#15861);
#14306=AXIS2_PLACEMENT_3D('',#19562,#15862,#15863);
#14307=AXIS2_PLACEMENT_3D('',#19564,#15865,#15866);
#14308=AXIS2_PLACEMENT_3D('',#19566,#15867,#15868);
#14309=AXIS2_PLACEMENT_3D('',#19568,#15870,#15871);
#14310=AXIS2_PLACEMENT_3D('',#19570,#15872,#15873);
#14311=AXIS2_PLACEMENT_3D('',#19572,#15875,#15876);
#14312=AXIS2_PLACEMENT_3D('',#19574,#15877,#15878);
#14313=AXIS2_PLACEMENT_3D('',#19576,#15880,#15881);
#14314=AXIS2_PLACEMENT_3D('',#19578,#15882,#15883);
#14315=AXIS2_PLACEMENT_3D('',#19581,#15885,#15886);
#14316=AXIS2_PLACEMENT_3D('',#19582,#15887,#15888);
#14317=AXIS2_PLACEMENT_3D('',#19584,#15889,#15890);
#14318=AXIS2_PLACEMENT_3D('',#19585,#15891,#15892);
#14319=AXIS2_PLACEMENT_3D('',#19588,#15894,#15895);
#14320=AXIS2_PLACEMENT_3D('',#19589,#15896,#15897);
#14321=AXIS2_PLACEMENT_3D('',#19592,#15899,#15900);
#14322=AXIS2_PLACEMENT_3D('',#19593,#15901,#15902);
#14323=AXIS2_PLACEMENT_3D('',#19594,#15903,#15904);
#14324=AXIS2_PLACEMENT_3D('',#19595,#15905,#15906);
#14325=AXIS2_PLACEMENT_3D('',#19596,#15907,#15908);
#14326=AXIS2_PLACEMENT_3D('',#19598,#15909,#15910);
#14327=AXIS2_PLACEMENT_3D('',#19601,#15912,#15913);
#14328=AXIS2_PLACEMENT_3D('',#19602,#15914,#15915);
#14329=AXIS2_PLACEMENT_3D('',#19604,#15916,#15917);
#14330=AXIS2_PLACEMENT_3D('',#19607,#15919,#15920);
#14331=AXIS2_PLACEMENT_3D('',#19608,#15921,#15922);
#14332=AXIS2_PLACEMENT_3D('',#19609,#15923,#15924);
#14333=AXIS2_PLACEMENT_3D('',#19610,#15925,#15926);
#14334=AXIS2_PLACEMENT_3D('',#19611,#15927,#15928);
#14335=AXIS2_PLACEMENT_3D('',#19616,#15930,#15931);
#14336=AXIS2_PLACEMENT_3D('',#19619,#15933,#15934);
#14337=AXIS2_PLACEMENT_3D('',#19620,#15935,#15936);
#14338=AXIS2_PLACEMENT_3D('',#19625,#15938,#15939);
#14339=AXIS2_PLACEMENT_3D('',#19628,#15941,#15942);
#14340=AXIS2_PLACEMENT_3D('',#19629,#15943,#15944);
#14341=AXIS2_PLACEMENT_3D('',#19634,#15946,#15947);
#14342=AXIS2_PLACEMENT_3D('',#19637,#15949,#15950);
#14343=AXIS2_PLACEMENT_3D('',#19638,#15951,#15952);
#14344=AXIS2_PLACEMENT_3D('',#19643,#15954,#15955);
#14345=AXIS2_PLACEMENT_3D('',#19646,#15957,#15958);
#14346=AXIS2_PLACEMENT_3D('',#19647,#15959,#15960);
#14347=AXIS2_PLACEMENT_3D('',#19648,#15961,#15962);
#14348=AXIS2_PLACEMENT_3D('',#19649,#15963,#15964);
#14349=AXIS2_PLACEMENT_3D('',#19650,#15965,#15966);
#14350=AXIS2_PLACEMENT_3D('',#19651,#15967,#15968);
#14351=AXIS2_PLACEMENT_3D('',#19653,#15969,#15970);
#14352=AXIS2_PLACEMENT_3D('',#19654,#15971,#15972);
#14353=AXIS2_PLACEMENT_3D('',#19655,#15973,#15974);
#14354=AXIS2_PLACEMENT_3D('',#19656,#15975,#15976);
#14355=AXIS2_PLACEMENT_3D('',#19657,#15977,#15978);
#14356=AXIS2_PLACEMENT_3D('',#19658,#15979,#15980);
#14357=AXIS2_PLACEMENT_3D('',#19659,#15981,#15982);
#14358=AXIS2_PLACEMENT_3D('',#19660,#15983,#15984);
#14359=AXIS2_PLACEMENT_3D('',#19661,#15985,#15986);
#14360=AXIS2_PLACEMENT_3D('',#19662,#15987,#15988);
#14361=AXIS2_PLACEMENT_3D('',#19665,#15990,#15991);
#14362=AXIS2_PLACEMENT_3D('',#19666,#15992,#15993);
#14363=AXIS2_PLACEMENT_3D('',#19668,#15994,#15995);
#14364=AXIS2_PLACEMENT_3D('',#19669,#15996,#15997);
#14365=AXIS2_PLACEMENT_3D('',#19671,#15998,#15999);
#14366=AXIS2_PLACEMENT_3D('',#19673,#16001,#16002);
#14367=AXIS2_PLACEMENT_3D('',#19674,#16003,#16004);
#14368=AXIS2_PLACEMENT_3D('',#19675,#16005,#16006);
#14369=AXIS2_PLACEMENT_3D('',#19677,#16007,#16008);
#14370=AXIS2_PLACEMENT_3D('',#19680,#16010,#16011);
#14371=AXIS2_PLACEMENT_3D('',#19681,#16012,#16013);
#14372=AXIS2_PLACEMENT_3D('',#19683,#16014,#16015);
#14373=AXIS2_PLACEMENT_3D('',#19686,#16017,#16018);
#14374=AXIS2_PLACEMENT_3D('',#19687,#16019,#16020);
#14375=AXIS2_PLACEMENT_3D('',#19689,#16021,#16022);
#14376=AXIS2_PLACEMENT_3D('',#19692,#16024,#16025);
#14377=AXIS2_PLACEMENT_3D('',#19693,#16026,#16027);
#14378=AXIS2_PLACEMENT_3D('',#19695,#16028,#16029);
#14379=AXIS2_PLACEMENT_3D('',#19698,#16031,#16032);
#14380=AXIS2_PLACEMENT_3D('',#19699,#16033,#16034);
#14381=AXIS2_PLACEMENT_3D('',#19701,#16035,#16036);
#14382=AXIS2_PLACEMENT_3D('',#19704,#16038,#16039);
#14383=AXIS2_PLACEMENT_3D('',#19705,#16040,#16041);
#14384=AXIS2_PLACEMENT_3D('',#19706,#16042,#16043);
#14385=AXIS2_PLACEMENT_3D('',#19708,#16044,#16045);
#14386=AXIS2_PLACEMENT_3D('',#19711,#16047,#16048);
#14387=AXIS2_PLACEMENT_3D('',#19712,#16049,#16050);
#14388=AXIS2_PLACEMENT_3D('',#19713,#16051,#16052);
#14389=AXIS2_PLACEMENT_3D('',#19714,#16053,#16054);
#14390=AXIS2_PLACEMENT_3D('',#19715,#16055,#16056);
#14391=AXIS2_PLACEMENT_3D('',#19719,#16058,#16059);
#14392=AXIS2_PLACEMENT_3D('',#19720,#16060,#16061);
#14393=AXIS2_PLACEMENT_3D('',#19737,#16062,#16063);
#14394=AXIS2_PLACEMENT_3D('',#19749,#16065,#16066);
#14395=AXIS2_PLACEMENT_3D('',#19758,#16067,#16068);
#14396=AXIS2_PLACEMENT_3D('',#19760,#16070,#16071);
#14397=AXIS2_PLACEMENT_3D('',#19765,#16073,#16074);
#14398=AXIS2_PLACEMENT_3D('',#19769,#16076,#16077);
#14399=AXIS2_PLACEMENT_3D('',#19773,#16079,#16080);
#14400=AXIS2_PLACEMENT_3D('',#19777,#16082,#16083);
#14401=AXIS2_PLACEMENT_3D('',#19782,#16086,#16087);
#14402=AXIS2_PLACEMENT_3D('',#19787,#16090,#16091);
#14403=AXIS2_PLACEMENT_3D('',#19790,#16093,#16094);
#14404=AXIS2_PLACEMENT_3D('',#19792,#16095,#16096);
#14405=AXIS2_PLACEMENT_3D('',#19796,#16098,#16099);
#14406=AXIS2_PLACEMENT_3D('',#19800,#16102,#16103);
#14407=AXIS2_PLACEMENT_3D('',#19802,#16105,#16106);
#14408=AXIS2_PLACEMENT_3D('',#19809,#16110,#16111);
#14409=AXIS2_PLACEMENT_3D('',#19814,#16115,#16116);
#14410=AXIS2_PLACEMENT_3D('',#19818,#16119,#16120);
#14411=AXIS2_PLACEMENT_3D('',#19820,#16122,#16123);
#14412=AXIS2_PLACEMENT_3D('',#19826,#16127,#16128);
#14413=AXIS2_PLACEMENT_3D('',#19832,#16132,#16133);
#14414=AXIS2_PLACEMENT_3D('',#19836,#16136,#16137);
#14415=AXIS2_PLACEMENT_3D('',#19842,#16141,#16142);
#14416=AXIS2_PLACEMENT_3D('',#19845,#16145,#16146);
#14417=AXIS2_PLACEMENT_3D('',#19851,#16150,#16151);
#14418=AXIS2_PLACEMENT_3D('',#19853,#16153,#16154);
#14419=AXIS2_PLACEMENT_3D('',#19854,#16155,#16156);
#14420=AXIS2_PLACEMENT_3D('',#19856,#16158,#16159);
#14421=AXIS2_PLACEMENT_3D('',#19862,#16163,#16164);
#14422=AXIS2_PLACEMENT_3D('',#19863,#16165,#16166);
#14423=AXIS2_PLACEMENT_3D('',#19865,#16167,#16168);
#14424=AXIS2_PLACEMENT_3D('',#19867,#16170,#16171);
#14425=AXIS2_PLACEMENT_3D('',#19870,#16173,#16174);
#14426=AXIS2_PLACEMENT_3D('',#19871,#16175,#16176);
#14427=AXIS2_PLACEMENT_3D('',#19873,#16178,#16179);
#14428=AXIS2_PLACEMENT_3D('',#19874,#16180,#16181);
#14429=AXIS2_PLACEMENT_3D('',#19876,#16183,#16184);
#14430=AXIS2_PLACEMENT_3D('',#19878,#16186,#16187);
#14431=AXIS2_PLACEMENT_3D('',#19879,#16188,#16189);
#14432=AXIS2_PLACEMENT_3D('',#19880,#16190,#16191);
#14433=AXIS2_PLACEMENT_3D('',#19881,#16192,#16193);
#14434=AXIS2_PLACEMENT_3D('',#19883,#16194,#16195);
#14435=AXIS2_PLACEMENT_3D('',#19886,#16197,#16198);
#14436=AXIS2_PLACEMENT_3D('',#19887,#16199,#16200);
#14437=AXIS2_PLACEMENT_3D('',#19889,#16201,#16202);
#14438=AXIS2_PLACEMENT_3D('',#19892,#16204,#16205);
#14439=AXIS2_PLACEMENT_3D('',#19893,#16206,#16207);
#14440=AXIS2_PLACEMENT_3D('',#19894,#16208,#16209);
#14441=AXIS2_PLACEMENT_3D('',#19895,#16210,#16211);
#14442=AXIS2_PLACEMENT_3D('',#19896,#16212,#16213);
#14443=AXIS2_PLACEMENT_3D('',#19898,#16214,#16215);
#14444=AXIS2_PLACEMENT_3D('',#19901,#16217,#16218);
#14445=AXIS2_PLACEMENT_3D('',#19902,#16219,#16220);
#14446=AXIS2_PLACEMENT_3D('',#19903,#16221,#16222);
#14447=AXIS2_PLACEMENT_3D('',#19904,#16223,#16224);
#14448=AXIS2_PLACEMENT_3D('',#19905,#16225,#16226);
#14449=AXIS2_PLACEMENT_3D('',#19907,#16227,#16228);
#14450=AXIS2_PLACEMENT_3D('',#19910,#16230,#16231);
#14451=AXIS2_PLACEMENT_3D('',#19911,#16232,#16233);
#14452=AXIS2_PLACEMENT_3D('',#19912,#16234,#16235);
#14453=AXIS2_PLACEMENT_3D('',#19913,#16236,#16237);
#14454=AXIS2_PLACEMENT_3D('',#19914,#16238,#16239);
#14455=AXIS2_PLACEMENT_3D('',#19916,#16240,#16241);
#14456=AXIS2_PLACEMENT_3D('',#19919,#16243,#16244);
#14457=AXIS2_PLACEMENT_3D('',#19920,#16245,#16246);
#14458=AXIS2_PLACEMENT_3D('',#19922,#16247,#16248);
#14459=AXIS2_PLACEMENT_3D('',#19923,#16249,#16250);
#14460=AXIS2_PLACEMENT_3D('',#19925,#16251,#16252);
#14461=AXIS2_PLACEMENT_3D('',#19928,#16254,#16255);
#14462=AXIS2_PLACEMENT_3D('',#19929,#16256,#16257);
#14463=AXIS2_PLACEMENT_3D('',#19931,#16258,#16259);
#14464=AXIS2_PLACEMENT_3D('',#19932,#16260,#16261);
#14465=AXIS2_PLACEMENT_3D('',#19934,#16262,#16263);
#14466=AXIS2_PLACEMENT_3D('',#19937,#16265,#16266);
#14467=AXIS2_PLACEMENT_3D('',#19938,#16267,#16268);
#14468=AXIS2_PLACEMENT_3D('',#19940,#16269,#16270);
#14469=AXIS2_PLACEMENT_3D('',#19941,#16271,#16272);
#14470=AXIS2_PLACEMENT_3D('',#19943,#16273,#16274);
#14471=AXIS2_PLACEMENT_3D('',#19946,#16276,#16277);
#14472=AXIS2_PLACEMENT_3D('',#19947,#16278,#16279);
#14473=AXIS2_PLACEMENT_3D('',#19949,#16280,#16281);
#14474=AXIS2_PLACEMENT_3D('',#19950,#16282,#16283);
#14475=AXIS2_PLACEMENT_3D('',#19952,#16284,#16285);
#14476=AXIS2_PLACEMENT_3D('',#19954,#16287,#16288);
#14477=AXIS2_PLACEMENT_3D('',#19956,#16289,#16290);
#14478=AXIS2_PLACEMENT_3D('',#19958,#16292,#16293);
#14479=AXIS2_PLACEMENT_3D('',#19960,#16294,#16295);
#14480=AXIS2_PLACEMENT_3D('',#19962,#16297,#16298);
#14481=AXIS2_PLACEMENT_3D('',#19964,#16299,#16300);
#14482=AXIS2_PLACEMENT_3D('',#19966,#16302,#16303);
#14483=AXIS2_PLACEMENT_3D('',#19975,#16308,#16309);
#14484=AXIS2_PLACEMENT_3D('',#19981,#16313,#16314);
#14485=AXIS2_PLACEMENT_3D('',#19987,#16318,#16319);
#14486=AXIS2_PLACEMENT_3D('',#19993,#16323,#16324);
#14487=AXIS2_PLACEMENT_3D('',#19999,#16328,#16329);
#14488=AXIS2_PLACEMENT_3D('',#20005,#16333,#16334);
#14489=AXIS2_PLACEMENT_3D('',#20011,#16338,#16339);
#14490=AXIS2_PLACEMENT_3D('',#20017,#16343,#16344);
#14491=AXIS2_PLACEMENT_3D('',#20023,#16348,#16349);
#14492=AXIS2_PLACEMENT_3D('',#20029,#16353,#16354);
#14493=AXIS2_PLACEMENT_3D('',#20035,#16358,#16359);
#14494=AXIS2_PLACEMENT_3D('',#20038,#16362,#16363);
#14495=AXIS2_PLACEMENT_3D('',#20039,#16364,#16365);
#14496=AXIS2_PLACEMENT_3D('',#20040,#16366,#16367);
#14497=AXIS2_PLACEMENT_3D('',#20041,#16368,#16369);
#14498=AXIS2_PLACEMENT_3D('',#20042,#16370,#16371);
#14499=AXIS2_PLACEMENT_3D('',#20045,#16372,#16373);
#14500=AXIS2_PLACEMENT_3D('',#20046,#16374,#16375);
#14501=AXIS2_PLACEMENT_3D('',#20048,#16376,#16377);
#14502=AXIS2_PLACEMENT_3D('',#20050,#16378,#16379);
#14503=AXIS2_PLACEMENT_3D('',#20051,#16380,#16381);
#14504=AXIS2_PLACEMENT_3D('',#20052,#16382,#16383);
#14505=AXIS2_PLACEMENT_3D('',#20055,#16385,#16386);
#14506=AXIS2_PLACEMENT_3D('',#20056,#16387,#16388);
#14507=AXIS2_PLACEMENT_3D('',#20058,#16389,#16390);
#14508=AXIS2_PLACEMENT_3D('',#20061,#16392,#16393);
#14509=AXIS2_PLACEMENT_3D('',#20062,#16394,#16395);
#14510=AXIS2_PLACEMENT_3D('',#20065,#16397,#16398);
#14511=AXIS2_PLACEMENT_3D('',#20066,#16399,#16400);
#14512=AXIS2_PLACEMENT_3D('',#20067,#16401,#16402);
#14513=AXIS2_PLACEMENT_3D('',#20069,#16403,#16404);
#14514=AXIS2_PLACEMENT_3D('',#20071,#16406,#16407);
#14515=AXIS2_PLACEMENT_3D('',#20073,#16408,#16409);
#14516=AXIS2_PLACEMENT_3D('',#20074,#16410,#16411);
#14517=AXIS2_PLACEMENT_3D('',#20076,#16413,#16414);
#14518=AXIS2_PLACEMENT_3D('',#20077,#16415,#16416);
#14519=AXIS2_PLACEMENT_3D('',#20080,#16417,#16418);
#14520=AXIS2_PLACEMENT_3D('',#20081,#16419,#16420);
#14521=AXIS2_PLACEMENT_3D('',#20083,#16421,#16422);
#14522=AXIS2_PLACEMENT_3D('',#20085,#16423,#16424);
#14523=AXIS2_PLACEMENT_3D('',#20086,#16425,#16426);
#14524=AXIS2_PLACEMENT_3D('',#20087,#16427,#16428);
#14525=AXIS2_PLACEMENT_3D('',#20089,#16429,#16430);
#14526=AXIS2_PLACEMENT_3D('',#20091,#16432,#16433);
#14527=AXIS2_PLACEMENT_3D('',#20093,#16434,#16435);
#14528=AXIS2_PLACEMENT_3D('',#20095,#16436,#16437);
#14529=AXIS2_PLACEMENT_3D('',#20096,#16438,#16439);
#14530=AXIS2_PLACEMENT_3D('',#20098,#16440,#16441);
#14531=AXIS2_PLACEMENT_3D('',#20100,#16443,#16444);
#14532=AXIS2_PLACEMENT_3D('',#20102,#16445,#16446);
#14533=AXIS2_PLACEMENT_3D('',#20104,#16448,#16449);
#14534=AXIS2_PLACEMENT_3D('',#20106,#16450,#16451);
#14535=AXIS2_PLACEMENT_3D('',#20108,#16453,#16454);
#14536=AXIS2_PLACEMENT_3D('',#20109,#16455,#16456);
#14537=AXIS2_PLACEMENT_3D('',#20111,#16458,#16459);
#14538=AXIS2_PLACEMENT_3D('',#20112,#16460,#16461);
#14539=AXIS2_PLACEMENT_3D('',#20115,#16462,#16463);
#14540=AXIS2_PLACEMENT_3D('',#20116,#16464,#16465);
#14541=AXIS2_PLACEMENT_3D('',#20119,#16466,#16467);
#14542=AXIS2_PLACEMENT_3D('',#20120,#16468,#16469);
#14543=AXIS2_PLACEMENT_3D('',#20123,#16470,#16471);
#14544=AXIS2_PLACEMENT_3D('',#20124,#16472,#16473);
#14545=AXIS2_PLACEMENT_3D('',#20127,#16474,#16475);
#14546=AXIS2_PLACEMENT_3D('',#20128,#16476,#16477);
#14547=AXIS2_PLACEMENT_3D('',#20131,#16478,#16479);
#14548=AXIS2_PLACEMENT_3D('',#20132,#16480,#16481);
#14549=AXIS2_PLACEMENT_3D('',#20135,#16482,#16483);
#14550=AXIS2_PLACEMENT_3D('',#20136,#16484,#16485);
#14551=AXIS2_PLACEMENT_3D('',#20139,#16486,#16487);
#14552=AXIS2_PLACEMENT_3D('',#20140,#16488,#16489);
#14553=AXIS2_PLACEMENT_3D('',#20141,#16490,#16491);
#14554=AXIS2_PLACEMENT_3D('',#20167,#16492,#16493);
#14555=AXIS2_PLACEMENT_3D('',#20191,#16494,#16495);
#14556=AXIS2_PLACEMENT_3D('',#20192,#16496,#16497);
#14557=AXIS2_PLACEMENT_3D('',#20194,#16498,#16499);
#14558=AXIS2_PLACEMENT_3D('',#20219,#16500,#16501);
#14559=AXIS2_PLACEMENT_3D('',#20244,#16502,#16503);
#14560=AXIS2_PLACEMENT_3D('',#20247,#16505,#16506);
#14561=AXIS2_PLACEMENT_3D('',#20249,#16507,#16508);
#14562=AXIS2_PLACEMENT_3D('',#20274,#16509,#16510);
#14563=AXIS2_PLACEMENT_3D('',#20299,#16511,#16512);
#14564=AXIS2_PLACEMENT_3D('',#20324,#16513,#16514);
#14565=AXIS2_PLACEMENT_3D('',#20348,#16515,#16516);
#14566=AXIS2_PLACEMENT_3D('',#20349,#16517,#16518);
#14567=AXIS2_PLACEMENT_3D('',#20351,#16519,#16520);
#14568=AXIS2_PLACEMENT_3D('',#20352,#16521,#16522);
#14569=AXIS2_PLACEMENT_3D('',#20353,#16523,#16524);
#14570=AXIS2_PLACEMENT_3D('',#20377,#16525,#16526);
#14571=AXIS2_PLACEMENT_3D('',#20378,#16527,#16528);
#14572=AXIS2_PLACEMENT_3D('',#20380,#16529,#16530);
#14573=AXIS2_PLACEMENT_3D('',#20381,#16531,#16532);
#14574=AXIS2_PLACEMENT_3D('',#20382,#16533,#16534);
#14575=AXIS2_PLACEMENT_3D('',#20406,#16535,#16536);
#14576=AXIS2_PLACEMENT_3D('',#20407,#16537,#16538);
#14577=AXIS2_PLACEMENT_3D('',#20409,#16539,#16540);
#14578=AXIS2_PLACEMENT_3D('',#20411,#16541,#16542);
#14579=AXIS2_PLACEMENT_3D('',#20412,#16543,#16544);
#14580=AXIS2_PLACEMENT_3D('',#20413,#16545,#16546);
#14581=AXIS2_PLACEMENT_3D('',#20437,#16547,#16548);
#14582=AXIS2_PLACEMENT_3D('',#20438,#16549,#16550);
#14583=AXIS2_PLACEMENT_3D('',#20440,#16551,#16552);
#14584=AXIS2_PLACEMENT_3D('',#20441,#16553,#16554);
#14585=AXIS2_PLACEMENT_3D('',#20442,#16555,#16556);
#14586=AXIS2_PLACEMENT_3D('',#20466,#16557,#16558);
#14587=AXIS2_PLACEMENT_3D('',#20467,#16559,#16560);
#14588=AXIS2_PLACEMENT_3D('',#20469,#16561,#16562);
#14589=AXIS2_PLACEMENT_3D('',#20470,#16563,#16564);
#14590=AXIS2_PLACEMENT_3D('',#20471,#16565,#16566);
#14591=AXIS2_PLACEMENT_3D('',#20495,#16567,#16568);
#14592=AXIS2_PLACEMENT_3D('',#20496,#16569,#16570);
#14593=AXIS2_PLACEMENT_3D('',#20498,#16571,#16572);
#14594=AXIS2_PLACEMENT_3D('',#20501,#16574,#16575);
#14595=AXIS2_PLACEMENT_3D('',#20525,#16576,#16577);
#14596=AXIS2_PLACEMENT_3D('',#20526,#16578,#16579);
#14597=AXIS2_PLACEMENT_3D('',#20527,#16580,#16581);
#14598=AXIS2_PLACEMENT_3D('',#20528,#16582,#16583);
#14599=AXIS2_PLACEMENT_3D('',#20529,#16584,#16585);
#14600=AXIS2_PLACEMENT_3D('',#20530,#16586,#16587);
#14601=AXIS2_PLACEMENT_3D('',#20531,#16588,#16589);
#14602=AXIS2_PLACEMENT_3D('',#20532,#16590,#16591);
#14603=AXIS2_PLACEMENT_3D('',#20533,#16592,#16593);
#14604=AXIS2_PLACEMENT_3D('',#20535,#16594,#16595);
#14605=AXIS2_PLACEMENT_3D('',#20537,#16596,#16597);
#14606=AXIS2_PLACEMENT_3D('',#20538,#16598,#16599);
#14607=AXIS2_PLACEMENT_3D('',#20540,#16600,#16601);
#14608=AXIS2_PLACEMENT_3D('',#20542,#16603,#16604);
#14609=AXIS2_PLACEMENT_3D('',#20544,#16605,#16606);
#14610=AXIS2_PLACEMENT_3D('',#20545,#16607,#16608);
#14611=AXIS2_PLACEMENT_3D('',#20547,#16610,#16611);
#14612=AXIS2_PLACEMENT_3D('',#20549,#16612,#16613);
#14613=AXIS2_PLACEMENT_3D('',#20551,#16614,#16615);
#14614=AXIS2_PLACEMENT_3D('',#20552,#16616,#16617);
#14615=AXIS2_PLACEMENT_3D('',#20554,#16618,#16619);
#14616=AXIS2_PLACEMENT_3D('',#20556,#16621,#16622);
#14617=AXIS2_PLACEMENT_3D('',#20558,#16623,#16624);
#14618=AXIS2_PLACEMENT_3D('',#20559,#16625,#16626);
#14619=AXIS2_PLACEMENT_3D('',#20561,#16628,#16629);
#14620=AXIS2_PLACEMENT_3D('',#20562,#16630,#16631);
#14621=AXIS2_PLACEMENT_3D('',#20563,#16632,#16633);
#14622=AXIS2_PLACEMENT_3D('',#20564,#16634,#16635);
#14623=AXIS2_PLACEMENT_3D('',#20565,#16636,#16637);
#14624=AXIS2_PLACEMENT_3D('',#20566,#16638,#16639);
#14625=AXIS2_PLACEMENT_3D('',#20567,#16640,#16641);
#14626=AXIS2_PLACEMENT_3D('',#20569,#16642,#16643);
#14627=AXIS2_PLACEMENT_3D('',#20570,#16644,#16645);
#14628=AXIS2_PLACEMENT_3D('',#20572,#16646,#16647);
#14629=AXIS2_PLACEMENT_3D('',#20574,#16649,#16650);
#14630=AXIS2_PLACEMENT_3D('',#20576,#16651,#16652);
#14631=AXIS2_PLACEMENT_3D('',#20578,#16654,#16655);
#14632=AXIS2_PLACEMENT_3D('',#20580,#16656,#16657);
#14633=AXIS2_PLACEMENT_3D('',#20582,#16659,#16660);
#14634=AXIS2_PLACEMENT_3D('',#20584,#16661,#16662);
#14635=AXIS2_PLACEMENT_3D('',#20585,#16663,#16664);
#14636=AXIS2_PLACEMENT_3D('',#20587,#16665,#16666);
#14637=AXIS2_PLACEMENT_3D('',#20589,#16668,#16669);
#14638=AXIS2_PLACEMENT_3D('',#20591,#16670,#16671);
#14639=AXIS2_PLACEMENT_3D('',#20593,#16673,#16674);
#14640=AXIS2_PLACEMENT_3D('',#20595,#16675,#16676);
#14641=AXIS2_PLACEMENT_3D('',#20597,#16678,#16679);
#14642=AXIS2_PLACEMENT_3D('',#20598,#16680,#16681);
#14643=AXIS2_PLACEMENT_3D('',#20607,#16686,#16687);
#14644=AXIS2_PLACEMENT_3D('',#20613,#16691,#16692);
#14645=AXIS2_PLACEMENT_3D('',#20619,#16696,#16697);
#14646=AXIS2_PLACEMENT_3D('',#20625,#16701,#16702);
#14647=AXIS2_PLACEMENT_3D('',#20631,#16706,#16707);
#14648=AXIS2_PLACEMENT_3D('',#20634,#16710,#16711);
#14649=AXIS2_PLACEMENT_3D('',#20635,#16712,#16713);
#14650=AXIS2_PLACEMENT_3D('',#20636,#16714,#16715);
#14651=AXIS2_PLACEMENT_3D('',#20637,#16716,#16717);
#14652=AXIS2_PLACEMENT_3D('',#20638,#16718,#16719);
#14653=AXIS2_PLACEMENT_3D('',#20640,#16720,#16721);
#14654=AXIS2_PLACEMENT_3D('',#20643,#16723,#16724);
#14655=AXIS2_PLACEMENT_3D('',#20644,#16725,#16726);
#14656=AXIS2_PLACEMENT_3D('',#20646,#16727,#16728);
#14657=AXIS2_PLACEMENT_3D('',#20649,#16730,#16731);
#14658=AXIS2_PLACEMENT_3D('',#20650,#16732,#16733);
#14659=AXIS2_PLACEMENT_3D('',#20652,#16734,#16735);
#14660=AXIS2_PLACEMENT_3D('',#20655,#16737,#16738);
#14661=AXIS2_PLACEMENT_3D('',#20656,#16739,#16740);
#14662=AXIS2_PLACEMENT_3D('',#20658,#16741,#16742);
#14663=AXIS2_PLACEMENT_3D('',#20661,#16744,#16745);
#14664=AXIS2_PLACEMENT_3D('',#20662,#16746,#16747);
#14665=AXIS2_PLACEMENT_3D('',#20664,#16748,#16749);
#14666=AXIS2_PLACEMENT_3D('',#20667,#16751,#16752);
#14667=AXIS2_PLACEMENT_3D('',#20668,#16753,#16754);
#14668=AXIS2_PLACEMENT_3D('',#20677,#16759,#16760);
#14669=AXIS2_PLACEMENT_3D('',#20683,#16764,#16765);
#14670=AXIS2_PLACEMENT_3D('',#20689,#16769,#16770);
#14671=AXIS2_PLACEMENT_3D('',#20692,#16773,#16774);
#14672=AXIS2_PLACEMENT_3D('',#20693,#16775,#16776);
#14673=AXIS2_PLACEMENT_3D('',#20695,#16777,#16778);
#14674=AXIS2_PLACEMENT_3D('',#20698,#16780,#16781);
#14675=AXIS2_PLACEMENT_3D('',#20699,#16782,#16783);
#14676=AXIS2_PLACEMENT_3D('',#20701,#16784,#16785);
#14677=AXIS2_PLACEMENT_3D('',#20704,#16787,#16788);
#14678=AXIS2_PLACEMENT_3D('',#20705,#16789,#16790);
#14679=AXIS2_PLACEMENT_3D('',#20707,#16791,#16792);
#14680=AXIS2_PLACEMENT_3D('',#20710,#16794,#16795);
#14681=AXIS2_PLACEMENT_3D('',#20711,#16796,#16797);
#14682=AXIS2_PLACEMENT_3D('',#20713,#16798,#16799);
#14683=AXIS2_PLACEMENT_3D('',#20716,#16801,#16802);
#14684=AXIS2_PLACEMENT_3D('',#20717,#16803,#16804);
#14685=AXIS2_PLACEMENT_3D('',#20722,#16806,#16807);
#14686=AXIS2_PLACEMENT_3D('',#20725,#16809,#16810);
#14687=AXIS2_PLACEMENT_3D('',#20726,#16811,#16812);
#14688=AXIS2_PLACEMENT_3D('',#20736,#16818,#16819);
#14689=AXIS2_PLACEMENT_3D('',#20740,#16822,#16823);
#14690=AXIS2_PLACEMENT_3D('',#20744,#16826,#16827);
#14691=AXIS2_PLACEMENT_3D('',#20748,#16830,#16831);
#14692=AXIS2_PLACEMENT_3D('',#20752,#16834,#16835);
#14693=AXIS2_PLACEMENT_3D('',#20754,#16837,#16838);
#14694=AXIS2_PLACEMENT_3D('',#20755,#16839,#16840);
#14695=AXIS2_PLACEMENT_3D('',#20756,#16841,#16842);
#14696=AXIS2_PLACEMENT_3D('',#20765,#16847,#16848);
#14697=AXIS2_PLACEMENT_3D('',#20771,#16852,#16853);
#14698=AXIS2_PLACEMENT_3D('',#20777,#16857,#16858);
#14699=AXIS2_PLACEMENT_3D('',#20780,#16861,#16862);
#14700=AXIS2_PLACEMENT_3D('',#20781,#16863,#16864);
#14701=AXIS2_PLACEMENT_3D('',#20782,#16865,#16866);
#14702=AXIS2_PLACEMENT_3D('',#20783,#16867,#16868);
#14703=AXIS2_PLACEMENT_3D('',#20861,#16870,#16871);
#14704=AXIS2_PLACEMENT_3D('',#20863,#16872,#16873);
#14705=AXIS2_PLACEMENT_3D('',#20866,#16875,#16876);
#14706=AXIS2_PLACEMENT_3D('',#20867,#16877,#16878);
#14707=AXIS2_PLACEMENT_3D('',#20868,#16879,#16880);
#14708=AXIS2_PLACEMENT_3D('',#20870,#16881,#16882);
#14709=AXIS2_PLACEMENT_3D('',#20873,#16884,#16885);
#14710=AXIS2_PLACEMENT_3D('',#20874,#16886,#16887);
#14711=AXIS2_PLACEMENT_3D('',#20875,#16888,#16889);
#14712=AXIS2_PLACEMENT_3D('',#20877,#16890,#16891);
#14713=AXIS2_PLACEMENT_3D('',#20880,#16893,#16894);
#14714=AXIS2_PLACEMENT_3D('',#20881,#16895,#16896);
#14715=AXIS2_PLACEMENT_3D('',#20882,#16897,#16898);
#14716=AXIS2_PLACEMENT_3D('',#20884,#16899,#16900);
#14717=AXIS2_PLACEMENT_3D('',#20887,#16902,#16903);
#14718=AXIS2_PLACEMENT_3D('',#20888,#16904,#16905);
#14719=AXIS2_PLACEMENT_3D('',#20889,#16906,#16907);
#14720=AXIS2_PLACEMENT_3D('',#20894,#16909,#16910);
#14721=AXIS2_PLACEMENT_3D('',#20897,#16912,#16913);
#14722=AXIS2_PLACEMENT_3D('',#20898,#16914,#16915);
#14723=AXIS2_PLACEMENT_3D('',#20899,#16916,#16917);
#14724=AXIS2_PLACEMENT_3D('',#20900,#16918,#16919);
#14725=AXIS2_PLACEMENT_3D('',#20905,#16921,#16922);
#14726=AXIS2_PLACEMENT_3D('',#20908,#16924,#16925);
#14727=AXIS2_PLACEMENT_3D('',#20909,#16926,#16927);
#14728=AXIS2_PLACEMENT_3D('',#20910,#16928,#16929);
#14729=AXIS2_PLACEMENT_3D('',#20911,#16930,#16931);
#14730=AXIS2_PLACEMENT_3D('',#20916,#16933,#16934);
#14731=AXIS2_PLACEMENT_3D('',#20919,#16936,#16937);
#14732=AXIS2_PLACEMENT_3D('',#20920,#16938,#16939);
#14733=AXIS2_PLACEMENT_3D('',#20921,#16940,#16941);
#14734=AXIS2_PLACEMENT_3D('',#20922,#16942,#16943);
#14735=AXIS2_PLACEMENT_3D('',#20927,#16945,#16946);
#14736=AXIS2_PLACEMENT_3D('',#20930,#16948,#16949);
#14737=AXIS2_PLACEMENT_3D('',#20931,#16950,#16951);
#14738=AXIS2_PLACEMENT_3D('',#20932,#16952,#16953);
#14739=AXIS2_PLACEMENT_3D('',#20933,#16954,#16955);
#14740=AXIS2_PLACEMENT_3D('',#20935,#16956,#16957);
#14741=AXIS2_PLACEMENT_3D('',#20938,#16959,#16960);
#14742=AXIS2_PLACEMENT_3D('',#20939,#16961,#16962);
#14743=AXIS2_PLACEMENT_3D('',#20941,#16963,#16964);
#14744=AXIS2_PLACEMENT_3D('',#20943,#16965,#16966);
#14745=AXIS2_PLACEMENT_3D('',#20944,#16967,#16968);
#14746=AXIS2_PLACEMENT_3D('',#20945,#16969,#16970);
#14747=AXIS2_PLACEMENT_3D('',#20946,#16971,#16972);
#14748=AXIS2_PLACEMENT_3D('',#20947,#16973,#16974);
#14749=AXIS2_PLACEMENT_3D('',#20949,#16975,#16976);
#14750=AXIS2_PLACEMENT_3D('',#20951,#16977,#16978);
#14751=AXIS2_PLACEMENT_3D('',#20953,#16979,#16980);
#14752=AXIS2_PLACEMENT_3D('',#20954,#16981,#16982);
#14753=AXIS2_PLACEMENT_3D('',#20956,#16983,#16984);
#14754=AXIS2_PLACEMENT_3D('',#20958,#16986,#16987);
#14755=AXIS2_PLACEMENT_3D('',#20960,#16988,#16989);
#14756=AXIS2_PLACEMENT_3D('',#20962,#16991,#16992);
#14757=AXIS2_PLACEMENT_3D('',#20964,#16993,#16994);
#14758=AXIS2_PLACEMENT_3D('',#20966,#16996,#16997);
#14759=AXIS2_PLACEMENT_3D('',#20968,#16998,#16999);
#14760=AXIS2_PLACEMENT_3D('',#20970,#17001,#17002);
#14761=AXIS2_PLACEMENT_3D('',#20972,#17003,#17004);
#14762=AXIS2_PLACEMENT_3D('',#20975,#17006,#17007);
#14763=AXIS2_PLACEMENT_3D('',#20976,#17008,#17009);
#14764=AXIS2_PLACEMENT_3D('',#20978,#17010,#17011);
#14765=AXIS2_PLACEMENT_3D('',#20979,#17012,#17013);
#14766=AXIS2_PLACEMENT_3D('',#20982,#17015,#17016);
#14767=AXIS2_PLACEMENT_3D('',#20983,#17017,#17018);
#14768=AXIS2_PLACEMENT_3D('',#20986,#17020,#17021);
#14769=AXIS2_PLACEMENT_3D('',#20987,#17022,#17023);
#14770=AXIS2_PLACEMENT_3D('',#20988,#17024,#17025);
#14771=AXIS2_PLACEMENT_3D('',#20989,#17026,#17027);
#14772=AXIS2_PLACEMENT_3D('',#20990,#17028,#17029);
#14773=AXIS2_PLACEMENT_3D('',#20992,#17030,#17031);
#14774=AXIS2_PLACEMENT_3D('',#20995,#17033,#17034);
#14775=AXIS2_PLACEMENT_3D('',#20996,#17035,#17036);
#14776=AXIS2_PLACEMENT_3D('',#20998,#17037,#17038);
#14777=AXIS2_PLACEMENT_3D('',#21001,#17040,#17041);
#14778=AXIS2_PLACEMENT_3D('',#21002,#17042,#17043);
#14779=AXIS2_PLACEMENT_3D('',#21003,#17044,#17045);
#14780=AXIS2_PLACEMENT_3D('',#21004,#17046,#17047);
#14781=AXIS2_PLACEMENT_3D('',#21005,#17048,#17049);
#14782=AXIS2_PLACEMENT_3D('',#21007,#17050,#17051);
#14783=AXIS2_PLACEMENT_3D('',#21010,#17053,#17054);
#14784=AXIS2_PLACEMENT_3D('',#21011,#17055,#17056);
#14785=AXIS2_PLACEMENT_3D('',#21013,#17057,#17058);
#14786=AXIS2_PLACEMENT_3D('',#21016,#17060,#17061);
#14787=AXIS2_PLACEMENT_3D('',#21017,#17062,#17063);
#14788=AXIS2_PLACEMENT_3D('',#21019,#17064,#17065);
#14789=AXIS2_PLACEMENT_3D('',#21022,#17067,#17068);
#14790=AXIS2_PLACEMENT_3D('',#21023,#17069,#17070);
#14791=AXIS2_PLACEMENT_3D('',#21025,#17071,#17072);
#14792=AXIS2_PLACEMENT_3D('',#21028,#17074,#17075);
#14793=AXIS2_PLACEMENT_3D('',#21029,#17076,#17077);
#14794=AXIS2_PLACEMENT_3D('',#21031,#17078,#17079);
#14795=AXIS2_PLACEMENT_3D('',#21034,#17081,#17082);
#14796=AXIS2_PLACEMENT_3D('',#21035,#17083,#17084);
#14797=AXIS2_PLACEMENT_3D('',#21037,#17085,#17086);
#14798=AXIS2_PLACEMENT_3D('',#21040,#17088,#17089);
#14799=AXIS2_PLACEMENT_3D('',#21041,#17090,#17091);
#14800=AXIS2_PLACEMENT_3D('',#21042,#17092,#17093);
#14801=AXIS2_PLACEMENT_3D('',#21043,#17094,#17095);
#14802=AXIS2_PLACEMENT_3D('',#21044,#17096,#17097);
#14803=AXIS2_PLACEMENT_3D('',#21045,#17098,#17099);
#14804=AXIS2_PLACEMENT_3D('',#21049,#17101,#17102);
#14805=AXIS2_PLACEMENT_3D('',#21050,#17103,#17104);
#14806=AXIS2_PLACEMENT_3D('',#21054,#17106,#17107);
#14807=AXIS2_PLACEMENT_3D('',#21057,#17109,#17110);
#14808=AXIS2_PLACEMENT_3D('',#21059,#17111,#17112);
#14809=AXIS2_PLACEMENT_3D('',#21061,#17114,#17115);
#14810=AXIS2_PLACEMENT_3D('',#21065,#17117,#17118);
#14811=AXIS2_PLACEMENT_3D('',#21066,#17119,#17120);
#14812=AXIS2_PLACEMENT_3D('',#21070,#17122,#17123);
#14813=AXIS2_PLACEMENT_3D('',#21073,#17125,#17126);
#14814=AXIS2_PLACEMENT_3D('',#21075,#17127,#17128);
#14815=AXIS2_PLACEMENT_3D('',#21077,#17130,#17131);
#14816=AXIS2_PLACEMENT_3D('',#21081,#17133,#17134);
#14817=AXIS2_PLACEMENT_3D('',#21082,#17135,#17136);
#14818=AXIS2_PLACEMENT_3D('',#21086,#17138,#17139);
#14819=AXIS2_PLACEMENT_3D('',#21089,#17141,#17142);
#14820=AXIS2_PLACEMENT_3D('',#21091,#17143,#17144);
#14821=AXIS2_PLACEMENT_3D('',#21093,#17146,#17147);
#14822=AXIS2_PLACEMENT_3D('',#21097,#17149,#17150);
#14823=AXIS2_PLACEMENT_3D('',#21098,#17151,#17152);
#14824=AXIS2_PLACEMENT_3D('',#21102,#17154,#17155);
#14825=AXIS2_PLACEMENT_3D('',#21105,#17157,#17158);
#14826=AXIS2_PLACEMENT_3D('',#21107,#17159,#17160);
#14827=AXIS2_PLACEMENT_3D('',#21109,#17162,#17163);
#14828=AXIS2_PLACEMENT_3D('',#21120,#17170,#17171);
#14829=AXIS2_PLACEMENT_3D('',#21131,#17178,#17179);
#14830=AXIS2_PLACEMENT_3D('',#21150,#17190,#17191);
#14831=AXIS2_PLACEMENT_3D('',#21154,#17194,#17195);
#14832=AXIS2_PLACEMENT_3D('',#21158,#17198,#17199);
#14833=AXIS2_PLACEMENT_3D('',#21162,#17202,#17203);
#14834=AXIS2_PLACEMENT_3D('',#21166,#17206,#17207);
#14835=AXIS2_PLACEMENT_3D('',#21168,#17209,#17210);
#14836=AXIS2_PLACEMENT_3D('',#21172,#17213,#17214);
#14837=AXIS2_PLACEMENT_3D('',#21176,#17217,#17218);
#14838=AXIS2_PLACEMENT_3D('',#21180,#17221,#17222);
#14839=AXIS2_PLACEMENT_3D('',#21184,#17225,#17226);
#14840=AXIS2_PLACEMENT_3D('',#21186,#17228,#17229);
#14841=AXIS2_PLACEMENT_3D('',#21187,#17230,#17231);
#14842=AXIS2_PLACEMENT_3D('',#21188,#17232,#17233);
#14843=AXIS2_PLACEMENT_3D('',#21197,#17238,#17239);
#14844=AXIS2_PLACEMENT_3D('',#21203,#17243,#17244);
#14845=AXIS2_PLACEMENT_3D('',#21209,#17248,#17249);
#14846=AXIS2_PLACEMENT_3D('',#21215,#17253,#17254);
#14847=AXIS2_PLACEMENT_3D('',#21221,#17258,#17259);
#14848=AXIS2_PLACEMENT_3D('',#21227,#17263,#17264);
#14849=AXIS2_PLACEMENT_3D('',#21233,#17268,#17269);
#14850=AXIS2_PLACEMENT_3D('',#21236,#17272,#17273);
#14851=AXIS2_PLACEMENT_3D('',#21237,#17274,#17275);
#14852=AXIS2_PLACEMENT_3D('',#21238,#17276,#17277);
#14853=AXIS2_PLACEMENT_3D('',#21239,#17278,#17279);
#14854=AXIS2_PLACEMENT_3D('',#21248,#17284,#17285);
#14855=AXIS2_PLACEMENT_3D('',#21254,#17289,#17290);
#14856=AXIS2_PLACEMENT_3D('',#21260,#17294,#17295);
#14857=AXIS2_PLACEMENT_3D('',#21266,#17299,#17300);
#14858=AXIS2_PLACEMENT_3D('',#21272,#17304,#17305);
#14859=AXIS2_PLACEMENT_3D('',#21278,#17309,#17310);
#14860=AXIS2_PLACEMENT_3D('',#21284,#17314,#17315);
#14861=AXIS2_PLACEMENT_3D('',#21287,#17318,#17319);
#14862=AXIS2_PLACEMENT_3D('',#21288,#17320,#17321);
#14863=AXIS2_PLACEMENT_3D('',#21289,#17322,#17323);
#14864=AXIS2_PLACEMENT_3D('',#21290,#17324,#17325);
#14865=AXIS2_PLACEMENT_3D('',#21291,#17326,#17327);
#14866=AXIS2_PLACEMENT_3D('',#21292,#17328,#17329);
#14867=AXIS2_PLACEMENT_3D('',#21293,#17330,#17331);
#14868=AXIS2_PLACEMENT_3D('',#21302,#17336,#17337);
#14869=AXIS2_PLACEMENT_3D('',#21308,#17341,#17342);
#14870=AXIS2_PLACEMENT_3D('',#21314,#17346,#17347);
#14871=AXIS2_PLACEMENT_3D('',#21320,#17351,#17352);
#14872=AXIS2_PLACEMENT_3D('',#21326,#17356,#17357);
#14873=AXIS2_PLACEMENT_3D('',#21329,#17360,#17361);
#14874=AXIS2_PLACEMENT_3D('',#21330,#17362,#17363);
#14875=AXIS2_PLACEMENT_3D('',#21332,#17364,#17365);
#14876=AXIS2_PLACEMENT_3D('',#21333,#17366,#17367);
#14877=AXIS2_PLACEMENT_3D('',#21335,#17368,#17369);
#14878=AXIS2_PLACEMENT_3D('',#21337,#17371,#17372);
#14879=AXIS2_PLACEMENT_3D('',#21339,#17373,#17374);
#14880=AXIS2_PLACEMENT_3D('',#21341,#17376,#17377);
#14881=AXIS2_PLACEMENT_3D('',#21343,#17378,#17379);
#14882=AXIS2_PLACEMENT_3D('',#21345,#17381,#17382);
#14883=AXIS2_PLACEMENT_3D('',#21346,#17383,#17384);
#14884=AXIS2_PLACEMENT_3D('',#21347,#17385,#17386);
#14885=AXIS2_PLACEMENT_3D('',#21356,#17391,#17392);
#14886=AXIS2_PLACEMENT_3D('',#21362,#17396,#17397);
#14887=AXIS2_PLACEMENT_3D('',#21368,#17401,#17402);
#14888=AXIS2_PLACEMENT_3D('',#21374,#17406,#17407);
#14889=AXIS2_PLACEMENT_3D('',#21380,#17411,#17412);
#14890=AXIS2_PLACEMENT_3D('',#21383,#17415,#17416);
#14891=AXIS2_PLACEMENT_3D('',#21384,#17417,#17418);
#14892=AXIS2_PLACEMENT_3D('',#21385,#17419,#17420);
#14893=AXIS2_PLACEMENT_3D('',#21387,#17421,#17422);
#14894=AXIS2_PLACEMENT_3D('',#21388,#17423,#17424);
#14895=AXIS2_PLACEMENT_3D('',#21390,#17425,#17426);
#14896=AXIS2_PLACEMENT_3D('',#21391,#17427,#17428);
#14897=AXIS2_PLACEMENT_3D('',#21393,#17429,#17430);
#14898=AXIS2_PLACEMENT_3D('',#21395,#17432,#17433);
#14899=AXIS2_PLACEMENT_3D('',#21397,#17434,#17435);
#14900=AXIS2_PLACEMENT_3D('',#21399,#17437,#17438);
#14901=AXIS2_PLACEMENT_3D('',#21401,#17439,#17440);
#14902=AXIS2_PLACEMENT_3D('',#21403,#17442,#17443);
#14903=AXIS2_PLACEMENT_3D('',#21405,#17444,#17445);
#14904=AXIS2_PLACEMENT_3D('',#21406,#17446,#17447);
#14905=AXIS2_PLACEMENT_3D('',#21408,#17448,#17449);
#14906=AXIS2_PLACEMENT_3D('',#21410,#17451,#17452);
#14907=AXIS2_PLACEMENT_3D('',#21412,#17454,#17455);
#14908=AXIS2_PLACEMENT_3D('',#21413,#17456,#17457);
#14909=AXIS2_PLACEMENT_3D('',#21414,#17458,#17459);
#14910=AXIS2_PLACEMENT_3D('',#21417,#17460,#17461);
#14911=AXIS2_PLACEMENT_3D('',#21418,#17462,#17463);
#14912=AXIS2_PLACEMENT_3D('',#21420,#17464,#17465);
#14913=AXIS2_PLACEMENT_3D('',#21422,#17466,#17467);
#14914=AXIS2_PLACEMENT_3D('',#21423,#17468,#17469);
#14915=AXIS2_PLACEMENT_3D('',#21424,#17470,#17471);
#14916=AXIS2_PLACEMENT_3D('',#21427,#17473,#17474);
#14917=AXIS2_PLACEMENT_3D('',#21428,#17475,#17476);
#14918=AXIS2_PLACEMENT_3D('',#21430,#17477,#17478);
#14919=AXIS2_PLACEMENT_3D('',#21433,#17480,#17481);
#14920=AXIS2_PLACEMENT_3D('',#21434,#17482,#17483);
#14921=AXIS2_PLACEMENT_3D('',#21437,#17485,#17486);
#14922=AXIS2_PLACEMENT_3D('',#21438,#17487,#17488);
#14923=AXIS2_PLACEMENT_3D('',#21439,#17489,#17490);
#14924=AXIS2_PLACEMENT_3D('',#21441,#17491,#17492);
#14925=AXIS2_PLACEMENT_3D('',#21443,#17494,#17495);
#14926=AXIS2_PLACEMENT_3D('',#21445,#17496,#17497);
#14927=AXIS2_PLACEMENT_3D('',#21446,#17498,#17499);
#14928=AXIS2_PLACEMENT_3D('',#21448,#17501,#17502);
#14929=AXIS2_PLACEMENT_3D('',#21449,#17503,#17504);
#14930=AXIS2_PLACEMENT_3D('',#21452,#17505,#17506);
#14931=AXIS2_PLACEMENT_3D('',#21453,#17507,#17508);
#14932=AXIS2_PLACEMENT_3D('',#21455,#17509,#17510);
#14933=AXIS2_PLACEMENT_3D('',#21457,#17511,#17512);
#14934=AXIS2_PLACEMENT_3D('',#21458,#17513,#17514);
#14935=AXIS2_PLACEMENT_3D('',#21459,#17515,#17516);
#14936=AXIS2_PLACEMENT_3D('',#21461,#17517,#17518);
#14937=AXIS2_PLACEMENT_3D('',#21463,#17520,#17521);
#14938=AXIS2_PLACEMENT_3D('',#21465,#17522,#17523);
#14939=AXIS2_PLACEMENT_3D('',#21467,#17524,#17525);
#14940=AXIS2_PLACEMENT_3D('',#21468,#17526,#17527);
#14941=AXIS2_PLACEMENT_3D('',#21470,#17528,#17529);
#14942=AXIS2_PLACEMENT_3D('',#21472,#17531,#17532);
#14943=AXIS2_PLACEMENT_3D('',#21474,#17533,#17534);
#14944=AXIS2_PLACEMENT_3D('',#21476,#17536,#17537);
#14945=AXIS2_PLACEMENT_3D('',#21478,#17538,#17539);
#14946=AXIS2_PLACEMENT_3D('',#21480,#17541,#17542);
#14947=AXIS2_PLACEMENT_3D('',#21481,#17543,#17544);
#14948=AXIS2_PLACEMENT_3D('',#21483,#17546,#17547);
#14949=AXIS2_PLACEMENT_3D('',#21484,#17548,#17549);
#14950=AXIS2_PLACEMENT_3D('',#21487,#17550,#17551);
#14951=AXIS2_PLACEMENT_3D('',#21488,#17552,#17553);
#14952=AXIS2_PLACEMENT_3D('',#21491,#17554,#17555);
#14953=AXIS2_PLACEMENT_3D('',#21492,#17556,#17557);
#14954=AXIS2_PLACEMENT_3D('',#21495,#17558,#17559);
#14955=AXIS2_PLACEMENT_3D('',#21496,#17560,#17561);
#14956=AXIS2_PLACEMENT_3D('',#21499,#17562,#17563);
#14957=AXIS2_PLACEMENT_3D('',#21500,#17564,#17565);
#14958=AXIS2_PLACEMENT_3D('',#21503,#17566,#17567);
#14959=AXIS2_PLACEMENT_3D('',#21504,#17568,#17569);
#14960=AXIS2_PLACEMENT_3D('',#21507,#17570,#17571);
#14961=AXIS2_PLACEMENT_3D('',#21508,#17572,#17573);
#14962=AXIS2_PLACEMENT_3D('',#21511,#17574,#17575);
#14963=AXIS2_PLACEMENT_3D('',#21512,#17576,#17577);
#14964=AXIS2_PLACEMENT_3D('',#21515,#17578,#17579);
#14965=AXIS2_PLACEMENT_3D('',#21516,#17580,#17581);
#14966=AXIS2_PLACEMENT_3D('',#21517,#17582,#17583);
#14967=AXIS2_PLACEMENT_3D('',#21543,#17584,#17585);
#14968=AXIS2_PLACEMENT_3D('',#21567,#17586,#17587);
#14969=AXIS2_PLACEMENT_3D('',#21568,#17588,#17589);
#14970=AXIS2_PLACEMENT_3D('',#21570,#17590,#17591);
#14971=AXIS2_PLACEMENT_3D('',#21595,#17592,#17593);
#14972=AXIS2_PLACEMENT_3D('',#21620,#17594,#17595);
#14973=AXIS2_PLACEMENT_3D('',#21636,#17597,#17598);
#14974=AXIS2_PLACEMENT_3D('',#21651,#17599,#17600);
#14975=AXIS2_PLACEMENT_3D('',#21676,#17601,#17602);
#14976=AXIS2_PLACEMENT_3D('',#21701,#17603,#17604);
#14977=AXIS2_PLACEMENT_3D('',#21726,#17605,#17606);
#14978=AXIS2_PLACEMENT_3D('',#21750,#17607,#17608);
#14979=AXIS2_PLACEMENT_3D('',#21751,#17609,#17610);
#14980=AXIS2_PLACEMENT_3D('',#21753,#17611,#17612);
#14981=AXIS2_PLACEMENT_3D('',#21754,#17613,#17614);
#14982=AXIS2_PLACEMENT_3D('',#21755,#17615,#17616);
#14983=AXIS2_PLACEMENT_3D('',#21779,#17617,#17618);
#14984=AXIS2_PLACEMENT_3D('',#21780,#17619,#17620);
#14985=AXIS2_PLACEMENT_3D('',#21782,#17621,#17622);
#14986=AXIS2_PLACEMENT_3D('',#21783,#17623,#17624);
#14987=AXIS2_PLACEMENT_3D('',#21784,#17625,#17626);
#14988=AXIS2_PLACEMENT_3D('',#21808,#17627,#17628);
#14989=AXIS2_PLACEMENT_3D('',#21809,#17629,#17630);
#14990=AXIS2_PLACEMENT_3D('',#21811,#17631,#17632);
#14991=AXIS2_PLACEMENT_3D('',#21812,#17633,#17634);
#14992=AXIS2_PLACEMENT_3D('',#21813,#17635,#17636);
#14993=AXIS2_PLACEMENT_3D('',#21828,#17637,#17638);
#14994=AXIS2_PLACEMENT_3D('',#21841,#17639,#17640);
#14995=AXIS2_PLACEMENT_3D('',#21843,#17641,#17642);
#14996=AXIS2_PLACEMENT_3D('',#21844,#17643,#17644);
#14997=AXIS2_PLACEMENT_3D('',#21845,#17645,#17646);
#14998=AXIS2_PLACEMENT_3D('',#21869,#17647,#17648);
#14999=AXIS2_PLACEMENT_3D('',#21870,#17649,#17650);
#15000=AXIS2_PLACEMENT_3D('',#21872,#17651,#17652);
#15001=AXIS2_PLACEMENT_3D('',#21873,#17653,#17654);
#15002=AXIS2_PLACEMENT_3D('',#21874,#17655,#17656);
#15003=AXIS2_PLACEMENT_3D('',#21898,#17657,#17658);
#15004=AXIS2_PLACEMENT_3D('',#21899,#17659,#17660);
#15005=AXIS2_PLACEMENT_3D('',#21901,#17661,#17662);
#15006=AXIS2_PLACEMENT_3D('',#21902,#17663,#17664);
#15007=AXIS2_PLACEMENT_3D('',#21903,#17665,#17666);
#15008=AXIS2_PLACEMENT_3D('',#21927,#17667,#17668);
#15009=AXIS2_PLACEMENT_3D('',#21928,#17669,#17670);
#15010=AXIS2_PLACEMENT_3D('',#21930,#17671,#17672);
#15011=AXIS2_PLACEMENT_3D('',#21933,#17674,#17675);
#15012=AXIS2_PLACEMENT_3D('',#21957,#17676,#17677);
#15013=AXIS2_PLACEMENT_3D('',#21958,#17678,#17679);
#15014=AXIS2_PLACEMENT_3D('',#21959,#17680,#17681);
#15015=AXIS2_PLACEMENT_3D('',#21960,#17682,#17683);
#15016=AXIS2_PLACEMENT_3D('',#21961,#17684,#17685);
#15017=AXIS2_PLACEMENT_3D('',#21962,#17686,#17687);
#15018=AXIS2_PLACEMENT_3D('',#21963,#17688,#17689);
#15019=AXIS2_PLACEMENT_3D('',#21964,#17690,#17691);
#15020=AXIS2_PLACEMENT_3D('',#21965,#17692,#17693);
#15021=AXIS2_PLACEMENT_3D('',#21967,#17694,#17695);
#15022=AXIS2_PLACEMENT_3D('',#21969,#17696,#17697);
#15023=AXIS2_PLACEMENT_3D('',#21970,#17698,#17699);
#15024=AXIS2_PLACEMENT_3D('',#21972,#17700,#17701);
#15025=AXIS2_PLACEMENT_3D('',#21974,#17703,#17704);
#15026=AXIS2_PLACEMENT_3D('',#21976,#17705,#17706);
#15027=AXIS2_PLACEMENT_3D('',#21977,#17707,#17708);
#15028=AXIS2_PLACEMENT_3D('',#21979,#17710,#17711);
#15029=AXIS2_PLACEMENT_3D('',#21981,#17712,#17713);
#15030=AXIS2_PLACEMENT_3D('',#21983,#17714,#17715);
#15031=AXIS2_PLACEMENT_3D('',#21984,#17716,#17717);
#15032=AXIS2_PLACEMENT_3D('',#21986,#17718,#17719);
#15033=AXIS2_PLACEMENT_3D('',#21988,#17721,#17722);
#15034=AXIS2_PLACEMENT_3D('',#21990,#17723,#17724);
#15035=AXIS2_PLACEMENT_3D('',#21991,#17725,#17726);
#15036=AXIS2_PLACEMENT_3D('',#21993,#17728,#17729);
#15037=AXIS2_PLACEMENT_3D('',#21994,#17730,#17731);
#15038=AXIS2_PLACEMENT_3D('',#21995,#17732,#17733);
#15039=AXIS2_PLACEMENT_3D('',#21996,#17734,#17735);
#15040=AXIS2_PLACEMENT_3D('',#21997,#17736,#17737);
#15041=AXIS2_PLACEMENT_3D('',#21998,#17738,#17739);
#15042=AXIS2_PLACEMENT_3D('',#21999,#17740,#17741);
#15043=AXIS2_PLACEMENT_3D('',#22000,#17742,#17743);
#15044=AXIS2_PLACEMENT_3D('',#22002,#17744,#17745);
#15045=AXIS2_PLACEMENT_3D('',#22005,#17747,#17748);
#15046=AXIS2_PLACEMENT_3D('',#22006,#17749,#17750);
#15047=AXIS2_PLACEMENT_3D('',#22007,#17751,#17752);
#15048=AXIS2_PLACEMENT_3D('',#22016,#17757,#17758);
#15049=AXIS2_PLACEMENT_3D('',#22018,#17759,#17760);
#15050=AXIS2_PLACEMENT_3D('',#22022,#17763,#17764);
#15051=AXIS2_PLACEMENT_3D('',#22026,#17767,#17768);
#15052=AXIS2_PLACEMENT_3D('',#22030,#17771,#17772);
#15053=AXIS2_PLACEMENT_3D('',#22031,#17773,#17774);
#15054=AXIS2_PLACEMENT_3D('',#22032,#17775,#17776);
#15055=AXIS2_PLACEMENT_3D('',#22034,#17777,#17778);
#15056=AXIS2_PLACEMENT_3D('',#22036,#17779,#17780);
#15057=AXIS2_PLACEMENT_3D('',#22037,#17781,#17782);
#15058=AXIS2_PLACEMENT_3D('',#22039,#17783,#17784);
#15059=AXIS2_PLACEMENT_3D('',#22041,#17785,#17786);
#15060=AXIS2_PLACEMENT_3D('',#22042,#17787,#17788);
#15061=AXIS2_PLACEMENT_3D('',#22044,#17790,#17791);
#15062=AXIS2_PLACEMENT_3D('',#22047,#17793,#17794);
#15063=AXIS2_PLACEMENT_3D('',#22048,#17795,#17796);
#15064=AXIS2_PLACEMENT_3D('',#22050,#17797,#17798);
#15065=AXIS2_PLACEMENT_3D('',#22052,#17800,#17801);
#15066=AXIS2_PLACEMENT_3D('',#22053,#17802,#17803);
#15067=AXIS2_PLACEMENT_3D('',#22054,#17804,#17805);
#15068=AXIS2_PLACEMENT_3D('',#22055,#17806,#17807);
#15069=AXIS2_PLACEMENT_3D('',#22057,#17808,#17809);
#15070=AXIS2_PLACEMENT_3D('',#22060,#17811,#17812);
#15071=AXIS2_PLACEMENT_3D('',#22061,#17813,#17814);
#15072=AXIS2_PLACEMENT_3D('',#22063,#17815,#17816);
#15073=AXIS2_PLACEMENT_3D('',#22066,#17818,#17819);
#15074=AXIS2_PLACEMENT_3D('',#22067,#17820,#17821);
#15075=AXIS2_PLACEMENT_3D('',#22068,#17822,#17823);
#15076=AXIS2_PLACEMENT_3D('',#22069,#17824,#17825);
#15077=AXIS2_PLACEMENT_3D('',#22070,#17826,#17827);
#15078=AXIS2_PLACEMENT_3D('',#22072,#17828,#17829);
#15079=AXIS2_PLACEMENT_3D('',#22075,#17831,#17832);
#15080=AXIS2_PLACEMENT_3D('',#22076,#17833,#17834);
#15081=AXIS2_PLACEMENT_3D('',#22078,#17835,#17836);
#15082=AXIS2_PLACEMENT_3D('',#22081,#17838,#17839);
#15083=AXIS2_PLACEMENT_3D('',#22082,#17840,#17841);
#15084=AXIS2_PLACEMENT_3D('',#22083,#17842,#17843);
#15085=AXIS2_PLACEMENT_3D('',#22084,#17844,#17845);
#15086=AXIS2_PLACEMENT_3D('',#22085,#17846,#17847);
#15087=AXIS2_PLACEMENT_3D('',#22087,#17848,#17849);
#15088=AXIS2_PLACEMENT_3D('',#22090,#17851,#17852);
#15089=AXIS2_PLACEMENT_3D('',#22091,#17853,#17854);
#15090=AXIS2_PLACEMENT_3D('',#22093,#17855,#17856);
#15091=AXIS2_PLACEMENT_3D('',#22096,#17858,#17859);
#15092=AXIS2_PLACEMENT_3D('',#22097,#17860,#17861);
#15093=AXIS2_PLACEMENT_3D('',#22098,#17862,#17863);
#15094=AXIS2_PLACEMENT_3D('',#22099,#17864,#17865);
#15095=AXIS2_PLACEMENT_3D('',#22100,#17866,#17867);
#15096=AXIS2_PLACEMENT_3D('',#22104,#17869,#17870);
#15097=AXIS2_PLACEMENT_3D('',#22105,#17871,#17872);
#15098=AXIS2_PLACEMENT_3D('',#22110,#17874,#17875);
#15099=AXIS2_PLACEMENT_3D('',#22112,#17876,#17877);
#15100=AXIS2_PLACEMENT_3D('',#22115,#17879,#17880);
#15101=AXIS2_PLACEMENT_3D('',#22116,#17881,#17882);
#15102=AXIS2_PLACEMENT_3D('',#22133,#17883,#17884);
#15103=AXIS2_PLACEMENT_3D('',#22165,#17886,#17887);
#15104=AXIS2_PLACEMENT_3D('',#22167,#17889,#17890);
#15105=AXIS2_PLACEMENT_3D('',#22169,#17891,#17892);
#15106=AXIS2_PLACEMENT_3D('',#22172,#17894,#17895);
#15107=AXIS2_PLACEMENT_3D('',#22173,#17896,#17897);
#15108=AXIS2_PLACEMENT_3D('',#22175,#17898,#17899);
#15109=AXIS2_PLACEMENT_3D('',#22178,#17901,#17902);
#15110=AXIS2_PLACEMENT_3D('',#22179,#17903,#17904);
#15111=AXIS2_PLACEMENT_3D('',#22180,#17905,#17906);
#15112=AXIS2_PLACEMENT_3D('',#22181,#17907,#17908);
#15113=AXIS2_PLACEMENT_3D('',#22182,#17909,#17910);
#15114=AXIS2_PLACEMENT_3D('',#22191,#17915,#17916);
#15115=AXIS2_PLACEMENT_3D('',#22197,#17920,#17921);
#15116=AXIS2_PLACEMENT_3D('',#22203,#17925,#17926);
#15117=AXIS2_PLACEMENT_3D('',#22206,#17929,#17930);
#15118=AXIS2_PLACEMENT_3D('',#22207,#17931,#17932);
#15119=AXIS2_PLACEMENT_3D('',#22208,#17933,#17934);
#15120=AXIS2_PLACEMENT_3D('',#22209,#17935,#17936);
#15121=AXIS2_PLACEMENT_3D('',#22211,#17937,#17938);
#15122=AXIS2_PLACEMENT_3D('',#22214,#17940,#17941);
#15123=AXIS2_PLACEMENT_3D('',#22215,#17942,#17943);
#15124=AXIS2_PLACEMENT_3D('',#22217,#17944,#17945);
#15125=AXIS2_PLACEMENT_3D('',#22220,#17947,#17948);
#15126=AXIS2_PLACEMENT_3D('',#22221,#17949,#17950);
#15127=AXIS2_PLACEMENT_3D('',#22222,#17951,#17952);
#15128=AXIS2_PLACEMENT_3D('',#22223,#17953,#17954);
#15129=AXIS2_PLACEMENT_3D('',#22224,#17955,#17956);
#15130=AXIS2_PLACEMENT_3D('',#22233,#17961,#17962);
#15131=AXIS2_PLACEMENT_3D('',#22239,#17966,#17967);
#15132=AXIS2_PLACEMENT_3D('',#22245,#17971,#17972);
#15133=AXIS2_PLACEMENT_3D('',#22248,#17973,#17974);
#15134=AXIS2_PLACEMENT_3D('',#22394,#17976,#17977);
#15135=AXIS2_PLACEMENT_3D('',#22540,#17979,#17980);
#15136=AXIS2_PLACEMENT_3D('',#22686,#17982,#17983);
#15137=AXIS2_PLACEMENT_3D('',#22832,#17985,#17986);
#15138=AXIS2_PLACEMENT_3D('',#22978,#17988,#17989);
#15139=AXIS2_PLACEMENT_3D('',#23124,#17991,#17992);
#15140=AXIS2_PLACEMENT_3D('',#23270,#17994,#17995);
#15141=AXIS2_PLACEMENT_3D('',#23416,#17997,#17998);
#15142=AXIS2_PLACEMENT_3D('',#23562,#18000,#18001);
#15143=AXIS2_PLACEMENT_3D('',#23708,#18003,#18004);
#15144=AXIS2_PLACEMENT_3D('',#23854,#18006,#18007);
#15145=AXIS2_PLACEMENT_3D('',#24000,#18009,#18010);
#15146=AXIS2_PLACEMENT_3D('',#24146,#18012,#18013);
#15147=AXIS2_PLACEMENT_3D('',#24292,#18015,#18016);
#15148=AXIS2_PLACEMENT_3D('',#24438,#18018,#18019);
#15149=AXIS2_PLACEMENT_3D('',#24584,#18021,#18022);
#15150=AXIS2_PLACEMENT_3D('',#24730,#18024,#18025);
#15151=AXIS2_PLACEMENT_3D('',#24876,#18027,#18028);
#15152=AXIS2_PLACEMENT_3D('',#25022,#18030,#18031);
#15153=AXIS2_PLACEMENT_3D('',#25166,#18033,#18034);
#15154=AXIS2_PLACEMENT_3D('',#25167,#18035,#18036);
#15155=AXIS2_PLACEMENT_3D('',#25168,#18037,#18038);
#15156=AXIS2_PLACEMENT_3D('',#25169,#18039,#18040);
#15157=AXIS2_PLACEMENT_3D('',#25171,#18041,#18042);
#15158=AXIS2_PLACEMENT_3D('',#25174,#18044,#18045);
#15159=AXIS2_PLACEMENT_3D('',#25175,#18046,#18047);
#15160=AXIS2_PLACEMENT_3D('',#25390,#18050,#18051);
#15161=AXIS2_PLACEMENT_3D('',#25606,#18055,#18056);
#15162=AXIS2_PLACEMENT_3D('',#25608,#18057,#18058);
#15163=AXIS2_PLACEMENT_3D('',#25822,#18061,#18062);
#15164=AXIS2_PLACEMENT_3D('',#26038,#18066,#18067);
#15165=AXIS2_PLACEMENT_3D('',#26040,#18068,#18069);
#15166=AXIS2_PLACEMENT_3D('',#26254,#18072,#18073);
#15167=AXIS2_PLACEMENT_3D('',#26470,#18077,#18078);
#15168=AXIS2_PLACEMENT_3D('',#26472,#18079,#18080);
#15169=AXIS2_PLACEMENT_3D('',#26686,#18083,#18084);
#15170=AXIS2_PLACEMENT_3D('',#26902,#18088,#18089);
#15171=AXIS2_PLACEMENT_3D('',#26904,#18090,#18091);
#15172=AXIS2_PLACEMENT_3D('',#27118,#18094,#18095);
#15173=AXIS2_PLACEMENT_3D('',#27334,#18099,#18100);
#15174=AXIS2_PLACEMENT_3D('',#27336,#18101,#18102);
#15175=AXIS2_PLACEMENT_3D('',#27550,#18105,#18106);
#15176=AXIS2_PLACEMENT_3D('',#27766,#18110,#18111);
#15177=AXIS2_PLACEMENT_3D('',#27768,#18112,#18113);
#15178=AXIS2_PLACEMENT_3D('',#27982,#18116,#18117);
#15179=AXIS2_PLACEMENT_3D('',#28198,#18121,#18122);
#15180=AXIS2_PLACEMENT_3D('',#28200,#18123,#18124);
#15181=AXIS2_PLACEMENT_3D('',#28414,#18127,#18128);
#15182=AXIS2_PLACEMENT_3D('',#28630,#18132,#18133);
#15183=AXIS2_PLACEMENT_3D('',#28632,#18134,#18135);
#15184=AXIS2_PLACEMENT_3D('',#28846,#18138,#18139);
#15185=AXIS2_PLACEMENT_3D('',#29062,#18143,#18144);
#15186=AXIS2_PLACEMENT_3D('',#29064,#18145,#18146);
#15187=AXIS2_PLACEMENT_3D('',#29278,#18149,#18150);
#15188=AXIS2_PLACEMENT_3D('',#29494,#18154,#18155);
#15189=AXIS2_PLACEMENT_3D('',#29496,#18156,#18157);
#15190=AXIS2_PLACEMENT_3D('',#29710,#18160,#18161);
#15191=AXIS2_PLACEMENT_3D('',#29926,#18165,#18166);
#15192=AXIS2_PLACEMENT_3D('',#29928,#18167,#18168);
#15193=AXIS2_PLACEMENT_3D('',#30142,#18171,#18172);
#15194=AXIS2_PLACEMENT_3D('',#30358,#18176,#18177);
#15195=AXIS2_PLACEMENT_3D('',#30360,#18178,#18179);
#15196=AXIS2_PLACEMENT_3D('',#30574,#18182,#18183);
#15197=AXIS2_PLACEMENT_3D('',#30790,#18187,#18188);
#15198=AXIS2_PLACEMENT_3D('',#30792,#18189,#18190);
#15199=AXIS2_PLACEMENT_3D('',#31006,#18193,#18194);
#15200=AXIS2_PLACEMENT_3D('',#31222,#18198,#18199);
#15201=AXIS2_PLACEMENT_3D('',#31224,#18200,#18201);
#15202=AXIS2_PLACEMENT_3D('',#31438,#18204,#18205);
#15203=AXIS2_PLACEMENT_3D('',#31654,#18209,#18210);
#15204=AXIS2_PLACEMENT_3D('',#31656,#18211,#18212);
#15205=AXIS2_PLACEMENT_3D('',#31870,#18215,#18216);
#15206=AXIS2_PLACEMENT_3D('',#32086,#18220,#18221);
#15207=AXIS2_PLACEMENT_3D('',#32088,#18222,#18223);
#15208=AXIS2_PLACEMENT_3D('',#32302,#18226,#18227);
#15209=AXIS2_PLACEMENT_3D('',#32518,#18231,#18232);
#15210=AXIS2_PLACEMENT_3D('',#32520,#18233,#18234);
#15211=AXIS2_PLACEMENT_3D('',#32734,#18237,#18238);
#15212=AXIS2_PLACEMENT_3D('',#32950,#18242,#18243);
#15213=AXIS2_PLACEMENT_3D('',#32952,#18244,#18245);
#15214=AXIS2_PLACEMENT_3D('',#33166,#18248,#18249);
#15215=AXIS2_PLACEMENT_3D('',#33382,#18253,#18254);
#15216=AXIS2_PLACEMENT_3D('',#33384,#18255,#18256);
#15217=AXIS2_PLACEMENT_3D('',#33598,#18259,#18260);
#15218=AXIS2_PLACEMENT_3D('',#33814,#18264,#18265);
#15219=AXIS2_PLACEMENT_3D('',#33815,#18266,#18267);
#15220=AXIS2_PLACEMENT_3D('',#33816,#18268,#18269);
#15221=AXIS2_PLACEMENT_3D('',#33817,#18270,#18271);
#15222=AXIS2_PLACEMENT_3D('',#33818,#18272,#18273);
#15223=AXIS2_PLACEMENT_3D('',#33819,#18274,#18275);
#15224=AXIS2_PLACEMENT_3D('',#33821,#18276,#18277);
#15225=AXIS2_PLACEMENT_3D('',#33824,#18279,#18280);
#15226=AXIS2_PLACEMENT_3D('',#33825,#18281,#18282);
#15227=AXIS2_PLACEMENT_3D('',#33826,#18283,#18284);
#15228=AXIS2_PLACEMENT_3D('',#33835,#18289,#18290);
#15229=AXIS2_PLACEMENT_3D('',#33837,#18291,#18292);
#15230=AXIS2_PLACEMENT_3D('',#33841,#18295,#18296);
#15231=AXIS2_PLACEMENT_3D('',#33845,#18299,#18300);
#15232=AXIS2_PLACEMENT_3D('',#33849,#18303,#18304);
#15233=AXIS2_PLACEMENT_3D('',#33850,#18305,#18306);
#15234=AXIS2_PLACEMENT_3D('',#33851,#18307,#18308);
#15235=AXIS2_PLACEMENT_3D('',#33853,#18309,#18310);
#15236=AXIS2_PLACEMENT_3D('',#33855,#18311,#18312);
#15237=AXIS2_PLACEMENT_3D('',#33856,#18313,#18314);
#15238=AXIS2_PLACEMENT_3D('',#33858,#18315,#18316);
#15239=AXIS2_PLACEMENT_3D('',#33860,#18317,#18318);
#15240=AXIS2_PLACEMENT_3D('',#33861,#18319,#18320);
#15241=AXIS2_PLACEMENT_3D('',#33863,#18322,#18323);
#15242=AXIS2_PLACEMENT_3D('',#33866,#18325,#18326);
#15243=AXIS2_PLACEMENT_3D('',#33867,#18327,#18328);
#15244=AXIS2_PLACEMENT_3D('',#33869,#18329,#18330);
#15245=AXIS2_PLACEMENT_3D('',#33871,#18332,#18333);
#15246=AXIS2_PLACEMENT_3D('',#33872,#18334,#18335);
#15247=AXIS2_PLACEMENT_3D('',#33873,#18336,#18337);
#15248=AXIS2_PLACEMENT_3D('',#33874,#18338,#18339);
#15249=AXIS2_PLACEMENT_3D('',#33876,#18340,#18341);
#15250=AXIS2_PLACEMENT_3D('',#33879,#18343,#18344);
#15251=AXIS2_PLACEMENT_3D('',#33880,#18345,#18346);
#15252=AXIS2_PLACEMENT_3D('',#33882,#18347,#18348);
#15253=AXIS2_PLACEMENT_3D('',#33885,#18350,#18351);
#15254=AXIS2_PLACEMENT_3D('',#33886,#18352,#18353);
#15255=AXIS2_PLACEMENT_3D('',#33887,#18354,#18355);
#15256=AXIS2_PLACEMENT_3D('',#33888,#18356,#18357);
#15257=AXIS2_PLACEMENT_3D('',#33889,#18358,#18359);
#15258=AXIS2_PLACEMENT_3D('',#33891,#18360,#18361);
#15259=AXIS2_PLACEMENT_3D('',#33894,#18363,#18364);
#15260=AXIS2_PLACEMENT_3D('',#33895,#18365,#18366);
#15261=AXIS2_PLACEMENT_3D('',#33897,#18367,#18368);
#15262=AXIS2_PLACEMENT_3D('',#33900,#18370,#18371);
#15263=AXIS2_PLACEMENT_3D('',#33901,#18372,#18373);
#15264=AXIS2_PLACEMENT_3D('',#33902,#18374,#18375);
#15265=AXIS2_PLACEMENT_3D('',#33903,#18376,#18377);
#15266=AXIS2_PLACEMENT_3D('',#33904,#18378,#18379);
#15267=AXIS2_PLACEMENT_3D('',#33982,#18381,#18382);
#15268=AXIS2_PLACEMENT_3D('',#33984,#18383,#18384);
#15269=AXIS2_PLACEMENT_3D('',#33987,#18386,#18387);
#15270=AXIS2_PLACEMENT_3D('',#33988,#18388,#18389);
#15271=AXIS2_PLACEMENT_3D('',#33990,#18390,#18391);
#15272=AXIS2_PLACEMENT_3D('',#33993,#18393,#18394);
#15273=AXIS2_PLACEMENT_3D('',#33994,#18395,#18396);
#15274=AXIS2_PLACEMENT_3D('',#33995,#18397,#18398);
#15275=AXIS2_PLACEMENT_3D('',#33996,#18399,#18400);
#15276=AXIS2_PLACEMENT_3D('',#33997,#18401,#18402);
#15277=AXIS2_PLACEMENT_3D('',#34006,#18407,#18408);
#15278=AXIS2_PLACEMENT_3D('',#34012,#18412,#18413);
#15279=AXIS2_PLACEMENT_3D('',#34018,#18417,#18418);
#15280=AXIS2_PLACEMENT_3D('',#34021,#18421,#18422);
#15281=AXIS2_PLACEMENT_3D('',#34022,#18423,#18424);
#15282=AXIS2_PLACEMENT_3D('',#34023,#18425,#18426);
#15283=AXIS2_PLACEMENT_3D('',#34024,#18427,#18428);
#15284=AXIS2_PLACEMENT_3D('',#34026,#18429,#18430);
#15285=AXIS2_PLACEMENT_3D('',#34029,#18432,#18433);
#15286=AXIS2_PLACEMENT_3D('',#34030,#18434,#18435);
#15287=AXIS2_PLACEMENT_3D('',#34032,#18436,#18437);
#15288=AXIS2_PLACEMENT_3D('',#34035,#18439,#18440);
#15289=AXIS2_PLACEMENT_3D('',#34036,#18441,#18442);
#15290=AXIS2_PLACEMENT_3D('',#34037,#18443,#18444);
#15291=AXIS2_PLACEMENT_3D('',#34038,#18445,#18446);
#15292=AXIS2_PLACEMENT_3D('',#34039,#18447,#18448);
#15293=AXIS2_PLACEMENT_3D('',#34041,#18449,#18450);
#15294=AXIS2_PLACEMENT_3D('',#34042,#18451,#18452);
#15295=AXIS2_PLACEMENT_3D('',#34051,#18457,#18458);
#15296=AXIS2_PLACEMENT_3D('',#34057,#18462,#18463);
#15297=AXIS2_PLACEMENT_3D('',#34063,#18467,#18468);
#15298=AXIS2_PLACEMENT_3D('',#34069,#18472,#18473);
#15299=AXIS2_PLACEMENT_3D('',#34075,#18477,#18478);
#15300=AXIS2_PLACEMENT_3D('',#34078,#18481,#18482);
#15301=AXIS2_PLACEMENT_3D('',#34079,#18483,#18484);
#15302=AXIS2_PLACEMENT_3D('',#34081,#18485,#18486);
#15303=AXIS2_PLACEMENT_3D('',#34082,#18487,#18488);
#15304=AXIS2_PLACEMENT_3D('',#34084,#18489,#18490);
#15305=AXIS2_PLACEMENT_3D('',#34086,#18492,#18493);
#15306=AXIS2_PLACEMENT_3D('',#34088,#18495,#18496);
#15307=AXIS2_PLACEMENT_3D('',#34089,#18497,#18498);
#15308=AXIS2_PLACEMENT_3D('',#34098,#18503,#18504);
#15309=AXIS2_PLACEMENT_3D('',#34104,#18508,#18509);
#15310=AXIS2_PLACEMENT_3D('',#34110,#18513,#18514);
#15311=AXIS2_PLACEMENT_3D('',#34113,#18515,#18516);
#15312=AXIS2_PLACEMENT_3D('',#34259,#18518,#18519);
#15313=AXIS2_PLACEMENT_3D('',#34405,#18521,#18522);
#15314=AXIS2_PLACEMENT_3D('',#34551,#18524,#18525);
#15315=AXIS2_PLACEMENT_3D('',#34697,#18527,#18528);
#15316=AXIS2_PLACEMENT_3D('',#34843,#18530,#18531);
#15317=AXIS2_PLACEMENT_3D('',#34989,#18533,#18534);
#15318=AXIS2_PLACEMENT_3D('',#35135,#18536,#18537);
#15319=AXIS2_PLACEMENT_3D('',#35281,#18539,#18540);
#15320=AXIS2_PLACEMENT_3D('',#35427,#18542,#18543);
#15321=AXIS2_PLACEMENT_3D('',#35573,#18545,#18546);
#15322=AXIS2_PLACEMENT_3D('',#35719,#18548,#18549);
#15323=AXIS2_PLACEMENT_3D('',#35865,#18551,#18552);
#15324=AXIS2_PLACEMENT_3D('',#36011,#18554,#18555);
#15325=AXIS2_PLACEMENT_3D('',#36157,#18557,#18558);
#15326=AXIS2_PLACEMENT_3D('',#36303,#18560,#18561);
#15327=AXIS2_PLACEMENT_3D('',#36449,#18563,#18564);
#15328=AXIS2_PLACEMENT_3D('',#36595,#18566,#18567);
#15329=AXIS2_PLACEMENT_3D('',#36741,#18569,#18570);
#15330=AXIS2_PLACEMENT_3D('',#36887,#18572,#18573);
#15331=AXIS2_PLACEMENT_3D('',#37033,#18575,#18576);
#15332=AXIS2_PLACEMENT_3D('',#37179,#18578,#18579);
#15333=AXIS2_PLACEMENT_3D('',#37325,#18581,#18582);
#15334=AXIS2_PLACEMENT_3D('',#37471,#18584,#18585);
#15335=AXIS2_PLACEMENT_3D('',#37617,#18587,#18588);
#15336=AXIS2_PLACEMENT_3D('',#37763,#18590,#18591);
#15337=AXIS2_PLACEMENT_3D('',#37909,#18593,#18594);
#15338=AXIS2_PLACEMENT_3D('',#38055,#18596,#18597);
#15339=AXIS2_PLACEMENT_3D('',#38201,#18599,#18600);
#15340=AXIS2_PLACEMENT_3D('',#38347,#18602,#18603);
#15341=AXIS2_PLACEMENT_3D('',#38493,#18605,#18606);
#15342=AXIS2_PLACEMENT_3D('',#38639,#18608,#18609);
#15343=AXIS2_PLACEMENT_3D('',#38785,#18611,#18612);
#15344=AXIS2_PLACEMENT_3D('',#38931,#18614,#18615);
#15345=AXIS2_PLACEMENT_3D('',#39077,#18617,#18618);
#15346=AXIS2_PLACEMENT_3D('',#39223,#18620,#18621);
#15347=AXIS2_PLACEMENT_3D('',#39369,#18623,#18624);
#15348=AXIS2_PLACEMENT_3D('',#39515,#18626,#18627);
#15349=AXIS2_PLACEMENT_3D('',#39661,#18629,#18630);
#15350=AXIS2_PLACEMENT_3D('',#39807,#18632,#18633);
#15351=AXIS2_PLACEMENT_3D('',#39951,#18635,#18636);
#15352=AXIS2_PLACEMENT_3D('',#39952,#18637,#18638);
#15353=AXIS2_PLACEMENT_3D('',#39953,#18639,#18640);
#15354=AXIS2_PLACEMENT_3D('',#39954,#18641,#18642);
#15355=AXIS2_PLACEMENT_3D('',#39956,#18643,#18644);
#15356=AXIS2_PLACEMENT_3D('',#39959,#18646,#18647);
#15357=AXIS2_PLACEMENT_3D('',#39960,#18648,#18649);
#15358=AXIS2_PLACEMENT_3D('',#40399,#18652,#18653);
#15359=AXIS2_PLACEMENT_3D('',#40401,#18655,#18656);
#15360=AXIS2_PLACEMENT_3D('',#40403,#18657,#18658);
#15361=AXIS2_PLACEMENT_3D('',#40841,#18661,#18662);
#15362=AXIS2_PLACEMENT_3D('',#40843,#18664,#18665);
#15363=AXIS2_PLACEMENT_3D('',#40845,#18666,#18667);
#15364=AXIS2_PLACEMENT_3D('',#41283,#18670,#18671);
#15365=AXIS2_PLACEMENT_3D('',#41285,#18673,#18674);
#15366=AXIS2_PLACEMENT_3D('',#41287,#18675,#18676);
#15367=AXIS2_PLACEMENT_3D('',#41725,#18679,#18680);
#15368=AXIS2_PLACEMENT_3D('',#41727,#18682,#18683);
#15369=AXIS2_PLACEMENT_3D('',#41729,#18684,#18685);
#15370=AXIS2_PLACEMENT_3D('',#42167,#18688,#18689);
#15371=AXIS2_PLACEMENT_3D('',#42169,#18691,#18692);
#15372=AXIS2_PLACEMENT_3D('',#42171,#18693,#18694);
#15373=AXIS2_PLACEMENT_3D('',#42609,#18697,#18698);
#15374=AXIS2_PLACEMENT_3D('',#42611,#18700,#18701);
#15375=AXIS2_PLACEMENT_3D('',#42613,#18702,#18703);
#15376=AXIS2_PLACEMENT_3D('',#43051,#18706,#18707);
#15377=AXIS2_PLACEMENT_3D('',#43053,#18709,#18710);
#15378=AXIS2_PLACEMENT_3D('',#43055,#18711,#18712);
#15379=AXIS2_PLACEMENT_3D('',#43493,#18715,#18716);
#15380=AXIS2_PLACEMENT_3D('',#43495,#18718,#18719);
#15381=AXIS2_PLACEMENT_3D('',#43497,#18720,#18721);
#15382=AXIS2_PLACEMENT_3D('',#43935,#18724,#18725);
#15383=AXIS2_PLACEMENT_3D('',#43937,#18727,#18728);
#15384=AXIS2_PLACEMENT_3D('',#43939,#18729,#18730);
#15385=AXIS2_PLACEMENT_3D('',#44377,#18733,#18734);
#15386=AXIS2_PLACEMENT_3D('',#44379,#18736,#18737);
#15387=AXIS2_PLACEMENT_3D('',#44381,#18738,#18739);
#15388=AXIS2_PLACEMENT_3D('',#44819,#18742,#18743);
#15389=AXIS2_PLACEMENT_3D('',#44821,#18745,#18746);
#15390=AXIS2_PLACEMENT_3D('',#44823,#18747,#18748);
#15391=AXIS2_PLACEMENT_3D('',#45261,#18751,#18752);
#15392=AXIS2_PLACEMENT_3D('',#45263,#18754,#18755);
#15393=AXIS2_PLACEMENT_3D('',#45265,#18756,#18757);
#15394=AXIS2_PLACEMENT_3D('',#45703,#18760,#18761);
#15395=AXIS2_PLACEMENT_3D('',#45705,#18763,#18764);
#15396=AXIS2_PLACEMENT_3D('',#45707,#18765,#18766);
#15397=AXIS2_PLACEMENT_3D('',#46145,#18769,#18770);
#15398=AXIS2_PLACEMENT_3D('',#46147,#18772,#18773);
#15399=AXIS2_PLACEMENT_3D('',#46149,#18774,#18775);
#15400=AXIS2_PLACEMENT_3D('',#46587,#18778,#18779);
#15401=AXIS2_PLACEMENT_3D('',#46589,#18781,#18782);
#15402=AXIS2_PLACEMENT_3D('',#46591,#18783,#18784);
#15403=AXIS2_PLACEMENT_3D('',#47029,#18787,#18788);
#15404=AXIS2_PLACEMENT_3D('',#47031,#18790,#18791);
#15405=AXIS2_PLACEMENT_3D('',#47033,#18792,#18793);
#15406=AXIS2_PLACEMENT_3D('',#47471,#18796,#18797);
#15407=AXIS2_PLACEMENT_3D('',#47473,#18799,#18800);
#15408=AXIS2_PLACEMENT_3D('',#47475,#18801,#18802);
#15409=AXIS2_PLACEMENT_3D('',#47913,#18805,#18806);
#15410=AXIS2_PLACEMENT_3D('',#47915,#18808,#18809);
#15411=AXIS2_PLACEMENT_3D('',#47917,#18810,#18811);
#15412=AXIS2_PLACEMENT_3D('',#48355,#18814,#18815);
#15413=AXIS2_PLACEMENT_3D('',#48357,#18817,#18818);
#15414=AXIS2_PLACEMENT_3D('',#48359,#18819,#18820);
#15415=AXIS2_PLACEMENT_3D('',#48797,#18823,#18824);
#15416=AXIS2_PLACEMENT_3D('',#48799,#18826,#18827);
#15417=AXIS2_PLACEMENT_3D('',#48801,#18828,#18829);
#15418=AXIS2_PLACEMENT_3D('',#49239,#18832,#18833);
#15419=AXIS2_PLACEMENT_3D('',#49241,#18835,#18836);
#15420=AXIS2_PLACEMENT_3D('',#49243,#18837,#18838);
#15421=AXIS2_PLACEMENT_3D('',#49681,#18841,#18842);
#15422=AXIS2_PLACEMENT_3D('',#49683,#18844,#18845);
#15423=AXIS2_PLACEMENT_3D('',#49685,#18846,#18847);
#15424=AXIS2_PLACEMENT_3D('',#50123,#18850,#18851);
#15425=AXIS2_PLACEMENT_3D('',#50125,#18853,#18854);
#15426=AXIS2_PLACEMENT_3D('',#50127,#18855,#18856);
#15427=AXIS2_PLACEMENT_3D('',#50565,#18859,#18860);
#15428=AXIS2_PLACEMENT_3D('',#50567,#18862,#18863);
#15429=AXIS2_PLACEMENT_3D('',#50569,#18864,#18865);
#15430=AXIS2_PLACEMENT_3D('',#51007,#18868,#18869);
#15431=AXIS2_PLACEMENT_3D('',#51009,#18871,#18872);
#15432=AXIS2_PLACEMENT_3D('',#51011,#18873,#18874);
#15433=AXIS2_PLACEMENT_3D('',#51449,#18877,#18878);
#15434=AXIS2_PLACEMENT_3D('',#51451,#18880,#18881);
#15435=AXIS2_PLACEMENT_3D('',#51453,#18882,#18883);
#15436=AXIS2_PLACEMENT_3D('',#51891,#18886,#18887);
#15437=AXIS2_PLACEMENT_3D('',#51893,#18889,#18890);
#15438=AXIS2_PLACEMENT_3D('',#51895,#18891,#18892);
#15439=AXIS2_PLACEMENT_3D('',#52333,#18895,#18896);
#15440=AXIS2_PLACEMENT_3D('',#52335,#18898,#18899);
#15441=AXIS2_PLACEMENT_3D('',#52337,#18900,#18901);
#15442=AXIS2_PLACEMENT_3D('',#52775,#18904,#18905);
#15443=AXIS2_PLACEMENT_3D('',#52777,#18907,#18908);
#15444=AXIS2_PLACEMENT_3D('',#52779,#18909,#18910);
#15445=AXIS2_PLACEMENT_3D('',#53217,#18913,#18914);
#15446=AXIS2_PLACEMENT_3D('',#53219,#18916,#18917);
#15447=AXIS2_PLACEMENT_3D('',#53221,#18918,#18919);
#15448=AXIS2_PLACEMENT_3D('',#53659,#18922,#18923);
#15449=AXIS2_PLACEMENT_3D('',#53661,#18925,#18926);
#15450=AXIS2_PLACEMENT_3D('',#53663,#18927,#18928);
#15451=AXIS2_PLACEMENT_3D('',#54101,#18931,#18932);
#15452=AXIS2_PLACEMENT_3D('',#54103,#18934,#18935);
#15453=AXIS2_PLACEMENT_3D('',#54105,#18936,#18937);
#15454=AXIS2_PLACEMENT_3D('',#54543,#18940,#18941);
#15455=AXIS2_PLACEMENT_3D('',#54545,#18943,#18944);
#15456=AXIS2_PLACEMENT_3D('',#54547,#18945,#18946);
#15457=AXIS2_PLACEMENT_3D('',#54985,#18949,#18950);
#15458=AXIS2_PLACEMENT_3D('',#54987,#18952,#18953);
#15459=AXIS2_PLACEMENT_3D('',#54989,#18954,#18955);
#15460=AXIS2_PLACEMENT_3D('',#55427,#18958,#18959);
#15461=AXIS2_PLACEMENT_3D('',#55429,#18961,#18962);
#15462=AXIS2_PLACEMENT_3D('',#55431,#18963,#18964);
#15463=AXIS2_PLACEMENT_3D('',#55869,#18967,#18968);
#15464=AXIS2_PLACEMENT_3D('',#55871,#18970,#18971);
#15465=AXIS2_PLACEMENT_3D('',#55873,#18972,#18973);
#15466=AXIS2_PLACEMENT_3D('',#56311,#18976,#18977);
#15467=AXIS2_PLACEMENT_3D('',#56313,#18979,#18980);
#15468=AXIS2_PLACEMENT_3D('',#56315,#18981,#18982);
#15469=AXIS2_PLACEMENT_3D('',#56753,#18985,#18986);
#15470=AXIS2_PLACEMENT_3D('',#56755,#18988,#18989);
#15471=AXIS2_PLACEMENT_3D('',#56757,#18990,#18991);
#15472=AXIS2_PLACEMENT_3D('',#56976,#18993,#18994);
#15473=AXIS2_PLACEMENT_3D('',#57197,#18997,#18998);
#15474=AXIS2_PLACEMENT_3D('',#57199,#18999,#19000);
#15475=AXIS2_PLACEMENT_3D('',#57637,#19003,#19004);
#15476=AXIS2_PLACEMENT_3D('',#57639,#19006,#19007);
#15477=AXIS2_PLACEMENT_3D('',#57640,#19008,#19009);
#15478=AXIS2_PLACEMENT_3D('',#57641,#19010,#19011);
#15479=AXIS2_PLACEMENT_3D('',#57642,#19012,#19013);
#15480=AXIS2_PLACEMENT_3D('',#57643,#19014,#19015);
#15481=AXIS2_PLACEMENT_3D('',#57652,#19020,#19021);
#15482=AXIS2_PLACEMENT_3D('',#57658,#19025,#19026);
#15483=AXIS2_PLACEMENT_3D('',#57664,#19030,#19031);
#15484=AXIS2_PLACEMENT_3D('',#57670,#19035,#19036);
#15485=AXIS2_PLACEMENT_3D('',#57676,#19040,#19041);
#15486=AXIS2_PLACEMENT_3D('',#57679,#19044,#19045);
#15487=AXIS2_PLACEMENT_3D('',#57680,#19046,#19047);
#15488=AXIS2_PLACEMENT_3D('',#57681,#19048,#19049);
#15489=AXIS2_PLACEMENT_3D('',#57683,#19050,#19051);
#15490=AXIS2_PLACEMENT_3D('',#57684,#19052,#19053);
#15491=AXIS2_PLACEMENT_3D('',#57686,#19054,#19055);
#15492=AXIS2_PLACEMENT_3D('',#57687,#19056,#19057);
#15493=AXIS2_PLACEMENT_3D('',#57689,#19058,#19059);
#15494=AXIS2_PLACEMENT_3D('',#57691,#19061,#19062);
#15495=AXIS2_PLACEMENT_3D('',#57693,#19063,#19064);
#15496=AXIS2_PLACEMENT_3D('',#57695,#19066,#19067);
#15497=AXIS2_PLACEMENT_3D('',#57697,#19068,#19069);
#15498=AXIS2_PLACEMENT_3D('',#57699,#19071,#19072);
#15499=AXIS2_PLACEMENT_3D('',#57701,#19073,#19074);
#15500=AXIS2_PLACEMENT_3D('',#57702,#19075,#19076);
#15501=AXIS2_PLACEMENT_3D('',#57704,#19077,#19078);
#15502=AXIS2_PLACEMENT_3D('',#57706,#19080,#19081);
#15503=AXIS2_PLACEMENT_3D('',#57708,#19083,#19084);
#15504=AXIS2_PLACEMENT_3D('',#57709,#19085,#19086);
#15505=AXIS2_PLACEMENT_3D('',#57710,#19087,#19088);
#15506=AXIS2_PLACEMENT_3D('',#57711,#19089,#19090);
#15507=AXIS2_PLACEMENT_3D('',#57712,#19091,#19092);
#15508=AXIS2_PLACEMENT_3D('',#57713,#19093,#19094);
#15509=AXIS2_PLACEMENT_3D('',#57714,#19095,#19096);
#15510=AXIS2_PLACEMENT_3D('',#57715,#19097,#19098);
#15511=AXIS2_PLACEMENT_3D('',#57716,#19099,#19100);
#15512=AXIS2_PLACEMENT_3D('',#57717,#19101,#19102);
#15513=AXIS2_PLACEMENT_3D('',#57718,#19103,#19104);
#15514=AXIS2_PLACEMENT_3D('',#57719,#19105,#19106);
#15515=AXIS2_PLACEMENT_3D('',#57720,#19107,#19108);
#15516=AXIS2_PLACEMENT_3D('',#57721,#19109,#19110);
#15517=AXIS2_PLACEMENT_3D('',#57722,#19111,#19112);
#15518=AXIS2_PLACEMENT_3D('',#57723,#19113,#19114);
#15519=AXIS2_PLACEMENT_3D('',#57724,#19115,#19116);
#15520=AXIS2_PLACEMENT_3D('',#57725,#19117,#19118);
#15521=AXIS2_PLACEMENT_3D('',#57726,#19119,#19120);
#15522=AXIS2_PLACEMENT_3D('',#57727,#19121,#19122);
#15523=AXIS2_PLACEMENT_3D('',#57728,#19123,#19124);
#15524=AXIS2_PLACEMENT_3D('',#57729,#19125,#19126);
#15525=AXIS2_PLACEMENT_3D('',#57730,#19127,#19128);
#15526=AXIS2_PLACEMENT_3D('',#57731,#19129,#19130);
#15527=AXIS2_PLACEMENT_3D('',#57732,#19131,#19132);
#15528=AXIS2_PLACEMENT_3D('',#57733,#19133,#19134);
#15529=AXIS2_PLACEMENT_3D('',#57734,#19135,#19136);
#15530=AXIS2_PLACEMENT_3D('',#57735,#19137,#19138);
#15531=AXIS2_PLACEMENT_3D('',#57736,#19139,#19140);
#15532=AXIS2_PLACEMENT_3D('',#57737,#19141,#19142);
#15533=AXIS2_PLACEMENT_3D('',#57738,#19143,#19144);
#15534=AXIS2_PLACEMENT_3D('',#57739,#19145,#19146);
#15535=AXIS2_PLACEMENT_3D('',#57740,#19147,#19148);
#15536=AXIS2_PLACEMENT_3D('',#57741,#19149,#19150);
#15537=AXIS2_PLACEMENT_3D('',#57742,#19151,#19152);
#15538=AXIS2_PLACEMENT_3D('',#57743,#19153,#19154);
#15539=AXIS2_PLACEMENT_3D('',#57744,#19155,#19156);
#15540=AXIS2_PLACEMENT_3D('',#57745,#19157,#19158);
#15541=AXIS2_PLACEMENT_3D('',#57746,#19159,#19160);
#15542=AXIS2_PLACEMENT_3D('',#57747,#19161,#19162);
#15543=AXIS2_PLACEMENT_3D('',#57748,#19163,#19164);
#15544=AXIS2_PLACEMENT_3D('',#57749,#19165,#19166);
#15545=AXIS2_PLACEMENT_3D('',#57750,#19167,#19168);
#15546=AXIS2_PLACEMENT_3D('',#57751,#19169,#19170);
#15547=AXIS2_PLACEMENT_3D('',#57752,#19171,#19172);
#15548=AXIS2_PLACEMENT_3D('',#57753,#19173,#19174);
#15549=AXIS2_PLACEMENT_3D('',#57754,#19175,#19176);
#15550=AXIS2_PLACEMENT_3D('',#57755,#19177,#19178);
#15551=AXIS2_PLACEMENT_3D('',#57756,#19179,#19180);
#15552=AXIS2_PLACEMENT_3D('',#57757,#19181,#19182);
#15553=AXIS2_PLACEMENT_3D('',#57758,#19183,#19184);
#15554=AXIS2_PLACEMENT_3D('',#57759,#19185,#19186);
#15555=AXIS2_PLACEMENT_3D('',#57760,#19187,#19188);
#15556=AXIS2_PLACEMENT_3D('',#57761,#19189,#19190);
#15557=AXIS2_PLACEMENT_3D('',#57762,#19191,#19192);
#15558=AXIS2_PLACEMENT_3D('',#57763,#19193,#19194);
#15559=AXIS2_PLACEMENT_3D('',#57764,#19195,#19196);
#15560=AXIS2_PLACEMENT_3D('',#57765,#19197,#19198);
#15561=AXIS2_PLACEMENT_3D('',#57766,#19199,#19200);
#15562=AXIS2_PLACEMENT_3D('',#57767,#19201,#19202);
#15563=AXIS2_PLACEMENT_3D('',#57768,#19203,#19204);
#15564=AXIS2_PLACEMENT_3D('',#57769,#19205,#19206);
#15565=AXIS2_PLACEMENT_3D('',#57770,#19207,#19208);
#15566=AXIS2_PLACEMENT_3D('',#57771,#19209,#19210);
#15567=AXIS2_PLACEMENT_3D('',#57772,#19211,#19212);
#15568=AXIS2_PLACEMENT_3D('',#57773,#19213,#19214);
#15569=AXIS2_PLACEMENT_3D('',#57774,#19215,#19216);
#15570=AXIS2_PLACEMENT_3D('',#57775,#19217,#19218);
#15571=AXIS2_PLACEMENT_3D('',#57776,#19219,#19220);
#15572=AXIS2_PLACEMENT_3D('',#57777,#19221,#19222);
#15573=AXIS2_PLACEMENT_3D('',#57778,#19223,#19224);
#15574=AXIS2_PLACEMENT_3D('',#57779,#19225,#19226);
#15575=AXIS2_PLACEMENT_3D('',#57780,#19227,#19228);
#15576=AXIS2_PLACEMENT_3D('',#57781,#19229,#19230);
#15577=AXIS2_PLACEMENT_3D('',#57782,#19231,#19232);
#15578=DIRECTION('axis',(0.,0.,1.));
#15579=DIRECTION('refdir',(1.,0.,0.));
#15580=DIRECTION('axis',(0.,0.,1.));
#15581=DIRECTION('refdir',(1.,0.,0.));
#15582=DIRECTION('axis',(0.,0.,1.));
#15583=DIRECTION('refdir',(1.,0.,0.));
#15584=DIRECTION('center_axis',(0.,0.,1.));
#15585=DIRECTION('ref_axis',(1.,0.,0.));
#15586=DIRECTION('center_axis',(0.,0.,1.));
#15587=DIRECTION('ref_axis',(1.,0.,0.));
#15588=DIRECTION('',(0.,0.,1.));
#15589=DIRECTION('center_axis',(0.,0.,-1.));
#15590=DIRECTION('ref_axis',(1.,0.,0.));
#15591=DIRECTION('center_axis',(0.,0.,1.));
#15592=DIRECTION('ref_axis',(1.,0.,0.));
#15593=DIRECTION('center_axis',(0.,0.,1.));
#15594=DIRECTION('ref_axis',(1.,0.,0.));
#15595=DIRECTION('',(0.,0.,1.));
#15596=DIRECTION('center_axis',(0.,0.,-1.));
#15597=DIRECTION('ref_axis',(1.,0.,0.));
#15598=DIRECTION('center_axis',(0.,0.,1.));
#15599=DIRECTION('ref_axis',(1.,0.,0.));
#15600=DIRECTION('center_axis',(0.,0.,1.));
#15601=DIRECTION('ref_axis',(1.,0.,0.));
#15602=DIRECTION('',(0.,0.,1.));
#15603=DIRECTION('center_axis',(0.,0.,-1.));
#15604=DIRECTION('ref_axis',(1.,0.,0.));
#15605=DIRECTION('center_axis',(0.,0.,1.));
#15606=DIRECTION('ref_axis',(1.,0.,0.));
#15607=DIRECTION('center_axis',(0.,0.,1.));
#15608=DIRECTION('ref_axis',(1.,0.,0.));
#15609=DIRECTION('',(0.,0.,1.));
#15610=DIRECTION('center_axis',(0.,0.,-1.));
#15611=DIRECTION('ref_axis',(1.,0.,0.));
#15612=DIRECTION('center_axis',(0.,0.,1.));
#15613=DIRECTION('ref_axis',(1.,0.,0.));
#15614=DIRECTION('center_axis',(0.,0.,1.));
#15615=DIRECTION('ref_axis',(1.,0.,0.));
#15616=DIRECTION('',(0.,0.,1.));
#15617=DIRECTION('center_axis',(0.,0.,-1.));
#15618=DIRECTION('ref_axis',(1.,0.,0.));
#15619=DIRECTION('center_axis',(0.,0.,1.));
#15620=DIRECTION('ref_axis',(1.,0.,0.));
#15621=DIRECTION('center_axis',(0.,0.,1.));
#15622=DIRECTION('ref_axis',(1.,0.,0.));
#15623=DIRECTION('',(0.,0.,1.));
#15624=DIRECTION('center_axis',(0.,0.,-1.));
#15625=DIRECTION('ref_axis',(1.,0.,0.));
#15626=DIRECTION('center_axis',(0.,0.,1.));
#15627=DIRECTION('ref_axis',(1.,0.,0.));
#15628=DIRECTION('center_axis',(0.,0.,1.));
#15629=DIRECTION('ref_axis',(1.,0.,0.));
#15630=DIRECTION('',(0.,0.,1.));
#15631=DIRECTION('center_axis',(0.,0.,-1.));
#15632=DIRECTION('ref_axis',(1.,0.,0.));
#15633=DIRECTION('center_axis',(0.,0.,1.));
#15634=DIRECTION('ref_axis',(1.,0.,0.));
#15635=DIRECTION('center_axis',(0.,0.,1.));
#15636=DIRECTION('ref_axis',(1.,0.,0.));
#15637=DIRECTION('',(0.,0.,1.));
#15638=DIRECTION('center_axis',(0.,0.,-1.));
#15639=DIRECTION('ref_axis',(1.,0.,0.));
#15640=DIRECTION('center_axis',(0.,0.,1.));
#15641=DIRECTION('ref_axis',(1.,0.,0.));
#15642=DIRECTION('center_axis',(0.,0.,1.));
#15643=DIRECTION('ref_axis',(1.,0.,0.));
#15644=DIRECTION('',(0.,0.,1.));
#15645=DIRECTION('center_axis',(0.,0.,-1.));
#15646=DIRECTION('ref_axis',(1.,0.,0.));
#15647=DIRECTION('center_axis',(0.,0.,1.));
#15648=DIRECTION('ref_axis',(1.,0.,0.));
#15649=DIRECTION('center_axis',(0.,0.,1.));
#15650=DIRECTION('ref_axis',(1.,0.,0.));
#15651=DIRECTION('',(0.,0.,1.));
#15652=DIRECTION('center_axis',(0.,0.,-1.));
#15653=DIRECTION('ref_axis',(1.,0.,0.));
#15654=DIRECTION('center_axis',(0.,0.,1.));
#15655=DIRECTION('ref_axis',(1.,0.,0.));
#15656=DIRECTION('center_axis',(0.,0.,1.));
#15657=DIRECTION('ref_axis',(1.,0.,0.));
#15658=DIRECTION('',(0.,0.,1.));
#15659=DIRECTION('center_axis',(0.,0.,-1.));
#15660=DIRECTION('ref_axis',(1.,0.,0.));
#15661=DIRECTION('center_axis',(0.,0.,1.));
#15662=DIRECTION('ref_axis',(1.,0.,0.));
#15663=DIRECTION('center_axis',(0.,0.,1.));
#15664=DIRECTION('ref_axis',(1.,0.,0.));
#15665=DIRECTION('',(0.,0.,1.));
#15666=DIRECTION('center_axis',(0.,0.,-1.));
#15667=DIRECTION('ref_axis',(1.,0.,0.));
#15668=DIRECTION('center_axis',(0.,1.,0.));
#15669=DIRECTION('ref_axis',(-1.,0.,0.));
#15670=DIRECTION('',(-1.,0.,0.));
#15671=DIRECTION('',(0.,0.,1.));
#15672=DIRECTION('',(-1.,0.,0.));
#15673=DIRECTION('',(0.,0.,1.));
#15674=DIRECTION('center_axis',(1.,0.,0.));
#15675=DIRECTION('ref_axis',(0.,1.,0.));
#15676=DIRECTION('',(0.,1.,0.));
#15677=DIRECTION('',(0.,1.,0.));
#15678=DIRECTION('',(0.,0.,1.));
#15679=DIRECTION('center_axis',(0.,-1.,0.));
#15680=DIRECTION('ref_axis',(1.,0.,0.));
#15681=DIRECTION('',(1.,0.,0.));
#15682=DIRECTION('',(1.,0.,0.));
#15683=DIRECTION('',(0.,0.,1.));
#15684=DIRECTION('center_axis',(-1.,0.,0.));
#15685=DIRECTION('ref_axis',(0.,-1.,0.));
#15686=DIRECTION('',(0.,-1.,0.));
#15687=DIRECTION('',(0.,-1.,0.));
#15688=DIRECTION('center_axis',(0.,0.,1.));
#15689=DIRECTION('ref_axis',(1.,0.,0.));
#15690=DIRECTION('center_axis',(0.,0.,1.));
#15691=DIRECTION('ref_axis',(1.,0.,0.));
#15692=DIRECTION('axis',(0.,0.,1.));
#15693=DIRECTION('refdir',(1.,0.,0.));
#15694=DIRECTION('center_axis',(0.,1.,0.));
#15695=DIRECTION('ref_axis',(-1.,0.,0.));
#15696=DIRECTION('',(-1.,0.,0.));
#15697=DIRECTION('',(0.,0.,1.));
#15698=DIRECTION('',(-1.,0.,0.));
#15699=DIRECTION('',(0.,0.,1.));
#15700=DIRECTION('center_axis',(1.,0.,0.));
#15701=DIRECTION('ref_axis',(0.,1.,0.));
#15702=DIRECTION('',(0.,1.,0.));
#15703=DIRECTION('',(0.,1.,0.));
#15704=DIRECTION('',(0.,0.,1.));
#15705=DIRECTION('center_axis',(0.,-1.,0.));
#15706=DIRECTION('ref_axis',(1.,0.,0.));
#15707=DIRECTION('',(1.,0.,0.));
#15708=DIRECTION('',(1.,0.,0.));
#15709=DIRECTION('',(0.,0.,1.));
#15710=DIRECTION('center_axis',(-1.,0.,0.));
#15711=DIRECTION('ref_axis',(0.,-1.,0.));
#15712=DIRECTION('',(0.,-1.,0.));
#15713=DIRECTION('',(0.,-1.,0.));
#15714=DIRECTION('center_axis',(0.,0.,1.));
#15715=DIRECTION('ref_axis',(1.,0.,0.));
#15716=DIRECTION('center_axis',(0.,0.,1.));
#15717=DIRECTION('ref_axis',(1.,0.,0.));
#15718=DIRECTION('axis',(0.,0.,1.));
#15719=DIRECTION('refdir',(1.,0.,0.));
#15720=DIRECTION('center_axis',(0.,1.,0.));
#15721=DIRECTION('ref_axis',(-1.,0.,0.));
#15722=DIRECTION('',(-1.,0.,0.));
#15723=DIRECTION('',(0.,0.,1.));
#15724=DIRECTION('',(-1.,0.,0.));
#15725=DIRECTION('',(0.,0.,1.));
#15726=DIRECTION('center_axis',(1.,0.,0.));
#15727=DIRECTION('ref_axis',(0.,1.,0.));
#15728=DIRECTION('',(0.,1.,0.));
#15729=DIRECTION('',(0.,1.,0.));
#15730=DIRECTION('',(0.,0.,1.));
#15731=DIRECTION('center_axis',(0.,-1.,0.));
#15732=DIRECTION('ref_axis',(1.,0.,0.));
#15733=DIRECTION('',(1.,0.,0.));
#15734=DIRECTION('',(1.,0.,0.));
#15735=DIRECTION('',(0.,0.,1.));
#15736=DIRECTION('center_axis',(-1.,0.,0.));
#15737=DIRECTION('ref_axis',(0.,-1.,0.));
#15738=DIRECTION('',(0.,-1.,0.));
#15739=DIRECTION('',(0.,-1.,0.));
#15740=DIRECTION('center_axis',(0.,0.,1.));
#15741=DIRECTION('ref_axis',(1.,0.,0.));
#15742=DIRECTION('center_axis',(0.,0.,1.));
#15743=DIRECTION('ref_axis',(1.,0.,0.));
#15744=DIRECTION('axis',(0.,0.,1.));
#15745=DIRECTION('refdir',(1.,0.,0.));
#15746=DIRECTION('center_axis',(1.,0.,0.));
#15747=DIRECTION('ref_axis',(0.,0.,-1.));
#15748=DIRECTION('',(1.,0.,0.));
#15749=DIRECTION('center_axis',(0.,0.,1.));
#15750=DIRECTION('ref_axis',(1.,0.,0.));
#15751=DIRECTION('center_axis',(0.,0.,1.));
#15752=DIRECTION('ref_axis',(1.,0.,0.));
#15753=DIRECTION('',(0.,0.,1.));
#15754=DIRECTION('center_axis',(0.,0.,-1.));
#15755=DIRECTION('ref_axis',(1.,0.,0.));
#15756=DIRECTION('center_axis',(0.,0.,1.));
#15757=DIRECTION('ref_axis',(1.,0.,0.));
#15758=DIRECTION('center_axis',(0.,0.,1.));
#15759=DIRECTION('ref_axis',(1.,0.,0.));
#15760=DIRECTION('center_axis',(0.,0.,1.));
#15761=DIRECTION('ref_axis',(1.,0.,0.));
#15762=DIRECTION('',(0.,0.,1.));
#15763=DIRECTION('center_axis',(0.,0.,-1.));
#15764=DIRECTION('ref_axis',(1.,0.,0.));
#15765=DIRECTION('center_axis',(0.,0.,1.));
#15766=DIRECTION('ref_axis',(1.,0.,0.));
#15767=DIRECTION('center_axis',(0.,0.,1.));
#15768=DIRECTION('ref_axis',(1.,0.,0.));
#15769=DIRECTION('center_axis',(0.,0.,1.));
#15770=DIRECTION('ref_axis',(1.,0.,0.));
#15771=DIRECTION('',(0.,0.,1.));
#15772=DIRECTION('center_axis',(0.,0.,-1.));
#15773=DIRECTION('ref_axis',(1.,0.,0.));
#15774=DIRECTION('center_axis',(0.,0.,1.));
#15775=DIRECTION('ref_axis',(1.,0.,0.));
#15776=DIRECTION('center_axis',(0.,0.,1.));
#15777=DIRECTION('ref_axis',(1.,0.,0.));
#15778=DIRECTION('center_axis',(0.,0.,1.));
#15779=DIRECTION('ref_axis',(1.,0.,0.));
#15780=DIRECTION('',(0.,0.,1.));
#15781=DIRECTION('center_axis',(0.,0.,-1.));
#15782=DIRECTION('ref_axis',(1.,0.,0.));
#15783=DIRECTION('center_axis',(0.,0.,1.));
#15784=DIRECTION('ref_axis',(1.,0.,0.));
#15785=DIRECTION('center_axis',(0.,0.,1.));
#15786=DIRECTION('ref_axis',(1.,0.,0.));
#15787=DIRECTION('center_axis',(0.,0.,1.));
#15788=DIRECTION('ref_axis',(1.,0.,0.));
#15789=DIRECTION('center_axis',(0.,0.,1.));
#15790=DIRECTION('ref_axis',(1.,0.,0.));
#15791=DIRECTION('center_axis',(0.,0.,1.));
#15792=DIRECTION('ref_axis',(1.,0.,0.));
#15793=DIRECTION('',(0.,0.,1.));
#15794=DIRECTION('center_axis',(0.,0.,1.));
#15795=DIRECTION('ref_axis',(1.,0.,0.));
#15796=DIRECTION('',(0.,0.,-1.));
#15797=DIRECTION('center_axis',(0.,0.,1.));
#15798=DIRECTION('ref_axis',(1.,0.,0.));
#15799=DIRECTION('',(0.,0.,-1.));
#15800=DIRECTION('center_axis',(0.,0.,1.));
#15801=DIRECTION('ref_axis',(1.,0.,0.));
#15802=DIRECTION('',(0.,0.,1.));
#15803=DIRECTION('center_axis',(0.,0.,1.));
#15804=DIRECTION('ref_axis',(1.,0.,0.));
#15805=DIRECTION('center_axis',(0.,0.,1.));
#15806=DIRECTION('ref_axis',(1.,0.,0.));
#15807=DIRECTION('center_axis',(0.,0.,1.));
#15808=DIRECTION('ref_axis',(1.,0.,0.));
#15809=DIRECTION('center_axis',(0.,0.,1.));
#15810=DIRECTION('ref_axis',(-0.707106781186548,-0.707106781186547,0.));
#15811=DIRECTION('',(0.,0.,-1.));
#15812=DIRECTION('center_axis',(0.,0.,1.));
#15813=DIRECTION('ref_axis',(1.,0.,0.));
#15814=DIRECTION('',(0.,0.,1.));
#15815=DIRECTION('center_axis',(0.,0.,1.));
#15816=DIRECTION('ref_axis',(1.,0.,0.));
#15817=DIRECTION('center_axis',(0.,0.,1.));
#15818=DIRECTION('ref_axis',(1.,0.,0.));
#15819=DIRECTION('center_axis',(0.,0.,1.));
#15820=DIRECTION('ref_axis',(1.,0.,0.));
#15821=DIRECTION('center_axis',(0.,0.,1.));
#15822=DIRECTION('ref_axis',(-0.707106781186547,0.707106781186548,0.));
#15823=DIRECTION('',(0.,0.,-1.));
#15824=DIRECTION('center_axis',(0.,0.,1.));
#15825=DIRECTION('ref_axis',(1.,0.,0.));
#15826=DIRECTION('',(0.,0.,1.));
#15827=DIRECTION('center_axis',(0.,0.,1.));
#15828=DIRECTION('ref_axis',(1.,0.,0.));
#15829=DIRECTION('center_axis',(0.,0.,1.));
#15830=DIRECTION('ref_axis',(1.,0.,0.));
#15831=DIRECTION('center_axis',(0.,0.,1.));
#15832=DIRECTION('ref_axis',(1.,0.,0.));
#15833=DIRECTION('center_axis',(0.,0.,1.));
#15834=DIRECTION('ref_axis',(1.,0.,0.));
#15835=DIRECTION('center_axis',(0.,0.,1.));
#15836=DIRECTION('ref_axis',(1.,0.,0.));
#15837=DIRECTION('',(0.,0.,-1.));
#15838=DIRECTION('center_axis',(0.,0.,1.));
#15839=DIRECTION('ref_axis',(1.,0.,0.));
#15840=DIRECTION('center_axis',(0.,0.,1.));
#15841=DIRECTION('ref_axis',(1.,0.,0.));
#15842=DIRECTION('center_axis',(0.,0.,1.));
#15843=DIRECTION('ref_axis',(1.,0.,0.));
#15844=DIRECTION('center_axis',(0.,0.,1.));
#15845=DIRECTION('ref_axis',(1.,0.,0.));
#15846=DIRECTION('center_axis',(0.,0.,1.));
#15847=DIRECTION('ref_axis',(1.,0.,0.));
#15848=DIRECTION('center_axis',(0.,0.,1.));
#15849=DIRECTION('ref_axis',(1.,0.,0.));
#15850=DIRECTION('center_axis',(0.,0.,1.));
#15851=DIRECTION('ref_axis',(1.,0.,0.));
#15852=DIRECTION('center_axis',(0.,0.,-1.));
#15853=DIRECTION('ref_axis',(1.,0.,0.));
#15854=DIRECTION('center_axis',(0.,0.,-1.));
#15855=DIRECTION('ref_axis',(1.,0.,0.));
#15856=DIRECTION('center_axis',(0.,0.,-1.));
#15857=DIRECTION('ref_axis',(1.,0.,0.));
#15858=DIRECTION('center_axis',(0.,0.,-1.));
#15859=DIRECTION('ref_axis',(1.,0.,0.));
#15860=DIRECTION('center_axis',(0.,0.,1.));
#15861=DIRECTION('ref_axis',(1.,0.,0.));
#15862=DIRECTION('center_axis',(0.,0.,1.));
#15863=DIRECTION('ref_axis',(1.,0.,0.));
#15864=DIRECTION('',(0.,0.,1.));
#15865=DIRECTION('center_axis',(0.,0.,1.));
#15866=DIRECTION('ref_axis',(1.,0.,0.));
#15867=DIRECTION('center_axis',(0.,0.,1.));
#15868=DIRECTION('ref_axis',(1.,0.,0.));
#15869=DIRECTION('',(0.,0.,1.));
#15870=DIRECTION('center_axis',(0.,0.,1.));
#15871=DIRECTION('ref_axis',(1.,0.,0.));
#15872=DIRECTION('center_axis',(0.,0.,1.));
#15873=DIRECTION('ref_axis',(1.,0.,0.));
#15874=DIRECTION('',(0.,0.,1.));
#15875=DIRECTION('center_axis',(0.,0.,1.));
#15876=DIRECTION('ref_axis',(1.,0.,0.));
#15877=DIRECTION('center_axis',(0.,0.,1.));
#15878=DIRECTION('ref_axis',(1.,0.,0.));
#15879=DIRECTION('',(0.,0.,1.));
#15880=DIRECTION('center_axis',(0.,0.,1.));
#15881=DIRECTION('ref_axis',(1.,0.,0.));
#15882=DIRECTION('center_axis',(0.,0.,1.));
#15883=DIRECTION('ref_axis',(1.,0.,0.));
#15884=DIRECTION('',(0.,0.,1.));
#15885=DIRECTION('center_axis',(0.,0.,-1.));
#15886=DIRECTION('ref_axis',(1.,0.,0.));
#15887=DIRECTION('center_axis',(0.,0.,1.));
#15888=DIRECTION('ref_axis',(1.,0.,0.));
#15889=DIRECTION('center_axis',(0.,0.,1.));
#15890=DIRECTION('ref_axis',(1.,0.,0.));
#15891=DIRECTION('center_axis',(0.,0.,1.));
#15892=DIRECTION('ref_axis',(1.,0.,0.));
#15893=DIRECTION('',(0.,0.,-1.));
#15894=DIRECTION('center_axis',(0.,0.,1.));
#15895=DIRECTION('ref_axis',(1.,0.,0.));
#15896=DIRECTION('center_axis',(0.,0.,1.));
#15897=DIRECTION('ref_axis',(1.,0.,0.));
#15898=DIRECTION('',(0.,0.,-1.));
#15899=DIRECTION('center_axis',(0.,0.,-1.));
#15900=DIRECTION('ref_axis',(1.,0.,0.));
#15901=DIRECTION('center_axis',(0.,0.,1.));
#15902=DIRECTION('ref_axis',(1.,0.,0.));
#15903=DIRECTION('center_axis',(0.,0.,1.));
#15904=DIRECTION('ref_axis',(1.,0.,0.));
#15905=DIRECTION('axis',(0.,0.,1.));
#15906=DIRECTION('refdir',(1.,0.,0.));
#15907=DIRECTION('center_axis',(0.,0.,1.));
#15908=DIRECTION('ref_axis',(1.,0.,0.));
#15909=DIRECTION('center_axis',(0.,0.,-1.));
#15910=DIRECTION('ref_axis',(1.,0.,0.));
#15911=DIRECTION('',(0.,0.,-1.));
#15912=DIRECTION('center_axis',(0.,0.,-1.));
#15913=DIRECTION('ref_axis',(1.,0.,0.));
#15914=DIRECTION('center_axis',(0.,0.,1.));
#15915=DIRECTION('ref_axis',(1.,0.,0.));
#15916=DIRECTION('center_axis',(0.,0.,1.));
#15917=DIRECTION('ref_axis',(1.,0.,0.));
#15918=DIRECTION('',(0.,0.,-1.));
#15919=DIRECTION('center_axis',(0.,0.,1.));
#15920=DIRECTION('ref_axis',(1.,0.,0.));
#15921=DIRECTION('center_axis',(0.,0.,1.));
#15922=DIRECTION('ref_axis',(1.,0.,0.));
#15923=DIRECTION('center_axis',(0.,0.,1.));
#15924=DIRECTION('ref_axis',(1.,0.,0.));
#15925=DIRECTION('axis',(0.,0.,1.));
#15926=DIRECTION('refdir',(1.,0.,0.));
#15927=DIRECTION('center_axis',(0.,0.,1.));
#15928=DIRECTION('ref_axis',(0.707106781186547,0.707106781186548,0.));
#15929=DIRECTION('',(0.,0.,1.));
#15930=DIRECTION('center_axis',(0.,0.,1.));
#15931=DIRECTION('ref_axis',(1.,0.,0.));
#15932=DIRECTION('',(0.,0.,-1.));
#15933=DIRECTION('center_axis',(0.,0.,-1.));
#15934=DIRECTION('ref_axis',(1.,0.,0.));
#15935=DIRECTION('center_axis',(0.,0.,1.));
#15936=DIRECTION('ref_axis',(0.707106781186548,-0.707106781186547,0.));
#15937=DIRECTION('',(0.,0.,1.));
#15938=DIRECTION('center_axis',(0.,0.,1.));
#15939=DIRECTION('ref_axis',(1.,0.,0.));
#15940=DIRECTION('',(0.,0.,-1.));
#15941=DIRECTION('center_axis',(0.,0.,-1.));
#15942=DIRECTION('ref_axis',(1.,0.,0.));
#15943=DIRECTION('center_axis',(0.,0.,1.));
#15944=DIRECTION('ref_axis',(-0.707106781186547,-0.707106781186548,0.));
#15945=DIRECTION('',(0.,0.,1.));
#15946=DIRECTION('center_axis',(0.,0.,1.));
#15947=DIRECTION('ref_axis',(1.,0.,0.));
#15948=DIRECTION('',(0.,0.,-1.));
#15949=DIRECTION('center_axis',(0.,0.,-1.));
#15950=DIRECTION('ref_axis',(1.,0.,0.));
#15951=DIRECTION('center_axis',(0.,0.,1.));
#15952=DIRECTION('ref_axis',(-0.707106781186548,0.707106781186547,0.));
#15953=DIRECTION('',(0.,0.,1.));
#15954=DIRECTION('center_axis',(0.,0.,1.));
#15955=DIRECTION('ref_axis',(1.,0.,0.));
#15956=DIRECTION('',(0.,0.,-1.));
#15957=DIRECTION('center_axis',(0.,0.,-1.));
#15958=DIRECTION('ref_axis',(1.,0.,0.));
#15959=DIRECTION('center_axis',(0.,0.,1.));
#15960=DIRECTION('ref_axis',(1.,0.,0.));
#15961=DIRECTION('center_axis',(0.,0.,1.));
#15962=DIRECTION('ref_axis',(1.,0.,0.));
#15963=DIRECTION('center_axis',(0.,0.,1.));
#15964=DIRECTION('ref_axis',(1.,0.,0.));
#15965=DIRECTION('center_axis',(0.,0.,1.));
#15966=DIRECTION('ref_axis',(1.,0.,0.));
#15967=DIRECTION('center_axis',(0.,0.,1.));
#15968=DIRECTION('ref_axis',(1.,0.,0.));
#15969=DIRECTION('center_axis',(0.,0.,1.));
#15970=DIRECTION('ref_axis',(1.,0.,0.));
#15971=DIRECTION('center_axis',(0.,0.,1.));
#15972=DIRECTION('ref_axis',(1.,0.,0.));
#15973=DIRECTION('center_axis',(0.,0.,1.));
#15974=DIRECTION('ref_axis',(1.,0.,0.));
#15975=DIRECTION('center_axis',(0.,0.,1.));
#15976=DIRECTION('ref_axis',(1.,0.,0.));
#15977=DIRECTION('center_axis',(0.,0.,1.));
#15978=DIRECTION('ref_axis',(1.,0.,0.));
#15979=DIRECTION('center_axis',(0.,0.,1.));
#15980=DIRECTION('ref_axis',(-1.,-1.22464679914735E-16,0.));
#15981=DIRECTION('center_axis',(0.,0.,1.));
#15982=DIRECTION('ref_axis',(1.,0.,0.));
#15983=DIRECTION('center_axis',(0.,0.,1.));
#15984=DIRECTION('ref_axis',(1.,0.,0.));
#15985=DIRECTION('center_axis',(0.,0.,1.));
#15986=DIRECTION('ref_axis',(1.,0.,0.));
#15987=DIRECTION('center_axis',(0.,0.,1.));
#15988=DIRECTION('ref_axis',(1.,0.,0.));
#15989=DIRECTION('',(0.,0.,-1.));
#15990=DIRECTION('center_axis',(0.,0.,1.));
#15991=DIRECTION('ref_axis',(1.,0.,0.));
#15992=DIRECTION('center_axis',(0.,0.,1.));
#15993=DIRECTION('ref_axis',(1.,0.,0.));
#15994=DIRECTION('center_axis',(0.,0.,-1.));
#15995=DIRECTION('ref_axis',(1.,0.,0.));
#15996=DIRECTION('center_axis',(0.,0.,1.));
#15997=DIRECTION('ref_axis',(1.,0.,0.));
#15998=DIRECTION('center_axis',(0.,0.,-1.));
#15999=DIRECTION('ref_axis',(1.,0.,0.));
#16000=DIRECTION('',(0.,0.,-1.));
#16001=DIRECTION('center_axis',(0.,0.,1.));
#16002=DIRECTION('ref_axis',(1.,0.,0.));
#16003=DIRECTION('axis',(0.,0.,1.));
#16004=DIRECTION('refdir',(1.,0.,0.));
#16005=DIRECTION('center_axis',(0.,0.,1.));
#16006=DIRECTION('ref_axis',(1.,0.,0.));
#16007=DIRECTION('center_axis',(0.,0.,1.));
#16008=DIRECTION('ref_axis',(1.,0.,0.));
#16009=DIRECTION('',(0.,0.,1.));
#16010=DIRECTION('center_axis',(0.,0.,-1.));
#16011=DIRECTION('ref_axis',(1.,0.,0.));
#16012=DIRECTION('center_axis',(0.,0.,1.));
#16013=DIRECTION('ref_axis',(1.,0.,0.));
#16014=DIRECTION('center_axis',(0.,0.,1.));
#16015=DIRECTION('ref_axis',(1.,0.,0.));
#16016=DIRECTION('',(0.,0.,1.));
#16017=DIRECTION('center_axis',(0.,0.,-1.));
#16018=DIRECTION('ref_axis',(1.,0.,0.));
#16019=DIRECTION('center_axis',(0.,0.,1.));
#16020=DIRECTION('ref_axis',(1.,0.,0.));
#16021=DIRECTION('center_axis',(0.,0.,1.));
#16022=DIRECTION('ref_axis',(1.,0.,0.));
#16023=DIRECTION('',(0.,0.,1.));
#16024=DIRECTION('center_axis',(0.,0.,-1.));
#16025=DIRECTION('ref_axis',(1.,0.,0.));
#16026=DIRECTION('center_axis',(0.,0.,1.));
#16027=DIRECTION('ref_axis',(1.,0.,0.));
#16028=DIRECTION('center_axis',(0.,0.,1.));
#16029=DIRECTION('ref_axis',(1.,0.,0.));
#16030=DIRECTION('',(0.,0.,1.));
#16031=DIRECTION('center_axis',(0.,0.,-1.));
#16032=DIRECTION('ref_axis',(1.,0.,0.));
#16033=DIRECTION('center_axis',(0.,0.,1.));
#16034=DIRECTION('ref_axis',(1.,0.,0.));
#16035=DIRECTION('center_axis',(0.,0.,1.));
#16036=DIRECTION('ref_axis',(1.,0.,0.));
#16037=DIRECTION('',(0.,0.,-1.));
#16038=DIRECTION('center_axis',(0.,0.,-1.));
#16039=DIRECTION('ref_axis',(1.,0.,0.));
#16040=DIRECTION('center_axis',(0.,0.,1.));
#16041=DIRECTION('ref_axis',(1.,0.,0.));
#16042=DIRECTION('center_axis',(0.,0.,1.));
#16043=DIRECTION('ref_axis',(1.,0.,0.));
#16044=DIRECTION('center_axis',(0.,0.,1.));
#16045=DIRECTION('ref_axis',(1.,0.,0.));
#16046=DIRECTION('',(0.,0.,-1.));
#16047=DIRECTION('center_axis',(0.,0.,1.));
#16048=DIRECTION('ref_axis',(1.,0.,0.));
#16049=DIRECTION('center_axis',(0.,0.,1.));
#16050=DIRECTION('ref_axis',(1.,0.,0.));
#16051=DIRECTION('center_axis',(0.,0.,1.));
#16052=DIRECTION('ref_axis',(1.,0.,0.));
#16053=DIRECTION('axis',(0.,0.,1.));
#16054=DIRECTION('refdir',(1.,0.,0.));
#16055=DIRECTION('center_axis',(1.,0.,0.));
#16056=DIRECTION('ref_axis',(0.,0.,-1.));
#16057=DIRECTION('',(0.,0.,1.));
#16058=DIRECTION('center_axis',(1.,0.,0.));
#16059=DIRECTION('ref_axis',(0.,0.,-1.));
#16060=DIRECTION('center_axis',(1.,0.,0.));
#16061=DIRECTION('ref_axis',(0.,0.,-1.));
#16062=DIRECTION('center_axis',(1.,0.,0.));
#16063=DIRECTION('ref_axis',(0.,0.,-1.));
#16064=DIRECTION('',(1.,0.,0.));
#16065=DIRECTION('center_axis',(-1.,0.,0.));
#16066=DIRECTION('ref_axis',(0.,0.,-1.));
#16067=DIRECTION('center_axis',(1.,0.,0.));
#16068=DIRECTION('ref_axis',(0.,0.,-1.));
#16069=DIRECTION('',(0.,0.,-1.));
#16070=DIRECTION('center_axis',(0.,1.,0.));
#16071=DIRECTION('ref_axis',(1.,0.,0.));
#16072=DIRECTION('',(0.,1.,0.));
#16073=DIRECTION('center_axis',(0.,1.,0.));
#16074=DIRECTION('ref_axis',(1.,0.,0.));
#16075=DIRECTION('',(0.,-1.,0.));
#16076=DIRECTION('center_axis',(0.,1.,0.));
#16077=DIRECTION('ref_axis',(1.,0.,0.));
#16078=DIRECTION('',(0.,1.,0.));
#16079=DIRECTION('center_axis',(0.,-1.,0.));
#16080=DIRECTION('ref_axis',(1.,0.,0.));
#16081=DIRECTION('',(0.,-1.,0.));
#16082=DIRECTION('center_axis',(0.,-1.,0.));
#16083=DIRECTION('ref_axis',(1.,0.,0.));
#16084=DIRECTION('',(0.,1.,0.));
#16085=DIRECTION('',(0.,1.,0.));
#16086=DIRECTION('center_axis',(0.,-1.,0.));
#16087=DIRECTION('ref_axis',(1.,0.,0.));
#16088=DIRECTION('',(0.,1.,0.));
#16089=DIRECTION('',(0.,1.,0.));
#16090=DIRECTION('center_axis',(0.,-1.,0.));
#16091=DIRECTION('ref_axis',(1.,0.,0.));
#16092=DIRECTION('',(0.,1.,0.));
#16093=DIRECTION('center_axis',(0.,-1.,0.));
#16094=DIRECTION('ref_axis',(1.,0.,0.));
#16095=DIRECTION('center_axis',(0.,1.,0.));
#16096=DIRECTION('ref_axis',(1.,0.,0.));
#16097=DIRECTION('',(0.,1.,0.));
#16098=DIRECTION('center_axis',(0.,1.,0.));
#16099=DIRECTION('ref_axis',(1.,0.,0.));
#16100=DIRECTION('',(0.,1.,0.));
#16101=DIRECTION('',(0.,1.,0.));
#16102=DIRECTION('center_axis',(0.,1.,0.));
#16103=DIRECTION('ref_axis',(1.,0.,0.));
#16104=DIRECTION('',(0.,1.,0.));
#16105=DIRECTION('center_axis',(0.,1.,0.));
#16106=DIRECTION('ref_axis',(1.,0.,0.));
#16107=DIRECTION('',(0.,0.,-1.));
#16108=DIRECTION('',(-1.,0.,0.));
#16109=DIRECTION('',(-1.,0.,0.));
#16110=DIRECTION('center_axis',(0.,1.,0.));
#16111=DIRECTION('ref_axis',(1.,0.,0.));
#16112=DIRECTION('',(1.,0.,0.));
#16113=DIRECTION('',(1.,0.,0.));
#16114=DIRECTION('',(0.,0.,-1.));
#16115=DIRECTION('center_axis',(-1.,0.,0.));
#16116=DIRECTION('ref_axis',(0.,-1.,0.));
#16117=DIRECTION('',(0.,0.,1.));
#16118=DIRECTION('',(0.,-1.,0.));
#16119=DIRECTION('center_axis',(0.,-1.,0.));
#16120=DIRECTION('ref_axis',(1.,0.,0.));
#16121=DIRECTION('',(1.,0.,0.));
#16122=DIRECTION('center_axis',(0.,-1.,0.));
#16123=DIRECTION('ref_axis',(1.,0.,0.));
#16124=DIRECTION('',(1.,0.,0.));
#16125=DIRECTION('',(0.,0.,1.));
#16126=DIRECTION('',(1.,0.,0.));
#16127=DIRECTION('center_axis',(0.,0.,1.));
#16128=DIRECTION('ref_axis',(1.,0.,0.));
#16129=DIRECTION('',(-1.,0.,0.));
#16130=DIRECTION('',(0.,-1.,0.));
#16131=DIRECTION('',(-1.,0.,0.));
#16132=DIRECTION('center_axis',(0.,0.,1.));
#16133=DIRECTION('ref_axis',(1.,0.,0.));
#16134=DIRECTION('',(1.,0.,0.));
#16135=DIRECTION('',(0.,-1.,0.));
#16136=DIRECTION('center_axis',(-1.,0.,0.));
#16137=DIRECTION('ref_axis',(0.,-1.,0.));
#16138=DIRECTION('',(0.,0.,1.));
#16139=DIRECTION('',(0.,-1.,0.));
#16140=DIRECTION('',(0.,0.,1.));
#16141=DIRECTION('center_axis',(-1.,0.,0.));
#16142=DIRECTION('ref_axis',(0.,-1.,0.));
#16143=DIRECTION('',(0.,0.,1.));
#16144=DIRECTION('',(0.,0.,1.));
#16145=DIRECTION('center_axis',(0.,1.,0.));
#16146=DIRECTION('ref_axis',(-1.,0.,0.));
#16147=DIRECTION('',(-1.,0.,0.));
#16148=DIRECTION('',(0.,0.,1.));
#16149=DIRECTION('',(-1.,0.,0.));
#16150=DIRECTION('center_axis',(0.,1.,0.));
#16151=DIRECTION('ref_axis',(-1.,0.,0.));
#16152=DIRECTION('',(-1.,0.,0.));
#16153=DIRECTION('center_axis',(0.,1.,0.));
#16154=DIRECTION('ref_axis',(-1.,0.,0.));
#16155=DIRECTION('center_axis',(0.,0.,1.));
#16156=DIRECTION('ref_axis',(1.,0.,0.));
#16157=DIRECTION('',(1.,0.,0.));
#16158=DIRECTION('center_axis',(0.,0.,1.));
#16159=DIRECTION('ref_axis',(1.,0.,0.));
#16160=DIRECTION('',(0.,1.,0.));
#16161=DIRECTION('',(1.,0.,0.));
#16162=DIRECTION('',(0.,-1.,0.));
#16163=DIRECTION('center_axis',(0.,0.,-1.));
#16164=DIRECTION('ref_axis',(1.,0.,0.));
#16165=DIRECTION('center_axis',(0.,0.,1.));
#16166=DIRECTION('ref_axis',(1.,0.,0.));
#16167=DIRECTION('center_axis',(0.,0.,1.));
#16168=DIRECTION('ref_axis',(1.,0.,0.));
#16169=DIRECTION('',(0.,0.,1.));
#16170=DIRECTION('center_axis',(0.,1.,0.));
#16171=DIRECTION('ref_axis',(-1.,0.,-1.22464679914735E-16));
#16172=DIRECTION('',(0.,1.,0.));
#16173=DIRECTION('center_axis',(0.,1.,0.));
#16174=DIRECTION('ref_axis',(1.,0.,0.));
#16175=DIRECTION('center_axis',(0.,1.,0.));
#16176=DIRECTION('ref_axis',(1.,0.,0.));
#16177=DIRECTION('',(-1.,0.,0.));
#16178=DIRECTION('center_axis',(0.,0.,1.));
#16179=DIRECTION('ref_axis',(1.,0.,0.));
#16180=DIRECTION('center_axis',(-1.,0.,0.));
#16181=DIRECTION('ref_axis',(0.,-1.,0.));
#16182=DIRECTION('',(0.,0.,1.));
#16183=DIRECTION('center_axis',(1.,0.,0.));
#16184=DIRECTION('ref_axis',(0.,1.,0.));
#16185=DIRECTION('',(0.,1.,0.));
#16186=DIRECTION('center_axis',(0.,-1.,0.));
#16187=DIRECTION('ref_axis',(1.,0.,0.));
#16188=DIRECTION('center_axis',(0.,0.,1.));
#16189=DIRECTION('ref_axis',(1.,0.,0.));
#16190=DIRECTION('axis',(0.,0.,1.));
#16191=DIRECTION('refdir',(1.,0.,0.));
#16192=DIRECTION('center_axis',(0.,1.,0.));
#16193=DIRECTION('ref_axis',(1.,0.,0.));
#16194=DIRECTION('center_axis',(0.,-1.,0.));
#16195=DIRECTION('ref_axis',(1.,0.,0.));
#16196=DIRECTION('',(0.,-1.,0.));
#16197=DIRECTION('center_axis',(0.,-1.,0.));
#16198=DIRECTION('ref_axis',(1.,0.,0.));
#16199=DIRECTION('center_axis',(0.,1.,0.));
#16200=DIRECTION('ref_axis',(1.,0.,0.));
#16201=DIRECTION('center_axis',(0.,1.,0.));
#16202=DIRECTION('ref_axis',(1.,0.,0.));
#16203=DIRECTION('',(0.,-1.,0.));
#16204=DIRECTION('center_axis',(0.,1.,0.));
#16205=DIRECTION('ref_axis',(1.,0.,0.));
#16206=DIRECTION('center_axis',(0.,1.,0.));
#16207=DIRECTION('ref_axis',(1.,0.,0.));
#16208=DIRECTION('center_axis',(0.,1.,0.));
#16209=DIRECTION('ref_axis',(1.,0.,0.));
#16210=DIRECTION('axis',(0.,0.,1.));
#16211=DIRECTION('refdir',(1.,0.,0.));
#16212=DIRECTION('center_axis',(0.,1.,0.));
#16213=DIRECTION('ref_axis',(1.,0.,0.));
#16214=DIRECTION('center_axis',(0.,1.,0.));
#16215=DIRECTION('ref_axis',(1.,0.,0.));
#16216=DIRECTION('',(0.,-1.,0.));
#16217=DIRECTION('center_axis',(0.,1.,0.));
#16218=DIRECTION('ref_axis',(1.,0.,0.));
#16219=DIRECTION('center_axis',(0.,1.,0.));
#16220=DIRECTION('ref_axis',(1.,0.,0.));
#16221=DIRECTION('center_axis',(0.,1.,0.));
#16222=DIRECTION('ref_axis',(1.,0.,0.));
#16223=DIRECTION('axis',(0.,0.,1.));
#16224=DIRECTION('refdir',(1.,0.,0.));
#16225=DIRECTION('center_axis',(0.,1.,0.));
#16226=DIRECTION('ref_axis',(1.,0.,0.));
#16227=DIRECTION('center_axis',(0.,1.,0.));
#16228=DIRECTION('ref_axis',(1.,0.,0.));
#16229=DIRECTION('',(0.,-1.,0.));
#16230=DIRECTION('center_axis',(0.,1.,0.));
#16231=DIRECTION('ref_axis',(1.,0.,0.));
#16232=DIRECTION('center_axis',(0.,1.,0.));
#16233=DIRECTION('ref_axis',(1.,0.,0.));
#16234=DIRECTION('center_axis',(0.,1.,0.));
#16235=DIRECTION('ref_axis',(1.,0.,0.));
#16236=DIRECTION('axis',(0.,0.,1.));
#16237=DIRECTION('refdir',(1.,0.,0.));
#16238=DIRECTION('center_axis',(0.,0.,1.));
#16239=DIRECTION('ref_axis',(1.,0.,0.));
#16240=DIRECTION('center_axis',(0.,0.,1.));
#16241=DIRECTION('ref_axis',(1.,0.,0.));
#16242=DIRECTION('',(0.,0.,1.));
#16243=DIRECTION('center_axis',(0.,0.,-1.));
#16244=DIRECTION('ref_axis',(1.,0.,0.));
#16245=DIRECTION('center_axis',(0.,0.,1.));
#16246=DIRECTION('ref_axis',(1.,0.,0.));
#16247=DIRECTION('center_axis',(0.,0.,1.));
#16248=DIRECTION('ref_axis',(1.,0.,0.));
#16249=DIRECTION('center_axis',(0.,0.,1.));
#16250=DIRECTION('ref_axis',(1.,0.,0.));
#16251=DIRECTION('center_axis',(0.,0.,1.));
#16252=DIRECTION('ref_axis',(1.,0.,0.));
#16253=DIRECTION('',(0.,0.,1.));
#16254=DIRECTION('center_axis',(0.,0.,-1.));
#16255=DIRECTION('ref_axis',(1.,0.,0.));
#16256=DIRECTION('center_axis',(0.,0.,1.));
#16257=DIRECTION('ref_axis',(1.,0.,0.));
#16258=DIRECTION('center_axis',(0.,0.,1.));
#16259=DIRECTION('ref_axis',(1.,0.,0.));
#16260=DIRECTION('center_axis',(0.,0.,1.));
#16261=DIRECTION('ref_axis',(1.,0.,0.));
#16262=DIRECTION('center_axis',(0.,0.,1.));
#16263=DIRECTION('ref_axis',(1.,0.,0.));
#16264=DIRECTION('',(0.,0.,1.));
#16265=DIRECTION('center_axis',(0.,0.,-1.));
#16266=DIRECTION('ref_axis',(1.,0.,0.));
#16267=DIRECTION('center_axis',(0.,0.,1.));
#16268=DIRECTION('ref_axis',(1.,0.,0.));
#16269=DIRECTION('center_axis',(0.,0.,1.));
#16270=DIRECTION('ref_axis',(1.,0.,0.));
#16271=DIRECTION('center_axis',(0.,0.,1.));
#16272=DIRECTION('ref_axis',(1.,0.,0.));
#16273=DIRECTION('center_axis',(0.,0.,1.));
#16274=DIRECTION('ref_axis',(1.,0.,0.));
#16275=DIRECTION('',(0.,0.,1.));
#16276=DIRECTION('center_axis',(0.,0.,-1.));
#16277=DIRECTION('ref_axis',(1.,0.,0.));
#16278=DIRECTION('center_axis',(0.,0.,1.));
#16279=DIRECTION('ref_axis',(1.,0.,0.));
#16280=DIRECTION('center_axis',(0.,0.,1.));
#16281=DIRECTION('ref_axis',(1.,0.,0.));
#16282=DIRECTION('center_axis',(0.,0.,1.));
#16283=DIRECTION('ref_axis',(1.,0.,0.));
#16284=DIRECTION('center_axis',(0.,0.,1.));
#16285=DIRECTION('ref_axis',(1.,0.,0.));
#16286=DIRECTION('',(0.,0.,1.));
#16287=DIRECTION('center_axis',(0.,0.,1.));
#16288=DIRECTION('ref_axis',(1.,0.,0.));
#16289=DIRECTION('center_axis',(0.,0.,1.));
#16290=DIRECTION('ref_axis',(1.,0.,0.));
#16291=DIRECTION('',(0.,0.,1.));
#16292=DIRECTION('center_axis',(0.,0.,1.));
#16293=DIRECTION('ref_axis',(1.,0.,0.));
#16294=DIRECTION('center_axis',(0.,0.,1.));
#16295=DIRECTION('ref_axis',(1.,0.,0.));
#16296=DIRECTION('',(0.,0.,1.));
#16297=DIRECTION('center_axis',(0.,0.,1.));
#16298=DIRECTION('ref_axis',(1.,0.,0.));
#16299=DIRECTION('center_axis',(0.,0.,1.));
#16300=DIRECTION('ref_axis',(1.,0.,0.));
#16301=DIRECTION('',(0.,0.,1.));
#16302=DIRECTION('center_axis',(0.,-0.56333682464151,0.826227342807548));
#16303=DIRECTION('ref_axis',(0.,-0.826227342807548,-0.56333682464151));
#16304=DIRECTION('',(0.,-0.826227342807548,-0.56333682464151));
#16305=DIRECTION('',(1.,0.,0.));
#16306=DIRECTION('',(0.,-0.826227342807548,-0.56333682464151));
#16307=DIRECTION('',(1.,0.,0.));
#16308=DIRECTION('center_axis',(0.,-1.,0.));
#16309=DIRECTION('ref_axis',(0.,0.,-1.));
#16310=DIRECTION('',(0.,0.,-1.));
#16311=DIRECTION('',(0.,0.,-1.));
#16312=DIRECTION('',(1.,0.,0.));
#16313=DIRECTION('center_axis',(0.,-0.56333682464151,-0.826227342807548));
#16314=DIRECTION('ref_axis',(0.,0.826227342807548,-0.56333682464151));
#16315=DIRECTION('',(0.,0.826227342807548,-0.56333682464151));
#16316=DIRECTION('',(0.,0.826227342807548,-0.56333682464151));
#16317=DIRECTION('',(1.,0.,0.));
#16318=DIRECTION('center_axis',(0.,-1.,0.));
#16319=DIRECTION('ref_axis',(0.,0.,-1.));
#16320=DIRECTION('',(0.,0.,-1.));
#16321=DIRECTION('',(0.,0.,-1.));
#16322=DIRECTION('',(1.,0.,0.));
#16323=DIRECTION('center_axis',(0.,0.,1.));
#16324=DIRECTION('ref_axis',(0.,-1.,0.));
#16325=DIRECTION('',(0.,-1.,0.));
#16326=DIRECTION('',(0.,-1.,0.));
#16327=DIRECTION('',(1.,0.,0.));
#16328=DIRECTION('center_axis',(0.,1.,0.));
#16329=DIRECTION('ref_axis',(0.,0.,1.));
#16330=DIRECTION('',(0.,0.,1.));
#16331=DIRECTION('',(0.,0.,1.));
#16332=DIRECTION('',(1.,0.,0.));
#16333=DIRECTION('center_axis',(0.,0.56333682464151,-0.826227342807548));
#16334=DIRECTION('ref_axis',(0.,0.826227342807548,0.56333682464151));
#16335=DIRECTION('',(0.,0.826227342807548,0.56333682464151));
#16336=DIRECTION('',(0.,0.826227342807548,0.56333682464151));
#16337=DIRECTION('',(1.,0.,0.));
#16338=DIRECTION('center_axis',(0.,1.,0.));
#16339=DIRECTION('ref_axis',(0.,0.,1.));
#16340=DIRECTION('',(0.,0.,1.));
#16341=DIRECTION('',(0.,0.,1.));
#16342=DIRECTION('',(1.,0.,0.));
#16343=DIRECTION('center_axis',(0.,0.56333682464151,0.826227342807548));
#16344=DIRECTION('ref_axis',(0.,-0.826227342807548,0.56333682464151));
#16345=DIRECTION('',(0.,-0.826227342807548,0.56333682464151));
#16346=DIRECTION('',(0.,-0.826227342807548,0.56333682464151));
#16347=DIRECTION('',(1.,0.,0.));
#16348=DIRECTION('center_axis',(0.,1.,0.));
#16349=DIRECTION('ref_axis',(0.,0.,1.));
#16350=DIRECTION('',(0.,0.,1.));
#16351=DIRECTION('',(0.,0.,1.));
#16352=DIRECTION('',(1.,0.,0.));
#16353=DIRECTION('center_axis',(0.,0.,-1.));
#16354=DIRECTION('ref_axis',(0.,1.,0.));
#16355=DIRECTION('',(0.,1.,0.));
#16356=DIRECTION('',(0.,1.,0.));
#16357=DIRECTION('',(1.,0.,0.));
#16358=DIRECTION('center_axis',(0.,-1.,0.));
#16359=DIRECTION('ref_axis',(0.,0.,-1.));
#16360=DIRECTION('',(0.,0.,-1.));
#16361=DIRECTION('',(0.,0.,-1.));
#16362=DIRECTION('center_axis',(1.,0.,0.));
#16363=DIRECTION('ref_axis',(0.,0.,-1.));
#16364=DIRECTION('center_axis',(1.,0.,0.));
#16365=DIRECTION('ref_axis',(0.,0.,-1.));
#16366=DIRECTION('axis',(0.,0.,1.));
#16367=DIRECTION('refdir',(1.,0.,0.));
#16368=DIRECTION('axis',(0.,0.,1.));
#16369=DIRECTION('refdir',(1.,0.,0.));
#16370=DIRECTION('center_axis',(0.,-1.,0.));
#16371=DIRECTION('ref_axis',(0.,0.,-1.));
#16372=DIRECTION('center_axis',(0.,-1.,0.));
#16373=DIRECTION('ref_axis',(1.,0.,0.));
#16374=DIRECTION('center_axis',(0.,-1.,0.));
#16375=DIRECTION('ref_axis',(1.,0.,0.));
#16376=DIRECTION('center_axis',(1.,0.,1.22464679914735E-16));
#16377=DIRECTION('ref_axis',(-1.22464679914735E-16,0.,1.));
#16378=DIRECTION('center_axis',(0.,1.,0.));
#16379=DIRECTION('ref_axis',(1.,0.,0.));
#16380=DIRECTION('center_axis',(0.,1.,0.));
#16381=DIRECTION('ref_axis',(1.,0.,0.));
#16382=DIRECTION('center_axis',(0.,-1.,0.));
#16383=DIRECTION('ref_axis',(1.,0.,0.));
#16384=DIRECTION('',(0.,1.,0.));
#16385=DIRECTION('center_axis',(0.,-1.,0.));
#16386=DIRECTION('ref_axis',(1.,0.,0.));
#16387=DIRECTION('center_axis',(0.,-1.,0.));
#16388=DIRECTION('ref_axis',(1.,0.,0.));
#16389=DIRECTION('center_axis',(0.,-1.,0.));
#16390=DIRECTION('ref_axis',(1.,0.,0.));
#16391=DIRECTION('',(0.,1.,0.));
#16392=DIRECTION('center_axis',(0.,-1.,0.));
#16393=DIRECTION('ref_axis',(1.,0.,0.));
#16394=DIRECTION('center_axis',(0.,1.,0.));
#16395=DIRECTION('ref_axis',(1.,0.,0.));
#16396=DIRECTION('',(-0.707106781186548,0.707106781186547,-8.65956056235493E-17));
#16397=DIRECTION('center_axis',(0.,-1.,0.));
#16398=DIRECTION('ref_axis',(1.,0.,0.));
#16399=DIRECTION('center_axis',(0.,1.,0.));
#16400=DIRECTION('ref_axis',(0.,0.,1.));
#16401=DIRECTION('center_axis',(0.,-1.,0.));
#16402=DIRECTION('ref_axis',(1.,0.,0.));
#16403=DIRECTION('center_axis',(0.,-1.,0.));
#16404=DIRECTION('ref_axis',(1.,0.,0.));
#16405=DIRECTION('',(0.,1.,0.));
#16406=DIRECTION('center_axis',(0.,-1.,0.));
#16407=DIRECTION('ref_axis',(0.,0.,-1.));
#16408=DIRECTION('center_axis',(0.,-1.,0.));
#16409=DIRECTION('ref_axis',(1.,0.,0.));
#16410=DIRECTION('center_axis',(0.,-1.,0.));
#16411=DIRECTION('ref_axis',(1.,0.,0.));
#16412=DIRECTION('',(0.707106781186548,0.707106781186547,8.65956056235493E-17));
#16413=DIRECTION('axis',(0.,0.,1.));
#16414=DIRECTION('refdir',(1.,0.,0.));
#16415=DIRECTION('center_axis',(0.,-1.,0.));
#16416=DIRECTION('ref_axis',(0.,0.,-1.));
#16417=DIRECTION('center_axis',(0.,-1.,0.));
#16418=DIRECTION('ref_axis',(1.,0.,0.));
#16419=DIRECTION('center_axis',(0.,-1.,0.));
#16420=DIRECTION('ref_axis',(1.,0.,0.));
#16421=DIRECTION('center_axis',(1.,0.,1.22464679914735E-16));
#16422=DIRECTION('ref_axis',(-1.22464679914735E-16,0.,1.));
#16423=DIRECTION('center_axis',(0.,1.,0.));
#16424=DIRECTION('ref_axis',(1.,0.,0.));
#16425=DIRECTION('center_axis',(0.,1.,0.));
#16426=DIRECTION('ref_axis',(1.,0.,0.));
#16427=DIRECTION('center_axis',(0.,-1.,0.));
#16428=DIRECTION('ref_axis',(1.,0.,0.));
#16429=DIRECTION('center_axis',(0.,-1.,0.));
#16430=DIRECTION('ref_axis',(1.,0.,0.));
#16431=DIRECTION('',(0.,1.,0.));
#16432=DIRECTION('center_axis',(0.,1.,0.));
#16433=DIRECTION('ref_axis',(0.,0.,1.));
#16434=DIRECTION('center_axis',(0.,-1.,0.));
#16435=DIRECTION('ref_axis',(1.,0.,0.));
#16436=DIRECTION('center_axis',(0.,-1.,0.));
#16437=DIRECTION('ref_axis',(1.,0.,0.));
#16438=DIRECTION('center_axis',(0.,-1.,0.));
#16439=DIRECTION('ref_axis',(1.,0.,0.));
#16440=DIRECTION('center_axis',(0.,-1.,0.));
#16441=DIRECTION('ref_axis',(1.,0.,0.));
#16442=DIRECTION('',(0.707106781186548,0.707106781186547,8.65956056235494E-17));
#16443=DIRECTION('center_axis',(0.,-1.,0.));
#16444=DIRECTION('ref_axis',(1.,0.,0.));
#16445=DIRECTION('center_axis',(0.,-1.,0.));
#16446=DIRECTION('ref_axis',(1.,0.,0.));
#16447=DIRECTION('',(0.,1.,0.));
#16448=DIRECTION('center_axis',(0.,1.,0.));
#16449=DIRECTION('ref_axis',(1.,0.,0.));
#16450=DIRECTION('center_axis',(0.,-1.,0.));
#16451=DIRECTION('ref_axis',(1.,0.,0.));
#16452=DIRECTION('',(-0.707106781186548,0.707106781186547,-8.65956056235494E-17));
#16453=DIRECTION('center_axis',(0.,-1.,0.));
#16454=DIRECTION('ref_axis',(0.,0.,-1.));
#16455=DIRECTION('center_axis',(0.,-1.,0.));
#16456=DIRECTION('ref_axis',(1.,0.,0.));
#16457=DIRECTION('',(0.,1.,0.));
#16458=DIRECTION('axis',(0.,0.,1.));
#16459=DIRECTION('refdir',(1.,0.,0.));
#16460=DIRECTION('center_axis',(0.,0.,1.));
#16461=DIRECTION('ref_axis',(1.,0.,0.));
#16462=DIRECTION('center_axis',(1.22464679914735E-16,-1.,0.));
#16463=DIRECTION('ref_axis',(-1.,-1.22464679914735E-16,0.));
#16464=DIRECTION('center_axis',(0.78183148246803,0.,0.623489801858733));
#16465=DIRECTION('ref_axis',(0.623489801858734,0.,-0.78183148246803));
#16466=DIRECTION('center_axis',(7.63554790147315E-17,-1.,-9.57467422477103E-17));
#16467=DIRECTION('ref_axis',(-0.623489801858734,-1.22464679914735E-16,0.78183148246803));
#16468=DIRECTION('center_axis',(0.974927912181824,0.,-0.222520933956314));
#16469=DIRECTION('ref_axis',(-0.222520933956314,0.,-0.974927912181824));
#16470=DIRECTION('center_axis',(-2.7250954951288E-17,-1.,-1.19394234705288E-16));
#16471=DIRECTION('ref_axis',(0.222520933956314,-1.22464679914735E-16,0.974927912181824));
#16472=DIRECTION('center_axis',(0.433883739117558,0.,-0.900968867902419));
#16473=DIRECTION('ref_axis',(-0.900968867902419,0.,-0.433883739117558));
#16474=DIRECTION('center_axis',(-1.10336864020811E-16,-1.,-5.31354332312403E-17));
#16475=DIRECTION('ref_axis',(0.900968867902419,-1.22464679914735E-16,0.433883739117558));
#16476=DIRECTION('center_axis',(-0.433883739117558,0.,-0.900968867902419));
#16477=DIRECTION('ref_axis',(-0.900968867902419,0.,0.433883739117558));
#16478=DIRECTION('center_axis',(-1.10336864020811E-16,-1.,5.31354332312403E-17));
#16479=DIRECTION('ref_axis',(0.900968867902419,-1.22464679914735E-16,-0.433883739117558));
#16480=DIRECTION('center_axis',(-0.974927912181824,0.,-0.222520933956314));
#16481=DIRECTION('ref_axis',(-0.222520933956315,0.,0.974927912181824));
#16482=DIRECTION('center_axis',(-2.7250954951288E-17,-1.,1.19394234705288E-16));
#16483=DIRECTION('ref_axis',(0.222520933956315,-1.22464679914735E-16,-0.974927912181824));
#16484=DIRECTION('center_axis',(-0.78183148246803,0.,0.623489801858734));
#16485=DIRECTION('ref_axis',(0.623489801858733,0.,0.78183148246803));
#16486=DIRECTION('center_axis',(7.63554790147315E-17,-1.,9.57467422477103E-17));
#16487=DIRECTION('ref_axis',(-0.623489801858733,-1.22464679914735E-16,-0.78183148246803));
#16488=DIRECTION('axis',(0.,0.,1.));
#16489=DIRECTION('refdir',(1.,0.,0.));
#16490=DIRECTION('center_axis',(0.,0.,1.));
#16491=DIRECTION('ref_axis',(1.,0.,0.));
#16492=DIRECTION('center_axis',(0.,-1.,0.));
#16493=DIRECTION('ref_axis',(0.,0.,-1.));
#16494=DIRECTION('center_axis',(0.,-1.,0.));
#16495=DIRECTION('ref_axis',(0.,0.,-1.));
#16496=DIRECTION('center_axis',(0.,1.,0.));
#16497=DIRECTION('ref_axis',(1.,0.,0.));
#16498=DIRECTION('center_axis',(0.,1.,0.));
#16499=DIRECTION('ref_axis',(1.,0.,0.));
#16500=DIRECTION('center_axis',(0.,1.,0.));
#16501=DIRECTION('ref_axis',(1.,0.,0.));
#16502=DIRECTION('center_axis',(0.,1.,0.));
#16503=DIRECTION('ref_axis',(1.,0.,0.));
#16504=DIRECTION('',(0.,-1.,0.));
#16505=DIRECTION('center_axis',(0.,-1.,0.));
#16506=DIRECTION('ref_axis',(1.,0.,0.));
#16507=DIRECTION('center_axis',(0.,1.,0.));
#16508=DIRECTION('ref_axis',(1.,0.,0.));
#16509=DIRECTION('center_axis',(0.,1.,0.));
#16510=DIRECTION('ref_axis',(1.,0.,0.));
#16511=DIRECTION('center_axis',(0.,1.,0.));
#16512=DIRECTION('ref_axis',(1.,0.,0.));
#16513=DIRECTION('center_axis',(0.,1.,0.));
#16514=DIRECTION('ref_axis',(1.,0.,0.));
#16515=DIRECTION('center_axis',(0.,1.,0.));
#16516=DIRECTION('ref_axis',(1.,0.,0.));
#16517=DIRECTION('center_axis',(0.,1.,0.));
#16518=DIRECTION('ref_axis',(1.,0.,0.));
#16519=DIRECTION('center_axis',(0.,-1.,0.));
#16520=DIRECTION('ref_axis',(1.,0.,0.));
#16521=DIRECTION('center_axis',(0.,-1.,0.));
#16522=DIRECTION('ref_axis',(0.,0.,-1.));
#16523=DIRECTION('center_axis',(8.96625347776458E-17,0.,1.));
#16524=DIRECTION('ref_axis',(1.,0.,0.));
#16525=DIRECTION('center_axis',(0.,-1.,0.));
#16526=DIRECTION('ref_axis',(0.,0.,-1.));
#16527=DIRECTION('center_axis',(0.,1.,0.));
#16528=DIRECTION('ref_axis',(1.,0.,0.));
#16529=DIRECTION('center_axis',(0.,-1.,0.));
#16530=DIRECTION('ref_axis',(1.,0.,0.));
#16531=DIRECTION('center_axis',(0.,-1.,0.));
#16532=DIRECTION('ref_axis',(0.,0.,-1.));
#16533=DIRECTION('center_axis',(0.,0.,1.));
#16534=DIRECTION('ref_axis',(1.,0.,0.));
#16535=DIRECTION('center_axis',(0.,-1.,0.));
#16536=DIRECTION('ref_axis',(0.,0.,-1.));
#16537=DIRECTION('center_axis',(0.,1.,0.));
#16538=DIRECTION('ref_axis',(1.,0.,0.));
#16539=DIRECTION('center_axis',(0.,-1.,0.));
#16540=DIRECTION('ref_axis',(1.,0.,0.));
#16541=DIRECTION('center_axis',(0.,-1.,0.));
#16542=DIRECTION('ref_axis',(1.,0.,0.));
#16543=DIRECTION('center_axis',(0.,-1.,0.));
#16544=DIRECTION('ref_axis',(0.,0.,-1.));
#16545=DIRECTION('center_axis',(0.,0.,1.));
#16546=DIRECTION('ref_axis',(1.,0.,0.));
#16547=DIRECTION('center_axis',(0.,-1.,0.));
#16548=DIRECTION('ref_axis',(0.,0.,-1.));
#16549=DIRECTION('center_axis',(0.,1.,0.));
#16550=DIRECTION('ref_axis',(1.,0.,0.));
#16551=DIRECTION('center_axis',(0.,-1.,0.));
#16552=DIRECTION('ref_axis',(1.,0.,0.));
#16553=DIRECTION('center_axis',(0.,-1.,0.));
#16554=DIRECTION('ref_axis',(0.,0.,-1.));
#16555=DIRECTION('center_axis',(8.96625347776458E-17,0.,1.));
#16556=DIRECTION('ref_axis',(1.,0.,0.));
#16557=DIRECTION('center_axis',(0.,-1.,0.));
#16558=DIRECTION('ref_axis',(0.,0.,-1.));
#16559=DIRECTION('center_axis',(0.,1.,0.));
#16560=DIRECTION('ref_axis',(1.,0.,0.));
#16561=DIRECTION('center_axis',(0.,-1.,0.));
#16562=DIRECTION('ref_axis',(1.,0.,0.));
#16563=DIRECTION('center_axis',(0.,-1.,0.));
#16564=DIRECTION('ref_axis',(0.,0.,-1.));
#16565=DIRECTION('center_axis',(0.,0.,1.));
#16566=DIRECTION('ref_axis',(1.,0.,0.));
#16567=DIRECTION('center_axis',(0.,-1.,0.));
#16568=DIRECTION('ref_axis',(0.,0.,-1.));
#16569=DIRECTION('center_axis',(0.,1.,0.));
#16570=DIRECTION('ref_axis',(1.,0.,0.));
#16571=DIRECTION('center_axis',(0.,1.,0.));
#16572=DIRECTION('ref_axis',(1.,0.,0.));
#16573=DIRECTION('',(0.,1.,0.));
#16574=DIRECTION('center_axis',(0.,-1.,0.));
#16575=DIRECTION('ref_axis',(1.,0.,0.));
#16576=DIRECTION('center_axis',(0.,-1.,0.));
#16577=DIRECTION('ref_axis',(1.,0.,0.));
#16578=DIRECTION('center_axis',(0.,1.,0.));
#16579=DIRECTION('ref_axis',(1.,0.,0.));
#16580=DIRECTION('center_axis',(0.,-1.,0.));
#16581=DIRECTION('ref_axis',(0.,0.,-1.));
#16582=DIRECTION('center_axis',(0.,0.,1.));
#16583=DIRECTION('ref_axis',(1.,0.,0.));
#16584=DIRECTION('center_axis',(0.,-1.,0.));
#16585=DIRECTION('ref_axis',(0.,0.,-1.));
#16586=DIRECTION('center_axis',(0.,-1.,0.));
#16587=DIRECTION('ref_axis',(-1.,0.,0.));
#16588=DIRECTION('center_axis',(0.,1.,0.));
#16589=DIRECTION('ref_axis',(1.,0.,0.));
#16590=DIRECTION('axis',(0.,0.,1.));
#16591=DIRECTION('refdir',(1.,0.,0.));
#16592=DIRECTION('center_axis',(0.,1.,0.));
#16593=DIRECTION('ref_axis',(0.,0.,1.));
#16594=DIRECTION('center_axis',(0.,-1.,0.));
#16595=DIRECTION('ref_axis',(1.,0.,0.));
#16596=DIRECTION('center_axis',(0.,-1.,0.));
#16597=DIRECTION('ref_axis',(1.,0.,0.));
#16598=DIRECTION('center_axis',(0.,-1.,0.));
#16599=DIRECTION('ref_axis',(1.,0.,0.));
#16600=DIRECTION('center_axis',(0.,-1.,0.));
#16601=DIRECTION('ref_axis',(1.,0.,0.));
#16602=DIRECTION('',(0.,1.,0.));
#16603=DIRECTION('center_axis',(0.,-1.,0.));
#16604=DIRECTION('ref_axis',(0.,0.,-1.));
#16605=DIRECTION('center_axis',(0.,-1.,0.));
#16606=DIRECTION('ref_axis',(1.,0.,0.));
#16607=DIRECTION('center_axis',(0.,-1.,0.));
#16608=DIRECTION('ref_axis',(1.,0.,0.));
#16609=DIRECTION('',(0.,1.,0.));
#16610=DIRECTION('center_axis',(0.,1.,0.));
#16611=DIRECTION('ref_axis',(0.,0.,1.));
#16612=DIRECTION('center_axis',(0.,-1.,0.));
#16613=DIRECTION('ref_axis',(1.,0.,0.));
#16614=DIRECTION('center_axis',(0.,-1.,0.));
#16615=DIRECTION('ref_axis',(1.,0.,0.));
#16616=DIRECTION('center_axis',(0.,-1.,0.));
#16617=DIRECTION('ref_axis',(1.,0.,0.));
#16618=DIRECTION('center_axis',(0.,-1.,0.));
#16619=DIRECTION('ref_axis',(1.,0.,0.));
#16620=DIRECTION('',(0.,1.,0.));
#16621=DIRECTION('center_axis',(0.,-1.,0.));
#16622=DIRECTION('ref_axis',(0.,0.,-1.));
#16623=DIRECTION('center_axis',(0.,-1.,0.));
#16624=DIRECTION('ref_axis',(1.,0.,0.));
#16625=DIRECTION('center_axis',(0.,-1.,0.));
#16626=DIRECTION('ref_axis',(1.,0.,0.));
#16627=DIRECTION('',(0.,1.,0.));
#16628=DIRECTION('',(0.,0.,1.));
#16629=DIRECTION('',(1.,0.,0.));
#16630=DIRECTION('',(0.,0.,1.));
#16631=DIRECTION('',(1.,0.,0.));
#16632=DIRECTION('',(0.,0.,1.));
#16633=DIRECTION('',(1.,0.,0.));
#16634=DIRECTION('',(0.,0.,1.));
#16635=DIRECTION('',(1.,0.,0.));
#16636=DIRECTION('',(0.,0.,1.));
#16637=DIRECTION('',(1.,0.,0.));
#16638=DIRECTION('axis',(0.,0.,1.));
#16639=DIRECTION('refdir',(1.,0.,0.));
#16640=DIRECTION('center_axis',(0.,1.,0.));
#16641=DIRECTION('ref_axis',(0.,0.,1.));
#16642=DIRECTION('center_axis',(0.,-1.,0.));
#16643=DIRECTION('ref_axis',(1.,0.,0.));
#16644=DIRECTION('center_axis',(0.,-1.,0.));
#16645=DIRECTION('ref_axis',(1.,0.,0.));
#16646=DIRECTION('center_axis',(0.,-1.,0.));
#16647=DIRECTION('ref_axis',(1.,0.,0.));
#16648=DIRECTION('',(0.707106781186547,0.707106781186548,8.65956056235493E-17));
#16649=DIRECTION('center_axis',(0.,-1.,0.));
#16650=DIRECTION('ref_axis',(1.,0.,0.));
#16651=DIRECTION('center_axis',(0.,-1.,0.));
#16652=DIRECTION('ref_axis',(1.,0.,0.));
#16653=DIRECTION('',(0.,1.,0.));
#16654=DIRECTION('center_axis',(0.,1.,0.));
#16655=DIRECTION('ref_axis',(1.,0.,0.));
#16656=DIRECTION('center_axis',(0.,-1.,0.));
#16657=DIRECTION('ref_axis',(1.,0.,0.));
#16658=DIRECTION('',(-0.707106781186547,0.707106781186548,-8.65956056235493E-17));
#16659=DIRECTION('center_axis',(0.,-1.,0.));
#16660=DIRECTION('ref_axis',(0.,0.,-1.));
#16661=DIRECTION('center_axis',(0.,-1.,0.));
#16662=DIRECTION('ref_axis',(1.,0.,0.));
#16663=DIRECTION('center_axis',(0.,1.,0.));
#16664=DIRECTION('ref_axis',(1.,0.,0.));
#16665=DIRECTION('center_axis',(0.,1.,0.));
#16666=DIRECTION('ref_axis',(1.,0.,0.));
#16667=DIRECTION('',(-0.447213595499958,0.894427190999916,-5.47678698264203E-17));
#16668=DIRECTION('center_axis',(0.,-1.,0.));
#16669=DIRECTION('ref_axis',(1.,0.,0.));
#16670=DIRECTION('center_axis',(0.,1.,0.));
#16671=DIRECTION('ref_axis',(1.,0.,0.));
#16672=DIRECTION('',(0.,1.,0.));
#16673=DIRECTION('center_axis',(0.,1.,0.));
#16674=DIRECTION('ref_axis',(1.,0.,0.));
#16675=DIRECTION('center_axis',(0.,-1.,0.));
#16676=DIRECTION('ref_axis',(1.,0.,0.));
#16677=DIRECTION('',(-0.707106781186547,0.707106781186548,-8.65956056235493E-17));
#16678=DIRECTION('center_axis',(0.,-1.,0.));
#16679=DIRECTION('ref_axis',(0.,0.,-1.));
#16680=DIRECTION('center_axis',(0.866025403784439,0.,-0.5));
#16681=DIRECTION('ref_axis',(0.5,0.,0.866025403784439));
#16682=DIRECTION('',(-0.5,0.,-0.866025403784439));
#16683=DIRECTION('',(0.,-1.,0.));
#16684=DIRECTION('',(0.5,0.,0.866025403784439));
#16685=DIRECTION('',(0.,-1.,0.));
#16686=DIRECTION('center_axis',(1.60246890531964E-16,0.,-1.));
#16687=DIRECTION('ref_axis',(1.,0.,1.60246890531964E-16));
#16688=DIRECTION('',(-1.,0.,-1.60246890531964E-16));
#16689=DIRECTION('',(0.,-1.,0.));
#16690=DIRECTION('',(1.,0.,1.60246890531964E-16));
#16691=DIRECTION('center_axis',(-0.866025403784439,0.,-0.5));
#16692=DIRECTION('ref_axis',(0.5,0.,-0.866025403784439));
#16693=DIRECTION('',(-0.5,0.,0.866025403784439));
#16694=DIRECTION('',(0.,-1.,0.));
#16695=DIRECTION('',(0.5,0.,-0.866025403784439));
#16696=DIRECTION('center_axis',(-0.866025403784439,0.,0.5));
#16697=DIRECTION('ref_axis',(-0.5,0.,-0.866025403784439));
#16698=DIRECTION('',(0.5,0.,0.866025403784439));
#16699=DIRECTION('',(0.,-1.,0.));
#16700=DIRECTION('',(-0.5,0.,-0.866025403784439));
#16701=DIRECTION('center_axis',(-1.60246890531964E-16,0.,1.));
#16702=DIRECTION('ref_axis',(-1.,0.,-1.60246890531964E-16));
#16703=DIRECTION('',(1.,0.,1.60246890531964E-16));
#16704=DIRECTION('',(0.,-1.,0.));
#16705=DIRECTION('',(-1.,0.,-1.60246890531964E-16));
#16706=DIRECTION('center_axis',(0.866025403784439,0.,0.5));
#16707=DIRECTION('ref_axis',(-0.5,0.,0.866025403784439));
#16708=DIRECTION('',(0.5,0.,-0.866025403784439));
#16709=DIRECTION('',(-0.5,0.,0.866025403784439));
#16710=DIRECTION('center_axis',(0.,1.,0.));
#16711=DIRECTION('ref_axis',(1.,0.,0.));
#16712=DIRECTION('center_axis',(0.,-1.,0.));
#16713=DIRECTION('ref_axis',(0.,0.,-1.));
#16714=DIRECTION('axis',(0.,0.,1.));
#16715=DIRECTION('refdir',(1.,0.,0.));
#16716=DIRECTION('axis',(0.,0.,1.));
#16717=DIRECTION('refdir',(1.,0.,0.));
#16718=DIRECTION('center_axis',(0.,0.,1.));
#16719=DIRECTION('ref_axis',(1.,0.,0.));
#16720=DIRECTION('center_axis',(0.,0.,1.));
#16721=DIRECTION('ref_axis',(1.,0.,0.));
#16722=DIRECTION('',(0.,0.,1.));
#16723=DIRECTION('center_axis',(0.,0.,-1.));
#16724=DIRECTION('ref_axis',(1.,0.,0.));
#16725=DIRECTION('center_axis',(0.,0.,1.));
#16726=DIRECTION('ref_axis',(1.,0.,0.));
#16727=DIRECTION('center_axis',(0.,0.,1.));
#16728=DIRECTION('ref_axis',(1.,0.,0.));
#16729=DIRECTION('',(0.,0.,1.));
#16730=DIRECTION('center_axis',(0.,0.,-1.));
#16731=DIRECTION('ref_axis',(1.,0.,0.));
#16732=DIRECTION('center_axis',(0.,0.,1.));
#16733=DIRECTION('ref_axis',(1.,0.,0.));
#16734=DIRECTION('center_axis',(0.,0.,1.));
#16735=DIRECTION('ref_axis',(1.,0.,0.));
#16736=DIRECTION('',(0.,0.,1.));
#16737=DIRECTION('center_axis',(0.,0.,-1.));
#16738=DIRECTION('ref_axis',(1.,0.,0.));
#16739=DIRECTION('center_axis',(0.,0.,1.));
#16740=DIRECTION('ref_axis',(1.,0.,0.));
#16741=DIRECTION('center_axis',(0.,0.,1.));
#16742=DIRECTION('ref_axis',(1.,0.,0.));
#16743=DIRECTION('',(0.,0.,1.));
#16744=DIRECTION('center_axis',(0.,0.,-1.));
#16745=DIRECTION('ref_axis',(1.,0.,0.));
#16746=DIRECTION('center_axis',(0.,1.,0.));
#16747=DIRECTION('ref_axis',(1.,0.,0.));
#16748=DIRECTION('center_axis',(0.,1.,0.));
#16749=DIRECTION('ref_axis',(1.,0.,0.));
#16750=DIRECTION('',(0.,1.,0.));
#16751=DIRECTION('center_axis',(0.,-1.,0.));
#16752=DIRECTION('ref_axis',(1.,0.,0.));
#16753=DIRECTION('center_axis',(0.,1.,0.));
#16754=DIRECTION('ref_axis',(-1.,0.,0.));
#16755=DIRECTION('',(-1.,0.,0.));
#16756=DIRECTION('',(0.,0.,1.));
#16757=DIRECTION('',(-1.,0.,0.));
#16758=DIRECTION('',(0.,0.,1.));
#16759=DIRECTION('center_axis',(1.,0.,0.));
#16760=DIRECTION('ref_axis',(0.,1.,0.));
#16761=DIRECTION('',(0.,1.,0.));
#16762=DIRECTION('',(0.,1.,0.));
#16763=DIRECTION('',(0.,0.,1.));
#16764=DIRECTION('center_axis',(0.,-1.,0.));
#16765=DIRECTION('ref_axis',(1.,0.,0.));
#16766=DIRECTION('',(1.,0.,0.));
#16767=DIRECTION('',(1.,0.,0.));
#16768=DIRECTION('',(0.,0.,1.));
#16769=DIRECTION('center_axis',(-1.,0.,0.));
#16770=DIRECTION('ref_axis',(0.,-1.,0.));
#16771=DIRECTION('',(0.,-1.,0.));
#16772=DIRECTION('',(0.,-1.,0.));
#16773=DIRECTION('center_axis',(0.,0.,1.));
#16774=DIRECTION('ref_axis',(1.,0.,0.));
#16775=DIRECTION('center_axis',(0.,0.,1.));
#16776=DIRECTION('ref_axis',(1.,0.,0.));
#16777=DIRECTION('center_axis',(0.,0.,1.));
#16778=DIRECTION('ref_axis',(1.,0.,0.));
#16779=DIRECTION('',(0.,0.,1.));
#16780=DIRECTION('center_axis',(0.,0.,-1.));
#16781=DIRECTION('ref_axis',(1.,0.,0.));
#16782=DIRECTION('center_axis',(0.,0.,1.));
#16783=DIRECTION('ref_axis',(1.,0.,0.));
#16784=DIRECTION('center_axis',(0.,0.,1.));
#16785=DIRECTION('ref_axis',(1.,0.,0.));
#16786=DIRECTION('',(0.,0.,1.));
#16787=DIRECTION('center_axis',(0.,0.,-1.));
#16788=DIRECTION('ref_axis',(1.,0.,0.));
#16789=DIRECTION('center_axis',(0.,0.,1.));
#16790=DIRECTION('ref_axis',(1.,0.,0.));
#16791=DIRECTION('center_axis',(0.,0.,1.));
#16792=DIRECTION('ref_axis',(1.,0.,0.));
#16793=DIRECTION('',(0.,0.,1.));
#16794=DIRECTION('center_axis',(0.,0.,-1.));
#16795=DIRECTION('ref_axis',(1.,0.,0.));
#16796=DIRECTION('center_axis',(0.,0.,1.));
#16797=DIRECTION('ref_axis',(1.,0.,0.));
#16798=DIRECTION('center_axis',(0.,0.,1.));
#16799=DIRECTION('ref_axis',(1.,0.,0.));
#16800=DIRECTION('',(0.,0.,1.));
#16801=DIRECTION('center_axis',(0.,0.,-1.));
#16802=DIRECTION('ref_axis',(1.,0.,0.));
#16803=DIRECTION('center_axis',(0.,0.,1.));
#16804=DIRECTION('ref_axis',(1.,0.,0.));
#16805=DIRECTION('',(0.,0.,-1.));
#16806=DIRECTION('center_axis',(0.,0.,-1.));
#16807=DIRECTION('ref_axis',(1.,0.,0.));
#16808=DIRECTION('',(0.,0.,1.));
#16809=DIRECTION('center_axis',(0.,0.,1.));
#16810=DIRECTION('ref_axis',(1.,0.,0.));
#16811=DIRECTION('center_axis',(0.,0.,1.));
#16812=DIRECTION('ref_axis',(1.,0.,0.));
#16813=DIRECTION('',(0.,-1.,0.));
#16814=DIRECTION('',(1.,0.,0.));
#16815=DIRECTION('',(0.,1.,0.));
#16816=DIRECTION('',(-1.,0.,0.));
#16817=DIRECTION('',(0.,-1.,0.));
#16818=DIRECTION('center_axis',(-1.,0.,0.));
#16819=DIRECTION('ref_axis',(0.,-1.,0.));
#16820=DIRECTION('',(0.,-1.,0.));
#16821=DIRECTION('',(0.,0.,1.));
#16822=DIRECTION('center_axis',(-1.,0.,0.));
#16823=DIRECTION('ref_axis',(0.,-1.,0.));
#16824=DIRECTION('',(0.,0.,1.));
#16825=DIRECTION('',(0.,-1.,0.));
#16826=DIRECTION('center_axis',(0.,1.,0.));
#16827=DIRECTION('ref_axis',(-1.,0.,0.));
#16828=DIRECTION('',(-1.,0.,0.));
#16829=DIRECTION('',(0.,0.,1.));
#16830=DIRECTION('center_axis',(1.,0.,0.));
#16831=DIRECTION('ref_axis',(0.,1.,0.));
#16832=DIRECTION('',(0.,1.,0.));
#16833=DIRECTION('',(0.,0.,1.));
#16834=DIRECTION('center_axis',(0.,-1.,0.));
#16835=DIRECTION('ref_axis',(1.,0.,0.));
#16836=DIRECTION('',(1.,0.,0.));
#16837=DIRECTION('center_axis',(0.,0.,1.));
#16838=DIRECTION('ref_axis',(1.,0.,0.));
#16839=DIRECTION('axis',(0.,0.,1.));
#16840=DIRECTION('refdir',(1.,0.,0.));
#16841=DIRECTION('center_axis',(0.,1.,0.));
#16842=DIRECTION('ref_axis',(-1.,0.,0.));
#16843=DIRECTION('',(-1.,0.,0.));
#16844=DIRECTION('',(0.,0.,1.));
#16845=DIRECTION('',(-1.,0.,0.));
#16846=DIRECTION('',(0.,0.,1.));
#16847=DIRECTION('center_axis',(1.,0.,0.));
#16848=DIRECTION('ref_axis',(0.,1.,0.));
#16849=DIRECTION('',(0.,1.,0.));
#16850=DIRECTION('',(0.,1.,0.));
#16851=DIRECTION('',(0.,0.,1.));
#16852=DIRECTION('center_axis',(0.,-1.,0.));
#16853=DIRECTION('ref_axis',(1.,0.,0.));
#16854=DIRECTION('',(1.,0.,0.));
#16855=DIRECTION('',(1.,0.,0.));
#16856=DIRECTION('',(0.,0.,1.));
#16857=DIRECTION('center_axis',(-1.,0.,0.));
#16858=DIRECTION('ref_axis',(0.,-1.,0.));
#16859=DIRECTION('',(0.,-1.,0.));
#16860=DIRECTION('',(0.,-1.,0.));
#16861=DIRECTION('center_axis',(0.,0.,1.));
#16862=DIRECTION('ref_axis',(1.,0.,0.));
#16863=DIRECTION('center_axis',(0.,0.,1.));
#16864=DIRECTION('ref_axis',(1.,0.,0.));
#16865=DIRECTION('axis',(0.,0.,1.));
#16866=DIRECTION('refdir',(1.,0.,0.));
#16867=DIRECTION('center_axis',(1.,0.,0.));
#16868=DIRECTION('ref_axis',(0.,0.,-1.));
#16869=DIRECTION('',(1.,0.,0.));
#16870=DIRECTION('center_axis',(0.,0.,1.));
#16871=DIRECTION('ref_axis',(1.,0.,0.));
#16872=DIRECTION('center_axis',(0.,0.,1.));
#16873=DIRECTION('ref_axis',(1.,0.,0.));
#16874=DIRECTION('',(0.,0.,1.));
#16875=DIRECTION('center_axis',(0.,0.,-1.));
#16876=DIRECTION('ref_axis',(1.,0.,0.));
#16877=DIRECTION('center_axis',(0.,0.,1.));
#16878=DIRECTION('ref_axis',(1.,0.,0.));
#16879=DIRECTION('center_axis',(0.,0.,1.));
#16880=DIRECTION('ref_axis',(1.,0.,0.));
#16881=DIRECTION('center_axis',(0.,0.,1.));
#16882=DIRECTION('ref_axis',(1.,0.,0.));
#16883=DIRECTION('',(0.,0.,1.));
#16884=DIRECTION('center_axis',(0.,0.,-1.));
#16885=DIRECTION('ref_axis',(1.,0.,0.));
#16886=DIRECTION('center_axis',(0.,0.,1.));
#16887=DIRECTION('ref_axis',(1.,0.,0.));
#16888=DIRECTION('center_axis',(0.,0.,1.));
#16889=DIRECTION('ref_axis',(1.,0.,0.));
#16890=DIRECTION('center_axis',(0.,0.,1.));
#16891=DIRECTION('ref_axis',(1.,0.,0.));
#16892=DIRECTION('',(0.,0.,1.));
#16893=DIRECTION('center_axis',(0.,0.,-1.));
#16894=DIRECTION('ref_axis',(1.,0.,0.));
#16895=DIRECTION('center_axis',(0.,0.,1.));
#16896=DIRECTION('ref_axis',(1.,0.,0.));
#16897=DIRECTION('center_axis',(0.,0.,1.));
#16898=DIRECTION('ref_axis',(1.,0.,0.));
#16899=DIRECTION('center_axis',(0.,0.,1.));
#16900=DIRECTION('ref_axis',(1.,0.,0.));
#16901=DIRECTION('',(0.,0.,1.));
#16902=DIRECTION('center_axis',(0.,0.,-1.));
#16903=DIRECTION('ref_axis',(1.,0.,0.));
#16904=DIRECTION('center_axis',(0.,0.,1.));
#16905=DIRECTION('ref_axis',(1.,0.,0.));
#16906=DIRECTION('center_axis',(0.,0.,1.));
#16907=DIRECTION('ref_axis',(1.,0.,0.));
#16908=DIRECTION('',(0.,0.,-1.));
#16909=DIRECTION('center_axis',(0.,0.,1.));
#16910=DIRECTION('ref_axis',(1.,0.,0.));
#16911=DIRECTION('',(0.,0.,1.));
#16912=DIRECTION('center_axis',(0.,0.,1.));
#16913=DIRECTION('ref_axis',(1.,0.,0.));
#16914=DIRECTION('center_axis',(0.,0.,1.));
#16915=DIRECTION('ref_axis',(1.,0.,0.));
#16916=DIRECTION('center_axis',(0.,0.,1.));
#16917=DIRECTION('ref_axis',(1.,0.,0.));
#16918=DIRECTION('center_axis',(0.,0.,1.));
#16919=DIRECTION('ref_axis',(1.,0.,0.));
#16920=DIRECTION('',(0.,0.,-1.));
#16921=DIRECTION('center_axis',(0.,0.,1.));
#16922=DIRECTION('ref_axis',(1.,0.,0.));
#16923=DIRECTION('',(0.,0.,1.));
#16924=DIRECTION('center_axis',(0.,0.,1.));
#16925=DIRECTION('ref_axis',(1.,0.,0.));
#16926=DIRECTION('center_axis',(0.,0.,1.));
#16927=DIRECTION('ref_axis',(1.,0.,0.));
#16928=DIRECTION('center_axis',(0.,0.,1.));
#16929=DIRECTION('ref_axis',(1.,0.,0.));
#16930=DIRECTION('center_axis',(0.,0.,1.));
#16931=DIRECTION('ref_axis',(-0.707106781186548,-0.707106781186547,0.));
#16932=DIRECTION('',(0.,0.,-1.));
#16933=DIRECTION('center_axis',(0.,0.,1.));
#16934=DIRECTION('ref_axis',(1.,0.,0.));
#16935=DIRECTION('',(0.,0.,1.));
#16936=DIRECTION('center_axis',(0.,0.,1.));
#16937=DIRECTION('ref_axis',(1.,0.,0.));
#16938=DIRECTION('center_axis',(0.,0.,1.));
#16939=DIRECTION('ref_axis',(1.,0.,0.));
#16940=DIRECTION('center_axis',(0.,0.,1.));
#16941=DIRECTION('ref_axis',(1.,0.,0.));
#16942=DIRECTION('center_axis',(0.,0.,1.));
#16943=DIRECTION('ref_axis',(-0.707106781186547,0.707106781186548,0.));
#16944=DIRECTION('',(0.,0.,-1.));
#16945=DIRECTION('center_axis',(0.,0.,1.));
#16946=DIRECTION('ref_axis',(1.,0.,0.));
#16947=DIRECTION('',(0.,0.,1.));
#16948=DIRECTION('center_axis',(0.,0.,1.));
#16949=DIRECTION('ref_axis',(1.,0.,0.));
#16950=DIRECTION('center_axis',(0.,0.,1.));
#16951=DIRECTION('ref_axis',(1.,0.,0.));
#16952=DIRECTION('center_axis',(0.,0.,1.));
#16953=DIRECTION('ref_axis',(1.,0.,0.));
#16954=DIRECTION('center_axis',(0.,0.,1.));
#16955=DIRECTION('ref_axis',(1.,0.,0.));
#16956=DIRECTION('center_axis',(0.,0.,1.));
#16957=DIRECTION('ref_axis',(1.,0.,0.));
#16958=DIRECTION('',(0.,0.,1.));
#16959=DIRECTION('center_axis',(0.,0.,-1.));
#16960=DIRECTION('ref_axis',(1.,0.,0.));
#16961=DIRECTION('center_axis',(0.,0.,1.));
#16962=DIRECTION('ref_axis',(1.,0.,0.));
#16963=DIRECTION('center_axis',(0.,0.,1.));
#16964=DIRECTION('ref_axis',(1.,0.,0.));
#16965=DIRECTION('center_axis',(0.,0.,1.));
#16966=DIRECTION('ref_axis',(1.,0.,0.));
#16967=DIRECTION('center_axis',(0.,0.,1.));
#16968=DIRECTION('ref_axis',(1.,0.,0.));
#16969=DIRECTION('center_axis',(0.,0.,1.));
#16970=DIRECTION('ref_axis',(1.,0.,0.));
#16971=DIRECTION('center_axis',(0.,0.,1.));
#16972=DIRECTION('ref_axis',(1.,0.,0.));
#16973=DIRECTION('center_axis',(0.,0.,1.));
#16974=DIRECTION('ref_axis',(1.,0.,0.));
#16975=DIRECTION('center_axis',(0.,0.,-1.));
#16976=DIRECTION('ref_axis',(1.,0.,0.));
#16977=DIRECTION('center_axis',(0.,0.,-1.));
#16978=DIRECTION('ref_axis',(1.,0.,0.));
#16979=DIRECTION('center_axis',(0.,0.,-1.));
#16980=DIRECTION('ref_axis',(1.,0.,0.));
#16981=DIRECTION('center_axis',(0.,0.,1.));
#16982=DIRECTION('ref_axis',(1.,0.,0.));
#16983=DIRECTION('center_axis',(0.,0.,1.));
#16984=DIRECTION('ref_axis',(1.,0.,0.));
#16985=DIRECTION('',(0.,0.,1.));
#16986=DIRECTION('center_axis',(0.,0.,1.));
#16987=DIRECTION('ref_axis',(1.,0.,0.));
#16988=DIRECTION('center_axis',(0.,0.,1.));
#16989=DIRECTION('ref_axis',(1.,0.,0.));
#16990=DIRECTION('',(0.,0.,1.));
#16991=DIRECTION('center_axis',(0.,0.,1.));
#16992=DIRECTION('ref_axis',(1.,0.,0.));
#16993=DIRECTION('center_axis',(0.,0.,1.));
#16994=DIRECTION('ref_axis',(1.,0.,0.));
#16995=DIRECTION('',(0.,0.,1.));
#16996=DIRECTION('center_axis',(0.,0.,1.));
#16997=DIRECTION('ref_axis',(1.,0.,0.));
#16998=DIRECTION('center_axis',(0.,0.,1.));
#16999=DIRECTION('ref_axis',(1.,0.,0.));
#17000=DIRECTION('',(0.,0.,-1.));
#17001=DIRECTION('center_axis',(0.,0.,1.));
#17002=DIRECTION('ref_axis',(1.,0.,0.));
#17003=DIRECTION('center_axis',(0.,0.,1.));
#17004=DIRECTION('ref_axis',(1.,0.,0.));
#17005=DIRECTION('',(0.,0.,1.));
#17006=DIRECTION('center_axis',(0.,0.,-1.));
#17007=DIRECTION('ref_axis',(1.,0.,0.));
#17008=DIRECTION('center_axis',(0.,0.,1.));
#17009=DIRECTION('ref_axis',(1.,0.,0.));
#17010=DIRECTION('center_axis',(0.,0.,1.));
#17011=DIRECTION('ref_axis',(1.,0.,0.));
#17012=DIRECTION('center_axis',(0.,0.,1.));
#17013=DIRECTION('ref_axis',(1.,0.,0.));
#17014=DIRECTION('',(0.,0.,-1.));
#17015=DIRECTION('center_axis',(0.,0.,1.));
#17016=DIRECTION('ref_axis',(1.,0.,0.));
#17017=DIRECTION('center_axis',(0.,0.,1.));
#17018=DIRECTION('ref_axis',(1.,0.,0.));
#17019=DIRECTION('',(0.,0.,-1.));
#17020=DIRECTION('center_axis',(0.,0.,-1.));
#17021=DIRECTION('ref_axis',(1.,0.,0.));
#17022=DIRECTION('center_axis',(0.,0.,1.));
#17023=DIRECTION('ref_axis',(1.,0.,0.));
#17024=DIRECTION('center_axis',(0.,0.,1.));
#17025=DIRECTION('ref_axis',(1.,0.,0.));
#17026=DIRECTION('axis',(0.,0.,1.));
#17027=DIRECTION('refdir',(1.,0.,0.));
#17028=DIRECTION('center_axis',(0.,0.,1.));
#17029=DIRECTION('ref_axis',(1.,0.,0.));
#17030=DIRECTION('center_axis',(0.,0.,-1.));
#17031=DIRECTION('ref_axis',(1.,0.,0.));
#17032=DIRECTION('',(0.,0.,-1.));
#17033=DIRECTION('center_axis',(0.,0.,-1.));
#17034=DIRECTION('ref_axis',(1.,0.,0.));
#17035=DIRECTION('center_axis',(0.,0.,1.));
#17036=DIRECTION('ref_axis',(1.,0.,0.));
#17037=DIRECTION('center_axis',(0.,0.,1.));
#17038=DIRECTION('ref_axis',(1.,0.,0.));
#17039=DIRECTION('',(0.,0.,-1.));
#17040=DIRECTION('center_axis',(0.,0.,1.));
#17041=DIRECTION('ref_axis',(1.,0.,0.));
#17042=DIRECTION('center_axis',(0.,0.,1.));
#17043=DIRECTION('ref_axis',(1.,0.,0.));
#17044=DIRECTION('center_axis',(0.,0.,1.));
#17045=DIRECTION('ref_axis',(1.,0.,0.));
#17046=DIRECTION('axis',(0.,0.,1.));
#17047=DIRECTION('refdir',(1.,0.,0.));
#17048=DIRECTION('center_axis',(0.,0.,1.));
#17049=DIRECTION('ref_axis',(1.,0.,0.));
#17050=DIRECTION('center_axis',(0.,0.,1.));
#17051=DIRECTION('ref_axis',(1.,0.,0.));
#17052=DIRECTION('',(0.,0.,1.));
#17053=DIRECTION('center_axis',(0.,0.,-1.));
#17054=DIRECTION('ref_axis',(1.,0.,0.));
#17055=DIRECTION('center_axis',(0.,0.,1.));
#17056=DIRECTION('ref_axis',(1.,0.,0.));
#17057=DIRECTION('center_axis',(0.,0.,1.));
#17058=DIRECTION('ref_axis',(1.,0.,0.));
#17059=DIRECTION('',(0.,0.,1.));
#17060=DIRECTION('center_axis',(0.,0.,-1.));
#17061=DIRECTION('ref_axis',(1.,0.,0.));
#17062=DIRECTION('center_axis',(0.,0.,1.));
#17063=DIRECTION('ref_axis',(1.,0.,0.));
#17064=DIRECTION('center_axis',(0.,0.,1.));
#17065=DIRECTION('ref_axis',(1.,0.,0.));
#17066=DIRECTION('',(0.,0.,1.));
#17067=DIRECTION('center_axis',(0.,0.,-1.));
#17068=DIRECTION('ref_axis',(1.,0.,0.));
#17069=DIRECTION('center_axis',(0.,0.,1.));
#17070=DIRECTION('ref_axis',(1.,0.,0.));
#17071=DIRECTION('center_axis',(0.,0.,1.));
#17072=DIRECTION('ref_axis',(1.,0.,0.));
#17073=DIRECTION('',(0.,0.,1.));
#17074=DIRECTION('center_axis',(0.,0.,-1.));
#17075=DIRECTION('ref_axis',(1.,0.,0.));
#17076=DIRECTION('center_axis',(0.,0.,1.));
#17077=DIRECTION('ref_axis',(1.,0.,0.));
#17078=DIRECTION('center_axis',(0.,0.,-1.));
#17079=DIRECTION('ref_axis',(1.,0.,0.));
#17080=DIRECTION('',(0.,0.,-1.));
#17081=DIRECTION('center_axis',(0.,0.,-1.));
#17082=DIRECTION('ref_axis',(1.,0.,0.));
#17083=DIRECTION('center_axis',(0.,0.,1.));
#17084=DIRECTION('ref_axis',(1.,0.,0.));
#17085=DIRECTION('center_axis',(0.,0.,1.));
#17086=DIRECTION('ref_axis',(1.,0.,0.));
#17087=DIRECTION('',(0.,0.,-1.));
#17088=DIRECTION('center_axis',(0.,0.,1.));
#17089=DIRECTION('ref_axis',(1.,0.,0.));
#17090=DIRECTION('center_axis',(0.,0.,1.));
#17091=DIRECTION('ref_axis',(1.,0.,0.));
#17092=DIRECTION('center_axis',(0.,0.,1.));
#17093=DIRECTION('ref_axis',(1.,0.,0.));
#17094=DIRECTION('axis',(0.,0.,1.));
#17095=DIRECTION('refdir',(1.,0.,0.));
#17096=DIRECTION('axis',(0.,0.,1.));
#17097=DIRECTION('refdir',(1.,0.,0.));
#17098=DIRECTION('center_axis',(0.,0.,1.));
#17099=DIRECTION('ref_axis',(1.,0.,0.));
#17100=DIRECTION('',(-1.,0.,0.));
#17101=DIRECTION('center_axis',(0.,0.,1.));
#17102=DIRECTION('ref_axis',(1.,0.,0.));
#17103=DIRECTION('center_axis',(0.,0.,1.));
#17104=DIRECTION('ref_axis',(1.,0.,0.));
#17105=DIRECTION('',(0.,0.,-1.));
#17106=DIRECTION('center_axis',(0.,0.,1.));
#17107=DIRECTION('ref_axis',(1.,0.,0.));
#17108=DIRECTION('',(0.,0.,1.));
#17109=DIRECTION('center_axis',(0.,0.,-1.));
#17110=DIRECTION('ref_axis',(1.,0.,0.));
#17111=DIRECTION('center_axis',(0.,0.,1.));
#17112=DIRECTION('ref_axis',(1.,0.,0.));
#17113=DIRECTION('',(0.,0.,1.));
#17114=DIRECTION('center_axis',(0.,0.,1.));
#17115=DIRECTION('ref_axis',(1.,0.,0.));
#17116=DIRECTION('',(1.,0.,0.));
#17117=DIRECTION('center_axis',(0.,0.,1.));
#17118=DIRECTION('ref_axis',(1.,0.,0.));
#17119=DIRECTION('center_axis',(0.,0.,1.));
#17120=DIRECTION('ref_axis',(1.,0.,0.));
#17121=DIRECTION('',(0.,0.,-1.));
#17122=DIRECTION('center_axis',(0.,0.,1.));
#17123=DIRECTION('ref_axis',(1.,0.,0.));
#17124=DIRECTION('',(0.,0.,1.));
#17125=DIRECTION('center_axis',(0.,0.,-1.));
#17126=DIRECTION('ref_axis',(1.,0.,0.));
#17127=DIRECTION('center_axis',(0.,0.,1.));
#17128=DIRECTION('ref_axis',(1.,0.,0.));
#17129=DIRECTION('',(0.,0.,1.));
#17130=DIRECTION('center_axis',(0.,0.,1.));
#17131=DIRECTION('ref_axis',(1.,0.,0.));
#17132=DIRECTION('',(-1.,0.,0.));
#17133=DIRECTION('center_axis',(0.,0.,1.));
#17134=DIRECTION('ref_axis',(1.,0.,0.));
#17135=DIRECTION('center_axis',(0.,0.,1.));
#17136=DIRECTION('ref_axis',(1.,0.,0.));
#17137=DIRECTION('',(0.,0.,-1.));
#17138=DIRECTION('center_axis',(0.,0.,1.));
#17139=DIRECTION('ref_axis',(1.,0.,0.));
#17140=DIRECTION('',(0.,0.,1.));
#17141=DIRECTION('center_axis',(0.,0.,-1.));
#17142=DIRECTION('ref_axis',(1.,0.,0.));
#17143=DIRECTION('center_axis',(0.,0.,1.));
#17144=DIRECTION('ref_axis',(1.,0.,0.));
#17145=DIRECTION('',(0.,0.,1.));
#17146=DIRECTION('center_axis',(0.,0.,1.));
#17147=DIRECTION('ref_axis',(1.,0.,0.));
#17148=DIRECTION('',(1.,0.,0.));
#17149=DIRECTION('center_axis',(0.,0.,1.));
#17150=DIRECTION('ref_axis',(1.,0.,0.));
#17151=DIRECTION('center_axis',(0.,0.,1.));
#17152=DIRECTION('ref_axis',(1.,0.,0.));
#17153=DIRECTION('',(0.,0.,-1.));
#17154=DIRECTION('center_axis',(0.,0.,1.));
#17155=DIRECTION('ref_axis',(1.,0.,0.));
#17156=DIRECTION('',(0.,0.,1.));
#17157=DIRECTION('center_axis',(0.,0.,-1.));
#17158=DIRECTION('ref_axis',(1.,0.,0.));
#17159=DIRECTION('center_axis',(0.,0.,1.));
#17160=DIRECTION('ref_axis',(1.,0.,0.));
#17161=DIRECTION('',(0.,0.,1.));
#17162=DIRECTION('center_axis',(0.,-1.,0.));
#17163=DIRECTION('ref_axis',(0.,0.,-1.));
#17164=DIRECTION('',(-1.,0.,0.));
#17165=DIRECTION('',(-1.,0.,0.));
#17166=DIRECTION('',(0.,0.,1.));
#17167=DIRECTION('',(1.,0.,0.));
#17168=DIRECTION('',(0.,0.,-1.));
#17169=DIRECTION('',(-1.,0.,0.));
#17170=DIRECTION('center_axis',(0.,1.,0.));
#17171=DIRECTION('ref_axis',(0.,0.,1.));
#17172=DIRECTION('',(1.,0.,0.));
#17173=DIRECTION('',(1.,0.,0.));
#17174=DIRECTION('',(0.,0.,1.));
#17175=DIRECTION('',(1.,0.,0.));
#17176=DIRECTION('',(0.,0.,-1.));
#17177=DIRECTION('',(1.,0.,0.));
#17178=DIRECTION('center_axis',(-1.,0.,0.));
#17179=DIRECTION('ref_axis',(0.,0.,1.));
#17180=DIRECTION('',(0.,-1.,0.));
#17181=DIRECTION('',(0.,0.,1.));
#17182=DIRECTION('',(0.,1.,0.));
#17183=DIRECTION('',(0.,0.,-1.));
#17184=DIRECTION('',(0.,-1.,0.));
#17185=DIRECTION('',(0.,-1.,0.));
#17186=DIRECTION('',(0.,0.,1.));
#17187=DIRECTION('',(0.,-1.,0.));
#17188=DIRECTION('',(0.,0.,-1.));
#17189=DIRECTION('',(0.,-1.,0.));
#17190=DIRECTION('center_axis',(0.,0.,-1.));
#17191=DIRECTION('ref_axis',(0.,1.,0.));
#17192=DIRECTION('',(0.,1.,0.));
#17193=DIRECTION('',(1.,0.,0.));
#17194=DIRECTION('center_axis',(0.,-1.,0.));
#17195=DIRECTION('ref_axis',(0.,0.,-1.));
#17196=DIRECTION('',(0.,0.,-1.));
#17197=DIRECTION('',(1.,0.,0.));
#17198=DIRECTION('center_axis',(0.,0.,1.));
#17199=DIRECTION('ref_axis',(0.,-1.,0.));
#17200=DIRECTION('',(0.,-1.,0.));
#17201=DIRECTION('',(1.,0.,0.));
#17202=DIRECTION('center_axis',(0.,1.,0.));
#17203=DIRECTION('ref_axis',(0.,0.,1.));
#17204=DIRECTION('',(0.,0.,1.));
#17205=DIRECTION('',(1.,0.,0.));
#17206=DIRECTION('center_axis',(0.,0.,-1.));
#17207=DIRECTION('ref_axis',(0.,1.,0.));
#17208=DIRECTION('',(0.,1.,0.));
#17209=DIRECTION('center_axis',(0.,0.,-1.));
#17210=DIRECTION('ref_axis',(0.,1.,0.));
#17211=DIRECTION('',(0.,1.,0.));
#17212=DIRECTION('',(1.,0.,0.));
#17213=DIRECTION('center_axis',(0.,-1.,0.));
#17214=DIRECTION('ref_axis',(0.,0.,-1.));
#17215=DIRECTION('',(0.,0.,-1.));
#17216=DIRECTION('',(1.,0.,0.));
#17217=DIRECTION('center_axis',(0.,0.,-1.));
#17218=DIRECTION('ref_axis',(0.,1.,0.));
#17219=DIRECTION('',(0.,1.,0.));
#17220=DIRECTION('',(1.,0.,0.));
#17221=DIRECTION('center_axis',(0.,1.,0.));
#17222=DIRECTION('ref_axis',(0.,0.,1.));
#17223=DIRECTION('',(0.,0.,1.));
#17224=DIRECTION('',(1.,0.,0.));
#17225=DIRECTION('center_axis',(0.,0.,-1.));
#17226=DIRECTION('ref_axis',(0.,1.,0.));
#17227=DIRECTION('',(0.,1.,0.));
#17228=DIRECTION('center_axis',(1.,0.,0.));
#17229=DIRECTION('ref_axis',(0.,0.,-1.));
#17230=DIRECTION('axis',(0.,0.,1.));
#17231=DIRECTION('refdir',(1.,0.,0.));
#17232=DIRECTION('center_axis',(0.,0.,1.));
#17233=DIRECTION('ref_axis',(0.,-1.,0.));
#17234=DIRECTION('',(0.,-1.,0.));
#17235=DIRECTION('',(1.,0.,0.));
#17236=DIRECTION('',(0.,-1.,0.));
#17237=DIRECTION('',(1.,0.,0.));
#17238=DIRECTION('center_axis',(0.,1.,0.));
#17239=DIRECTION('ref_axis',(0.,0.,1.));
#17240=DIRECTION('',(0.,0.,1.));
#17241=DIRECTION('',(0.,0.,1.));
#17242=DIRECTION('',(1.,0.,0.));
#17243=DIRECTION('center_axis',(0.,0.,-1.));
#17244=DIRECTION('ref_axis',(0.,1.,0.));
#17245=DIRECTION('',(0.,1.,0.));
#17246=DIRECTION('',(0.,1.,0.));
#17247=DIRECTION('',(1.,0.,0.));
#17248=DIRECTION('center_axis',(0.,-1.,0.));
#17249=DIRECTION('ref_axis',(0.,0.,-1.));
#17250=DIRECTION('',(0.,0.,-1.));
#17251=DIRECTION('',(0.,0.,-1.));
#17252=DIRECTION('',(1.,0.,0.));
#17253=DIRECTION('center_axis',(0.,0.,-1.));
#17254=DIRECTION('ref_axis',(0.,1.,0.));
#17255=DIRECTION('',(0.,1.,0.));
#17256=DIRECTION('',(0.,1.,0.));
#17257=DIRECTION('',(1.,0.,0.));
#17258=DIRECTION('center_axis',(0.,1.,0.));
#17259=DIRECTION('ref_axis',(0.,0.,1.));
#17260=DIRECTION('',(0.,0.,1.));
#17261=DIRECTION('',(0.,0.,1.));
#17262=DIRECTION('',(1.,0.,0.));
#17263=DIRECTION('center_axis',(0.,0.,-1.));
#17264=DIRECTION('ref_axis',(0.,1.,0.));
#17265=DIRECTION('',(0.,1.,0.));
#17266=DIRECTION('',(0.,1.,0.));
#17267=DIRECTION('',(1.,0.,0.));
#17268=DIRECTION('center_axis',(0.,-1.,0.));
#17269=DIRECTION('ref_axis',(0.,0.,-1.));
#17270=DIRECTION('',(0.,0.,-1.));
#17271=DIRECTION('',(0.,0.,-1.));
#17272=DIRECTION('center_axis',(1.,0.,0.));
#17273=DIRECTION('ref_axis',(0.,0.,-1.));
#17274=DIRECTION('center_axis',(1.,0.,0.));
#17275=DIRECTION('ref_axis',(0.,0.,-1.));
#17276=DIRECTION('axis',(0.,0.,1.));
#17277=DIRECTION('refdir',(1.,0.,0.));
#17278=DIRECTION('center_axis',(0.,0.,-1.));
#17279=DIRECTION('ref_axis',(0.,-1.,0.));
#17280=DIRECTION('',(0.,1.,0.));
#17281=DIRECTION('',(-1.,0.,0.));
#17282=DIRECTION('',(0.,-1.,0.));
#17283=DIRECTION('',(-1.,0.,0.));
#17284=DIRECTION('center_axis',(0.,1.,0.));
#17285=DIRECTION('ref_axis',(0.,0.,-1.));
#17286=DIRECTION('',(0.,0.,1.));
#17287=DIRECTION('',(0.,0.,-1.));
#17288=DIRECTION('',(-1.,0.,0.));
#17289=DIRECTION('center_axis',(0.,0.,-1.));
#17290=DIRECTION('ref_axis',(0.,-1.,0.));
#17291=DIRECTION('',(0.,1.,0.));
#17292=DIRECTION('',(0.,-1.,0.));
#17293=DIRECTION('',(-1.,0.,0.));
#17294=DIRECTION('center_axis',(0.,-1.,0.));
#17295=DIRECTION('ref_axis',(0.,0.,1.));
#17296=DIRECTION('',(0.,0.,-1.));
#17297=DIRECTION('',(0.,0.,1.));
#17298=DIRECTION('',(-1.,0.,0.));
#17299=DIRECTION('center_axis',(0.,0.,-1.));
#17300=DIRECTION('ref_axis',(0.,-1.,0.));
#17301=DIRECTION('',(0.,1.,0.));
#17302=DIRECTION('',(0.,-1.,0.));
#17303=DIRECTION('',(-1.,0.,0.));
#17304=DIRECTION('center_axis',(0.,1.,0.));
#17305=DIRECTION('ref_axis',(0.,0.,-1.));
#17306=DIRECTION('',(0.,0.,1.));
#17307=DIRECTION('',(0.,0.,-1.));
#17308=DIRECTION('',(-1.,0.,0.));
#17309=DIRECTION('center_axis',(0.,0.,1.));
#17310=DIRECTION('ref_axis',(0.,1.,0.));
#17311=DIRECTION('',(0.,-1.,0.));
#17312=DIRECTION('',(0.,1.,0.));
#17313=DIRECTION('',(-1.,0.,0.));
#17314=DIRECTION('center_axis',(0.,-1.,0.));
#17315=DIRECTION('ref_axis',(0.,0.,1.));
#17316=DIRECTION('',(0.,0.,-1.));
#17317=DIRECTION('',(0.,0.,1.));
#17318=DIRECTION('center_axis',(1.,0.,0.));
#17319=DIRECTION('ref_axis',(0.,0.,-1.));
#17320=DIRECTION('center_axis',(-1.,0.,0.));
#17321=DIRECTION('ref_axis',(0.,0.,1.));
#17322=DIRECTION('',(0.,0.,1.));
#17323=DIRECTION('',(1.,0.,0.));
#17324=DIRECTION('',(0.,0.,1.));
#17325=DIRECTION('',(1.,0.,0.));
#17326=DIRECTION('',(0.,0.,1.));
#17327=DIRECTION('',(1.,0.,0.));
#17328=DIRECTION('axis',(0.,0.,1.));
#17329=DIRECTION('refdir',(1.,0.,0.));
#17330=DIRECTION('center_axis',(0.866025403784439,0.,-0.5));
#17331=DIRECTION('ref_axis',(0.5,0.,0.866025403784439));
#17332=DIRECTION('',(0.5,0.,0.866025403784439));
#17333=DIRECTION('',(0.,-1.,0.));
#17334=DIRECTION('',(0.5,0.,0.866025403784439));
#17335=DIRECTION('',(0.,-1.,0.));
#17336=DIRECTION('center_axis',(1.20185167898973E-16,0.,-1.));
#17337=DIRECTION('ref_axis',(1.,0.,1.20185167898973E-16));
#17338=DIRECTION('',(1.,0.,1.20185167898973E-16));
#17339=DIRECTION('',(0.,-1.,0.));
#17340=DIRECTION('',(1.,0.,1.20185167898973E-16));
#17341=DIRECTION('center_axis',(-0.866025403784439,0.,-0.5));
#17342=DIRECTION('ref_axis',(0.5,0.,-0.866025403784439));
#17343=DIRECTION('',(0.5,0.,-0.866025403784439));
#17344=DIRECTION('',(0.,-1.,0.));
#17345=DIRECTION('',(0.5,0.,-0.866025403784439));
#17346=DIRECTION('center_axis',(-0.866025403784439,0.,0.5));
#17347=DIRECTION('ref_axis',(-0.5,0.,-0.866025403784439));
#17348=DIRECTION('',(-0.5,0.,-0.866025403784439));
#17349=DIRECTION('',(0.,-1.,0.));
#17350=DIRECTION('',(-0.5,0.,-0.866025403784439));
#17351=DIRECTION('center_axis',(-2.40370335797945E-16,0.,1.));
#17352=DIRECTION('ref_axis',(-1.,0.,-2.40370335797945E-16));
#17353=DIRECTION('',(-1.,0.,-2.40370335797945E-16));
#17354=DIRECTION('',(0.,-1.,0.));
#17355=DIRECTION('',(-1.,0.,-2.40370335797945E-16));
#17356=DIRECTION('center_axis',(0.866025403784439,0.,0.5));
#17357=DIRECTION('ref_axis',(-0.5,0.,0.866025403784439));
#17358=DIRECTION('',(-0.5,0.,0.866025403784439));
#17359=DIRECTION('',(-0.5,0.,0.866025403784439));
#17360=DIRECTION('center_axis',(0.,-1.,0.));
#17361=DIRECTION('ref_axis',(0.,0.,-1.));
#17362=DIRECTION('center_axis',(0.,1.,0.));
#17363=DIRECTION('ref_axis',(0.,0.,1.));
#17364=DIRECTION('center_axis',(0.,-1.,0.));
#17365=DIRECTION('ref_axis',(1.,0.,0.));
#17366=DIRECTION('center_axis',(0.,-1.,0.));
#17367=DIRECTION('ref_axis',(1.,0.,0.));
#17368=DIRECTION('center_axis',(0.,-1.,0.));
#17369=DIRECTION('ref_axis',(1.,0.,0.));
#17370=DIRECTION('',(0.707106781186548,0.707106781186547,8.65956056235494E-17));
#17371=DIRECTION('center_axis',(0.,-1.,0.));
#17372=DIRECTION('ref_axis',(1.,0.,0.));
#17373=DIRECTION('center_axis',(0.,1.,0.));
#17374=DIRECTION('ref_axis',(1.,0.,0.));
#17375=DIRECTION('',(0.,1.,0.));
#17376=DIRECTION('center_axis',(0.,1.,0.));
#17377=DIRECTION('ref_axis',(1.,0.,0.));
#17378=DIRECTION('center_axis',(0.,-1.,0.));
#17379=DIRECTION('ref_axis',(1.,0.,0.));
#17380=DIRECTION('',(-0.707106781186548,0.707106781186547,-8.65956056235494E-17));
#17381=DIRECTION('center_axis',(0.,-1.,0.));
#17382=DIRECTION('ref_axis',(0.,0.,-1.));
#17383=DIRECTION('axis',(0.,0.,1.));
#17384=DIRECTION('refdir',(1.,0.,0.));
#17385=DIRECTION('center_axis',(0.866025403784439,0.,-0.5));
#17386=DIRECTION('ref_axis',(0.5,0.,0.866025403784439));
#17387=DIRECTION('',(-0.5,0.,-0.866025403784439));
#17388=DIRECTION('',(0.,-1.,0.));
#17389=DIRECTION('',(0.5,0.,0.866025403784439));
#17390=DIRECTION('',(0.,-1.,0.));
#17391=DIRECTION('center_axis',(1.20185167898973E-16,0.,-1.));
#17392=DIRECTION('ref_axis',(1.,0.,1.20185167898973E-16));
#17393=DIRECTION('',(-1.,0.,-1.20185167898973E-16));
#17394=DIRECTION('',(0.,-1.,0.));
#17395=DIRECTION('',(1.,0.,1.20185167898973E-16));
#17396=DIRECTION('center_axis',(-0.866025403784439,0.,-0.5));
#17397=DIRECTION('ref_axis',(0.5,0.,-0.866025403784439));
#17398=DIRECTION('',(-0.5,0.,0.866025403784439));
#17399=DIRECTION('',(0.,-1.,0.));
#17400=DIRECTION('',(0.5,0.,-0.866025403784439));
#17401=DIRECTION('center_axis',(-0.866025403784439,0.,0.5));
#17402=DIRECTION('ref_axis',(-0.5,0.,-0.866025403784439));
#17403=DIRECTION('',(0.5,0.,0.866025403784439));
#17404=DIRECTION('',(0.,-1.,0.));
#17405=DIRECTION('',(-0.5,0.,-0.866025403784439));
#17406=DIRECTION('center_axis',(-2.40370335797945E-16,0.,1.));
#17407=DIRECTION('ref_axis',(-1.,0.,-2.40370335797945E-16));
#17408=DIRECTION('',(1.,0.,2.40370335797945E-16));
#17409=DIRECTION('',(0.,-1.,0.));
#17410=DIRECTION('',(-1.,0.,-2.40370335797945E-16));
#17411=DIRECTION('center_axis',(0.866025403784439,0.,0.5));
#17412=DIRECTION('ref_axis',(-0.5,0.,0.866025403784439));
#17413=DIRECTION('',(0.5,0.,-0.866025403784439));
#17414=DIRECTION('',(-0.5,0.,0.866025403784439));
#17415=DIRECTION('center_axis',(0.,1.,0.));
#17416=DIRECTION('ref_axis',(1.,0.,0.));
#17417=DIRECTION('center_axis',(0.,-1.,0.));
#17418=DIRECTION('ref_axis',(0.,0.,-1.));
#17419=DIRECTION('center_axis',(0.,1.,0.));
#17420=DIRECTION('ref_axis',(1.,0.,0.));
#17421=DIRECTION('center_axis',(0.,1.,0.));
#17422=DIRECTION('ref_axis',(1.,0.,0.));
#17423=DIRECTION('center_axis',(0.,1.,0.));
#17424=DIRECTION('ref_axis',(0.,0.,1.));
#17425=DIRECTION('center_axis',(0.,-1.,0.));
#17426=DIRECTION('ref_axis',(1.,0.,0.));
#17427=DIRECTION('center_axis',(0.,-1.,0.));
#17428=DIRECTION('ref_axis',(1.,0.,0.));
#17429=DIRECTION('center_axis',(0.,-1.,0.));
#17430=DIRECTION('ref_axis',(1.,0.,0.));
#17431=DIRECTION('',(0.707106781186548,0.707106781186547,8.65956056235493E-17));
#17432=DIRECTION('center_axis',(0.,-1.,0.));
#17433=DIRECTION('ref_axis',(1.,0.,0.));
#17434=DIRECTION('center_axis',(0.,-1.,0.));
#17435=DIRECTION('ref_axis',(1.,0.,0.));
#17436=DIRECTION('',(0.,1.,0.));
#17437=DIRECTION('center_axis',(0.,1.,0.));
#17438=DIRECTION('ref_axis',(1.,0.,0.));
#17439=DIRECTION('center_axis',(0.,-1.,0.));
#17440=DIRECTION('ref_axis',(1.,0.,0.));
#17441=DIRECTION('',(-0.707106781186547,0.707106781186548,-8.65956056235493E-17));
#17442=DIRECTION('center_axis',(0.,-1.,0.));
#17443=DIRECTION('ref_axis',(0.,0.,-1.));
#17444=DIRECTION('center_axis',(0.,-1.,0.));
#17445=DIRECTION('ref_axis',(1.,0.,0.));
#17446=DIRECTION('center_axis',(0.,1.,0.));
#17447=DIRECTION('ref_axis',(1.,0.,0.));
#17448=DIRECTION('center_axis',(0.,1.,0.));
#17449=DIRECTION('ref_axis',(1.,0.,0.));
#17450=DIRECTION('',(-0.447213595499958,0.894427190999916,-5.47678698264203E-17));
#17451=DIRECTION('center_axis',(0.,-1.,0.));
#17452=DIRECTION('ref_axis',(1.,0.,0.));
#17453=DIRECTION('',(0.,1.,0.));
#17454=DIRECTION('axis',(0.,0.,1.));
#17455=DIRECTION('refdir',(1.,0.,0.));
#17456=DIRECTION('axis',(0.,0.,1.));
#17457=DIRECTION('refdir',(1.,0.,0.));
#17458=DIRECTION('center_axis',(0.,-1.,0.));
#17459=DIRECTION('ref_axis',(0.,0.,-1.));
#17460=DIRECTION('center_axis',(0.,-1.,0.));
#17461=DIRECTION('ref_axis',(1.,0.,0.));
#17462=DIRECTION('center_axis',(0.,-1.,0.));
#17463=DIRECTION('ref_axis',(1.,0.,0.));
#17464=DIRECTION('center_axis',(1.,0.,1.22464679914735E-16));
#17465=DIRECTION('ref_axis',(-1.22464679914735E-16,0.,1.));
#17466=DIRECTION('center_axis',(0.,1.,0.));
#17467=DIRECTION('ref_axis',(1.,0.,0.));
#17468=DIRECTION('center_axis',(0.,1.,0.));
#17469=DIRECTION('ref_axis',(1.,0.,0.));
#17470=DIRECTION('center_axis',(0.,-1.,0.));
#17471=DIRECTION('ref_axis',(1.,0.,0.));
#17472=DIRECTION('',(0.,1.,0.));
#17473=DIRECTION('center_axis',(0.,-1.,0.));
#17474=DIRECTION('ref_axis',(1.,0.,0.));
#17475=DIRECTION('center_axis',(0.,-1.,0.));
#17476=DIRECTION('ref_axis',(1.,0.,0.));
#17477=DIRECTION('center_axis',(0.,-1.,0.));
#17478=DIRECTION('ref_axis',(1.,0.,0.));
#17479=DIRECTION('',(0.,1.,0.));
#17480=DIRECTION('center_axis',(0.,-1.,0.));
#17481=DIRECTION('ref_axis',(1.,0.,0.));
#17482=DIRECTION('center_axis',(0.,1.,0.));
#17483=DIRECTION('ref_axis',(1.,0.,0.));
#17484=DIRECTION('',(-0.707106781186548,0.707106781186547,-8.65956056235494E-17));
#17485=DIRECTION('center_axis',(0.,-1.,0.));
#17486=DIRECTION('ref_axis',(1.,0.,0.));
#17487=DIRECTION('center_axis',(0.,1.,0.));
#17488=DIRECTION('ref_axis',(0.,0.,1.));
#17489=DIRECTION('center_axis',(0.,-1.,0.));
#17490=DIRECTION('ref_axis',(1.,0.,0.));
#17491=DIRECTION('center_axis',(0.,-1.,0.));
#17492=DIRECTION('ref_axis',(1.,0.,0.));
#17493=DIRECTION('',(0.,1.,0.));
#17494=DIRECTION('center_axis',(0.,-1.,0.));
#17495=DIRECTION('ref_axis',(0.,0.,-1.));
#17496=DIRECTION('center_axis',(0.,-1.,0.));
#17497=DIRECTION('ref_axis',(1.,0.,0.));
#17498=DIRECTION('center_axis',(0.,-1.,0.));
#17499=DIRECTION('ref_axis',(1.,0.,0.));
#17500=DIRECTION('',(0.707106781186548,0.707106781186547,8.65956056235494E-17));
#17501=DIRECTION('axis',(0.,0.,1.));
#17502=DIRECTION('refdir',(1.,0.,0.));
#17503=DIRECTION('center_axis',(0.,-1.,0.));
#17504=DIRECTION('ref_axis',(0.,0.,-1.));
#17505=DIRECTION('center_axis',(0.,-1.,0.));
#17506=DIRECTION('ref_axis',(1.,0.,0.));
#17507=DIRECTION('center_axis',(0.,-1.,0.));
#17508=DIRECTION('ref_axis',(1.,0.,0.));
#17509=DIRECTION('center_axis',(1.,0.,1.22464679914735E-16));
#17510=DIRECTION('ref_axis',(-1.22464679914735E-16,0.,1.));
#17511=DIRECTION('center_axis',(0.,1.,0.));
#17512=DIRECTION('ref_axis',(1.,0.,0.));
#17513=DIRECTION('center_axis',(0.,1.,0.));
#17514=DIRECTION('ref_axis',(1.,0.,0.));
#17515=DIRECTION('center_axis',(0.,-1.,0.));
#17516=DIRECTION('ref_axis',(1.,0.,0.));
#17517=DIRECTION('center_axis',(0.,-1.,0.));
#17518=DIRECTION('ref_axis',(1.,0.,0.));
#17519=DIRECTION('',(0.,1.,0.));
#17520=DIRECTION('center_axis',(0.,1.,0.));
#17521=DIRECTION('ref_axis',(0.,0.,1.));
#17522=DIRECTION('center_axis',(0.,-1.,0.));
#17523=DIRECTION('ref_axis',(1.,0.,0.));
#17524=DIRECTION('center_axis',(0.,-1.,0.));
#17525=DIRECTION('ref_axis',(1.,0.,0.));
#17526=DIRECTION('center_axis',(0.,-1.,0.));
#17527=DIRECTION('ref_axis',(1.,0.,0.));
#17528=DIRECTION('center_axis',(0.,-1.,0.));
#17529=DIRECTION('ref_axis',(1.,0.,0.));
#17530=DIRECTION('',(0.707106781186548,0.707106781186547,8.65956056235494E-17));
#17531=DIRECTION('center_axis',(0.,-1.,0.));
#17532=DIRECTION('ref_axis',(1.,0.,0.));
#17533=DIRECTION('center_axis',(0.,-1.,0.));
#17534=DIRECTION('ref_axis',(1.,0.,0.));
#17535=DIRECTION('',(0.,1.,0.));
#17536=DIRECTION('center_axis',(0.,1.,0.));
#17537=DIRECTION('ref_axis',(1.,0.,0.));
#17538=DIRECTION('center_axis',(0.,-1.,0.));
#17539=DIRECTION('ref_axis',(1.,0.,0.));
#17540=DIRECTION('',(-0.707106781186548,0.707106781186547,-8.65956056235494E-17));
#17541=DIRECTION('center_axis',(0.,-1.,0.));
#17542=DIRECTION('ref_axis',(0.,0.,-1.));
#17543=DIRECTION('center_axis',(0.,-1.,0.));
#17544=DIRECTION('ref_axis',(1.,0.,0.));
#17545=DIRECTION('',(0.,1.,0.));
#17546=DIRECTION('axis',(0.,0.,1.));
#17547=DIRECTION('refdir',(1.,0.,0.));
#17548=DIRECTION('center_axis',(0.,0.,1.));
#17549=DIRECTION('ref_axis',(1.,0.,0.));
#17550=DIRECTION('center_axis',(1.22464679914735E-16,-1.,0.));
#17551=DIRECTION('ref_axis',(-1.,-1.22464679914735E-16,0.));
#17552=DIRECTION('center_axis',(0.707106781186548,0.,0.707106781186548));
#17553=DIRECTION('ref_axis',(0.707106781186548,0.,-0.707106781186548));
#17554=DIRECTION('center_axis',(8.65956056235493E-17,-1.,-8.65956056235493E-17));
#17555=DIRECTION('ref_axis',(-0.707106781186548,-1.22464679914735E-16,0.707106781186548));
#17556=DIRECTION('center_axis',(1.,0.,0.));
#17557=DIRECTION('ref_axis',(6.12323399573677E-17,0.,-1.));
#17558=DIRECTION('center_axis',(7.49879891330929E-33,-1.,-1.22464679914735E-16));
#17559=DIRECTION('ref_axis',(-6.12323399573677E-17,-1.22464679914735E-16,
1.));
#17560=DIRECTION('center_axis',(0.707106781186548,0.,-0.707106781186548));
#17561=DIRECTION('ref_axis',(-0.707106781186548,0.,-0.707106781186548));
#17562=DIRECTION('center_axis',(-8.65956056235493E-17,-1.,-8.65956056235493E-17));
#17563=DIRECTION('ref_axis',(0.707106781186548,-1.22464679914735E-16,0.707106781186548));
#17564=DIRECTION('center_axis',(0.,0.,-1.));
#17565=DIRECTION('ref_axis',(-1.,0.,-1.22464679914735E-16));
#17566=DIRECTION('center_axis',(-1.22464679914735E-16,-1.,-1.49975978266186E-32));
#17567=DIRECTION('ref_axis',(1.,-1.22464679914735E-16,1.22464679914735E-16));
#17568=DIRECTION('center_axis',(-0.707106781186548,0.,-0.707106781186548));
#17569=DIRECTION('ref_axis',(-0.707106781186548,0.,0.707106781186548));
#17570=DIRECTION('center_axis',(-8.65956056235493E-17,-1.,8.65956056235493E-17));
#17571=DIRECTION('ref_axis',(0.707106781186548,-1.22464679914735E-16,-0.707106781186548));
#17572=DIRECTION('center_axis',(-1.,0.,0.));
#17573=DIRECTION('ref_axis',(-1.83697019872103E-16,0.,1.));
#17574=DIRECTION('center_axis',(-2.24963967399279E-32,-1.,1.22464679914735E-16));
#17575=DIRECTION('ref_axis',(1.83697019872103E-16,-1.22464679914735E-16,
-1.));
#17576=DIRECTION('center_axis',(-0.707106781186548,0.,0.707106781186548));
#17577=DIRECTION('ref_axis',(0.707106781186548,0.,0.707106781186548));
#17578=DIRECTION('center_axis',(8.65956056235493E-17,-1.,8.65956056235494E-17));
#17579=DIRECTION('ref_axis',(-0.707106781186548,-1.22464679914735E-16,-0.707106781186548));
#17580=DIRECTION('axis',(0.,0.,1.));
#17581=DIRECTION('refdir',(1.,0.,0.));
#17582=DIRECTION('center_axis',(0.,0.,1.));
#17583=DIRECTION('ref_axis',(1.,0.,0.));
#17584=DIRECTION('center_axis',(0.,-1.,0.));
#17585=DIRECTION('ref_axis',(0.,0.,-1.));
#17586=DIRECTION('center_axis',(0.,-1.,0.));
#17587=DIRECTION('ref_axis',(0.,0.,-1.));
#17588=DIRECTION('center_axis',(0.,1.,0.));
#17589=DIRECTION('ref_axis',(1.,0.,0.));
#17590=DIRECTION('center_axis',(0.,1.,0.));
#17591=DIRECTION('ref_axis',(1.,0.,0.));
#17592=DIRECTION('center_axis',(0.,1.,0.));
#17593=DIRECTION('ref_axis',(1.,0.,0.));
#17594=DIRECTION('center_axis',(0.,1.,0.));
#17595=DIRECTION('ref_axis',(1.,0.,0.));
#17596=DIRECTION('',(0.,-1.,0.));
#17597=DIRECTION('center_axis',(0.,-1.,0.));
#17598=DIRECTION('ref_axis',(1.,0.,0.));
#17599=DIRECTION('center_axis',(0.,1.,0.));
#17600=DIRECTION('ref_axis',(1.,0.,0.));
#17601=DIRECTION('center_axis',(0.,1.,0.));
#17602=DIRECTION('ref_axis',(1.,0.,0.));
#17603=DIRECTION('center_axis',(0.,1.,0.));
#17604=DIRECTION('ref_axis',(1.,0.,0.));
#17605=DIRECTION('center_axis',(0.,1.,0.));
#17606=DIRECTION('ref_axis',(1.,0.,0.));
#17607=DIRECTION('center_axis',(0.,1.,0.));
#17608=DIRECTION('ref_axis',(1.,0.,0.));
#17609=DIRECTION('center_axis',(0.,1.,0.));
#17610=DIRECTION('ref_axis',(1.,0.,0.));
#17611=DIRECTION('center_axis',(0.,-1.,0.));
#17612=DIRECTION('ref_axis',(1.,0.,0.));
#17613=DIRECTION('center_axis',(0.,-1.,0.));
#17614=DIRECTION('ref_axis',(0.,0.,-1.));
#17615=DIRECTION('center_axis',(6.12323399573677E-17,0.,1.));
#17616=DIRECTION('ref_axis',(1.,0.,0.));
#17617=DIRECTION('center_axis',(0.,-1.,0.));
#17618=DIRECTION('ref_axis',(0.,0.,-1.));
#17619=DIRECTION('center_axis',(0.,1.,0.));
#17620=DIRECTION('ref_axis',(1.,0.,0.));
#17621=DIRECTION('center_axis',(0.,-1.,0.));
#17622=DIRECTION('ref_axis',(1.,0.,0.));
#17623=DIRECTION('center_axis',(0.,-1.,0.));
#17624=DIRECTION('ref_axis',(0.,0.,-1.));
#17625=DIRECTION('center_axis',(0.,0.,1.));
#17626=DIRECTION('ref_axis',(1.,0.,0.));
#17627=DIRECTION('center_axis',(0.,-1.,0.));
#17628=DIRECTION('ref_axis',(0.,0.,-1.));
#17629=DIRECTION('center_axis',(0.,1.,0.));
#17630=DIRECTION('ref_axis',(1.,0.,0.));
#17631=DIRECTION('center_axis',(0.,-1.,0.));
#17632=DIRECTION('ref_axis',(1.,0.,0.));
#17633=DIRECTION('center_axis',(0.,-1.,0.));
#17634=DIRECTION('ref_axis',(0.,0.,-1.));
#17635=DIRECTION('center_axis',(0.,0.,1.));
#17636=DIRECTION('ref_axis',(1.,0.,0.));
#17637=DIRECTION('center_axis',(0.,-1.,0.));
#17638=DIRECTION('ref_axis',(0.,0.,-1.));
#17639=DIRECTION('center_axis',(0.,1.,0.));
#17640=DIRECTION('ref_axis',(1.,0.,0.));
#17641=DIRECTION('center_axis',(0.,-1.,0.));
#17642=DIRECTION('ref_axis',(1.,0.,0.));
#17643=DIRECTION('center_axis',(0.,-1.,0.));
#17644=DIRECTION('ref_axis',(0.,0.,-1.));
#17645=DIRECTION('center_axis',(0.,0.,1.));
#17646=DIRECTION('ref_axis',(1.,0.,0.));
#17647=DIRECTION('center_axis',(0.,-1.,0.));
#17648=DIRECTION('ref_axis',(0.,0.,-1.));
#17649=DIRECTION('center_axis',(0.,1.,0.));
#17650=DIRECTION('ref_axis',(1.,0.,0.));
#17651=DIRECTION('center_axis',(0.,-1.,0.));
#17652=DIRECTION('ref_axis',(1.,0.,0.));
#17653=DIRECTION('center_axis',(0.,-1.,0.));
#17654=DIRECTION('ref_axis',(0.,0.,-1.));
#17655=DIRECTION('center_axis',(6.12323399573676E-17,0.,1.));
#17656=DIRECTION('ref_axis',(1.,0.,0.));
#17657=DIRECTION('center_axis',(0.,-1.,0.));
#17658=DIRECTION('ref_axis',(0.,0.,-1.));
#17659=DIRECTION('center_axis',(0.,1.,0.));
#17660=DIRECTION('ref_axis',(1.,0.,0.));
#17661=DIRECTION('center_axis',(0.,-1.,0.));
#17662=DIRECTION('ref_axis',(1.,0.,0.));
#17663=DIRECTION('center_axis',(0.,-1.,0.));
#17664=DIRECTION('ref_axis',(0.,0.,-1.));
#17665=DIRECTION('center_axis',(0.,0.,1.));
#17666=DIRECTION('ref_axis',(1.,0.,0.));
#17667=DIRECTION('center_axis',(0.,-1.,0.));
#17668=DIRECTION('ref_axis',(0.,0.,-1.));
#17669=DIRECTION('center_axis',(0.,1.,0.));
#17670=DIRECTION('ref_axis',(1.,0.,0.));
#17671=DIRECTION('center_axis',(0.,1.,0.));
#17672=DIRECTION('ref_axis',(1.,0.,0.));
#17673=DIRECTION('',(0.,1.,0.));
#17674=DIRECTION('center_axis',(0.,-1.,0.));
#17675=DIRECTION('ref_axis',(1.,0.,0.));
#17676=DIRECTION('center_axis',(0.,-1.,0.));
#17677=DIRECTION('ref_axis',(1.,0.,0.));
#17678=DIRECTION('center_axis',(0.,1.,0.));
#17679=DIRECTION('ref_axis',(1.,0.,0.));
#17680=DIRECTION('center_axis',(0.,-1.,0.));
#17681=DIRECTION('ref_axis',(0.,0.,-1.));
#17682=DIRECTION('center_axis',(0.,0.,1.));
#17683=DIRECTION('ref_axis',(1.,0.,0.));
#17684=DIRECTION('center_axis',(0.,-1.,0.));
#17685=DIRECTION('ref_axis',(0.,0.,-1.));
#17686=DIRECTION('center_axis',(0.,-1.,0.));
#17687=DIRECTION('ref_axis',(-1.,0.,0.));
#17688=DIRECTION('center_axis',(0.,1.,0.));
#17689=DIRECTION('ref_axis',(1.,0.,0.));
#17690=DIRECTION('axis',(0.,0.,1.));
#17691=DIRECTION('refdir',(1.,0.,0.));
#17692=DIRECTION('center_axis',(0.,1.,0.));
#17693=DIRECTION('ref_axis',(0.,0.,1.));
#17694=DIRECTION('center_axis',(0.,-1.,0.));
#17695=DIRECTION('ref_axis',(1.,0.,0.));
#17696=DIRECTION('center_axis',(0.,-1.,0.));
#17697=DIRECTION('ref_axis',(1.,0.,0.));
#17698=DIRECTION('center_axis',(0.,-1.,0.));
#17699=DIRECTION('ref_axis',(1.,0.,0.));
#17700=DIRECTION('center_axis',(0.,-1.,0.));
#17701=DIRECTION('ref_axis',(1.,0.,0.));
#17702=DIRECTION('',(0.,1.,0.));
#17703=DIRECTION('center_axis',(0.,-1.,0.));
#17704=DIRECTION('ref_axis',(0.,0.,-1.));
#17705=DIRECTION('center_axis',(0.,-1.,0.));
#17706=DIRECTION('ref_axis',(1.,0.,0.));
#17707=DIRECTION('center_axis',(0.,-1.,0.));
#17708=DIRECTION('ref_axis',(1.,0.,0.));
#17709=DIRECTION('',(0.,1.,0.));
#17710=DIRECTION('center_axis',(0.,1.,0.));
#17711=DIRECTION('ref_axis',(0.,0.,1.));
#17712=DIRECTION('center_axis',(0.,-1.,0.));
#17713=DIRECTION('ref_axis',(1.,0.,0.));
#17714=DIRECTION('center_axis',(0.,-1.,0.));
#17715=DIRECTION('ref_axis',(1.,0.,0.));
#17716=DIRECTION('center_axis',(0.,-1.,0.));
#17717=DIRECTION('ref_axis',(1.,0.,0.));
#17718=DIRECTION('center_axis',(0.,-1.,0.));
#17719=DIRECTION('ref_axis',(1.,0.,0.));
#17720=DIRECTION('',(0.,1.,0.));
#17721=DIRECTION('center_axis',(0.,-1.,0.));
#17722=DIRECTION('ref_axis',(0.,0.,-1.));
#17723=DIRECTION('center_axis',(0.,-1.,0.));
#17724=DIRECTION('ref_axis',(1.,0.,0.));
#17725=DIRECTION('center_axis',(0.,-1.,0.));
#17726=DIRECTION('ref_axis',(1.,0.,0.));
#17727=DIRECTION('',(0.,1.,0.));
#17728=DIRECTION('',(0.,0.,1.));
#17729=DIRECTION('',(1.,0.,0.));
#17730=DIRECTION('',(0.,0.,1.));
#17731=DIRECTION('',(1.,0.,0.));
#17732=DIRECTION('',(0.,0.,1.));
#17733=DIRECTION('',(1.,0.,0.));
#17734=DIRECTION('',(0.,0.,1.));
#17735=DIRECTION('',(1.,0.,0.));
#17736=DIRECTION('',(0.,0.,1.));
#17737=DIRECTION('',(1.,0.,0.));
#17738=DIRECTION('axis',(0.,0.,1.));
#17739=DIRECTION('refdir',(1.,0.,0.));
#17740=DIRECTION('axis',(0.,0.,1.));
#17741=DIRECTION('refdir',(1.,0.,0.));
#17742=DIRECTION('center_axis',(0.,0.,1.));
#17743=DIRECTION('ref_axis',(1.,0.,0.));
#17744=DIRECTION('center_axis',(0.,0.,1.));
#17745=DIRECTION('ref_axis',(1.,0.,0.));
#17746=DIRECTION('',(0.,0.,1.));
#17747=DIRECTION('center_axis',(0.,0.,-1.));
#17748=DIRECTION('ref_axis',(1.,0.,0.));
#17749=DIRECTION('center_axis',(0.,0.,1.));
#17750=DIRECTION('ref_axis',(1.,0.,0.));
#17751=DIRECTION('center_axis',(-1.,0.,0.));
#17752=DIRECTION('ref_axis',(0.,-1.,0.));
#17753=DIRECTION('',(0.,0.,-1.));
#17754=DIRECTION('',(0.,-1.,0.));
#17755=DIRECTION('',(0.,0.,1.));
#17756=DIRECTION('',(0.,1.,0.));
#17757=DIRECTION('center_axis',(0.,0.,1.));
#17758=DIRECTION('ref_axis',(1.,0.,0.));
#17759=DIRECTION('center_axis',(0.,0.,-1.));
#17760=DIRECTION('ref_axis',(1.,0.,0.));
#17761=DIRECTION('',(-1.,0.,0.));
#17762=DIRECTION('',(0.,-1.,0.));
#17763=DIRECTION('center_axis',(0.,-1.,0.));
#17764=DIRECTION('ref_axis',(1.,0.,0.));
#17765=DIRECTION('',(1.,0.,0.));
#17766=DIRECTION('',(0.,0.,1.));
#17767=DIRECTION('center_axis',(1.,0.,0.));
#17768=DIRECTION('ref_axis',(0.,1.,0.));
#17769=DIRECTION('',(0.,0.,1.));
#17770=DIRECTION('',(0.,1.,0.));
#17771=DIRECTION('center_axis',(0.,0.,1.));
#17772=DIRECTION('ref_axis',(1.,0.,0.));
#17773=DIRECTION('center_axis',(0.,0.,1.));
#17774=DIRECTION('ref_axis',(1.,0.,0.));
#17775=DIRECTION('center_axis',(0.,0.,1.));
#17776=DIRECTION('ref_axis',(1.,0.,0.));
#17777=DIRECTION('center_axis',(0.,0.,1.));
#17778=DIRECTION('ref_axis',(1.,0.,0.));
#17779=DIRECTION('center_axis',(0.,0.,1.));
#17780=DIRECTION('ref_axis',(1.,0.,0.));
#17781=DIRECTION('center_axis',(0.,0.,1.));
#17782=DIRECTION('ref_axis',(1.,0.,0.));
#17783=DIRECTION('center_axis',(0.,0.,1.));
#17784=DIRECTION('ref_axis',(1.,0.,0.));
#17785=DIRECTION('center_axis',(0.,0.,-1.));
#17786=DIRECTION('ref_axis',(1.,0.,0.));
#17787=DIRECTION('center_axis',(0.,0.,1.));
#17788=DIRECTION('ref_axis',(1.,0.,0.));
#17789=DIRECTION('',(0.,0.,-1.));
#17790=DIRECTION('center_axis',(0.,0.,1.));
#17791=DIRECTION('ref_axis',(1.,0.,0.));
#17792=DIRECTION('',(0.,0.,-1.));
#17793=DIRECTION('center_axis',(0.,0.,1.));
#17794=DIRECTION('ref_axis',(1.,0.,0.));
#17795=DIRECTION('center_axis',(0.,0.,1.));
#17796=DIRECTION('ref_axis',(1.,0.,0.));
#17797=DIRECTION('center_axis',(0.,0.,1.));
#17798=DIRECTION('ref_axis',(1.,0.,0.));
#17799=DIRECTION('',(0.,0.,-1.));
#17800=DIRECTION('center_axis',(0.,0.,1.));
#17801=DIRECTION('ref_axis',(1.,0.,0.));
#17802=DIRECTION('center_axis',(0.,0.,1.));
#17803=DIRECTION('ref_axis',(1.,0.,0.));
#17804=DIRECTION('axis',(0.,0.,1.));
#17805=DIRECTION('refdir',(1.,0.,0.));
#17806=DIRECTION('center_axis',(0.,0.,1.));
#17807=DIRECTION('ref_axis',(1.,0.,0.));
#17808=DIRECTION('center_axis',(0.,0.,-1.));
#17809=DIRECTION('ref_axis',(1.,0.,0.));
#17810=DIRECTION('',(0.,0.,-1.));
#17811=DIRECTION('center_axis',(0.,0.,-1.));
#17812=DIRECTION('ref_axis',(1.,0.,0.));
#17813=DIRECTION('center_axis',(0.,0.,1.));
#17814=DIRECTION('ref_axis',(1.,0.,0.));
#17815=DIRECTION('center_axis',(0.,0.,1.));
#17816=DIRECTION('ref_axis',(1.,0.,0.));
#17817=DIRECTION('',(0.,0.,-1.));
#17818=DIRECTION('center_axis',(0.,0.,1.));
#17819=DIRECTION('ref_axis',(1.,0.,0.));
#17820=DIRECTION('center_axis',(0.,0.,1.));
#17821=DIRECTION('ref_axis',(1.,0.,0.));
#17822=DIRECTION('center_axis',(0.,0.,1.));
#17823=DIRECTION('ref_axis',(1.,0.,0.));
#17824=DIRECTION('axis',(0.,0.,1.));
#17825=DIRECTION('refdir',(1.,0.,0.));
#17826=DIRECTION('center_axis',(0.,0.,1.));
#17827=DIRECTION('ref_axis',(1.,0.,0.));
#17828=DIRECTION('center_axis',(0.,0.,-1.));
#17829=DIRECTION('ref_axis',(1.,0.,0.));
#17830=DIRECTION('',(0.,0.,-1.));
#17831=DIRECTION('center_axis',(0.,0.,-1.));
#17832=DIRECTION('ref_axis',(1.,0.,0.));
#17833=DIRECTION('center_axis',(0.,0.,1.));
#17834=DIRECTION('ref_axis',(1.,0.,0.));
#17835=DIRECTION('center_axis',(0.,0.,1.));
#17836=DIRECTION('ref_axis',(1.,0.,0.));
#17837=DIRECTION('',(0.,0.,-1.));
#17838=DIRECTION('center_axis',(0.,0.,1.));
#17839=DIRECTION('ref_axis',(1.,0.,0.));
#17840=DIRECTION('center_axis',(0.,0.,1.));
#17841=DIRECTION('ref_axis',(1.,0.,0.));
#17842=DIRECTION('center_axis',(0.,0.,1.));
#17843=DIRECTION('ref_axis',(1.,0.,0.));
#17844=DIRECTION('axis',(0.,0.,1.));
#17845=DIRECTION('refdir',(1.,0.,0.));
#17846=DIRECTION('center_axis',(0.,0.,1.));
#17847=DIRECTION('ref_axis',(1.,0.,0.));
#17848=DIRECTION('center_axis',(0.,0.,-1.));
#17849=DIRECTION('ref_axis',(1.,0.,0.));
#17850=DIRECTION('',(0.,0.,-1.));
#17851=DIRECTION('center_axis',(0.,0.,-1.));
#17852=DIRECTION('ref_axis',(1.,0.,0.));
#17853=DIRECTION('center_axis',(0.,0.,1.));
#17854=DIRECTION('ref_axis',(1.,0.,0.));
#17855=DIRECTION('center_axis',(0.,0.,1.));
#17856=DIRECTION('ref_axis',(1.,0.,0.));
#17857=DIRECTION('',(0.,0.,-1.));
#17858=DIRECTION('center_axis',(0.,0.,1.));
#17859=DIRECTION('ref_axis',(1.,0.,0.));
#17860=DIRECTION('center_axis',(0.,0.,1.));
#17861=DIRECTION('ref_axis',(1.,0.,0.));
#17862=DIRECTION('center_axis',(0.,0.,1.));
#17863=DIRECTION('ref_axis',(1.,0.,0.));
#17864=DIRECTION('axis',(0.,0.,1.));
#17865=DIRECTION('refdir',(1.,0.,0.));
#17866=DIRECTION('center_axis',(1.,0.,0.));
#17867=DIRECTION('ref_axis',(0.,0.,-1.));
#17868=DIRECTION('',(0.,0.,1.));
#17869=DIRECTION('center_axis',(1.,0.,0.));
#17870=DIRECTION('ref_axis',(0.,0.,-1.));
#17871=DIRECTION('center_axis',(1.,0.,0.));
#17872=DIRECTION('ref_axis',(0.,0.,-1.));
#17873=DIRECTION('',(0.,0.,-1.));
#17874=DIRECTION('center_axis',(1.,0.,0.));
#17875=DIRECTION('ref_axis',(0.,0.,-1.));
#17876=DIRECTION('center_axis',(1.,0.,0.));
#17877=DIRECTION('ref_axis',(0.,0.,-1.));
#17878=DIRECTION('',(0.,0.,1.));
#17879=DIRECTION('center_axis',(1.,0.,0.));
#17880=DIRECTION('ref_axis',(0.,0.,-1.));
#17881=DIRECTION('center_axis',(1.,0.,0.));
#17882=DIRECTION('ref_axis',(0.,0.,-1.));
#17883=DIRECTION('center_axis',(1.,0.,0.));
#17884=DIRECTION('ref_axis',(0.,0.,-1.));
#17885=DIRECTION('',(1.,0.,0.));
#17886=DIRECTION('center_axis',(1.,0.,0.));
#17887=DIRECTION('ref_axis',(0.,0.,-1.));
#17888=DIRECTION('',(0.,0.,-1.));
#17889=DIRECTION('center_axis',(0.,0.,1.));
#17890=DIRECTION('ref_axis',(1.,0.,0.));
#17891=DIRECTION('center_axis',(0.,0.,-1.));
#17892=DIRECTION('ref_axis',(1.,0.,0.));
#17893=DIRECTION('',(0.,0.,-1.));
#17894=DIRECTION('center_axis',(0.,0.,-1.));
#17895=DIRECTION('ref_axis',(1.,0.,0.));
#17896=DIRECTION('center_axis',(0.,0.,1.));
#17897=DIRECTION('ref_axis',(1.,0.,0.));
#17898=DIRECTION('center_axis',(0.,0.,1.));
#17899=DIRECTION('ref_axis',(1.,0.,0.));
#17900=DIRECTION('',(0.,0.,-1.));
#17901=DIRECTION('center_axis',(0.,0.,1.));
#17902=DIRECTION('ref_axis',(1.,0.,0.));
#17903=DIRECTION('center_axis',(0.,0.,1.));
#17904=DIRECTION('ref_axis',(1.,0.,0.));
#17905=DIRECTION('center_axis',(0.,0.,1.));
#17906=DIRECTION('ref_axis',(1.,0.,0.));
#17907=DIRECTION('axis',(0.,0.,1.));
#17908=DIRECTION('refdir',(1.,0.,0.));
#17909=DIRECTION('center_axis',(0.,-1.,0.));
#17910=DIRECTION('ref_axis',(1.,0.,0.));
#17911=DIRECTION('',(-1.,0.,0.));
#17912=DIRECTION('',(0.,0.,1.));
#17913=DIRECTION('',(1.,0.,0.));
#17914=DIRECTION('',(0.,0.,1.));
#17915=DIRECTION('center_axis',(-1.,0.,0.));
#17916=DIRECTION('ref_axis',(0.,-1.,0.));
#17917=DIRECTION('',(0.,1.,0.));
#17918=DIRECTION('',(0.,-1.,0.));
#17919=DIRECTION('',(0.,0.,1.));
#17920=DIRECTION('center_axis',(0.,1.,0.));
#17921=DIRECTION('ref_axis',(-1.,0.,0.));
#17922=DIRECTION('',(1.,0.,0.));
#17923=DIRECTION('',(-1.,0.,0.));
#17924=DIRECTION('',(0.,0.,1.));
#17925=DIRECTION('center_axis',(1.,0.,0.));
#17926=DIRECTION('ref_axis',(0.,1.,0.));
#17927=DIRECTION('',(0.,-1.,0.));
#17928=DIRECTION('',(0.,1.,0.));
#17929=DIRECTION('center_axis',(0.,0.,1.));
#17930=DIRECTION('ref_axis',(1.,0.,0.));
#17931=DIRECTION('center_axis',(0.,0.,1.));
#17932=DIRECTION('ref_axis',(1.,0.,0.));
#17933=DIRECTION('axis',(0.,0.,1.));
#17934=DIRECTION('refdir',(1.,0.,0.));
#17935=DIRECTION('center_axis',(0.,0.,1.));
#17936=DIRECTION('ref_axis',(1.,0.,0.));
#17937=DIRECTION('center_axis',(0.,0.,-1.));
#17938=DIRECTION('ref_axis',(1.,0.,0.));
#17939=DIRECTION('',(0.,0.,-1.));
#17940=DIRECTION('center_axis',(0.,0.,-1.));
#17941=DIRECTION('ref_axis',(1.,0.,0.));
#17942=DIRECTION('center_axis',(0.,0.,1.));
#17943=DIRECTION('ref_axis',(1.,0.,0.));
#17944=DIRECTION('center_axis',(0.,0.,1.));
#17945=DIRECTION('ref_axis',(1.,0.,0.));
#17946=DIRECTION('',(0.,0.,-1.));
#17947=DIRECTION('center_axis',(0.,0.,1.));
#17948=DIRECTION('ref_axis',(1.,0.,0.));
#17949=DIRECTION('center_axis',(0.,0.,1.));
#17950=DIRECTION('ref_axis',(1.,0.,0.));
#17951=DIRECTION('center_axis',(0.,0.,1.));
#17952=DIRECTION('ref_axis',(1.,0.,0.));
#17953=DIRECTION('axis',(0.,0.,1.));
#17954=DIRECTION('refdir',(1.,0.,0.));
#17955=DIRECTION('center_axis',(1.,0.,0.));
#17956=DIRECTION('ref_axis',(0.,0.,-1.));
#17957=DIRECTION('',(0.,0.,1.));
#17958=DIRECTION('',(0.,1.,0.));
#17959=DIRECTION('',(0.,0.,-1.));
#17960=DIRECTION('',(0.,-1.,0.));
#17961=DIRECTION('center_axis',(0.,0.,-1.));
#17962=DIRECTION('ref_axis',(-1.,0.,0.));
#17963=DIRECTION('',(1.,0.,0.));
#17964=DIRECTION('',(0.,-1.,0.));
#17965=DIRECTION('',(-1.,0.,0.));
#17966=DIRECTION('center_axis',(-1.,0.,0.));
#17967=DIRECTION('ref_axis',(0.,0.,1.));
#17968=DIRECTION('',(0.,0.,-1.));
#17969=DIRECTION('',(0.,1.,0.));
#17970=DIRECTION('',(0.,0.,1.));
#17971=DIRECTION('center_axis',(0.,1.,0.));
#17972=DIRECTION('ref_axis',(1.,0.,0.));
#17973=DIRECTION('center_axis',(0.,-1.,0.));
#17974=DIRECTION('ref_axis',(1.,0.,0.));
#17975=DIRECTION('',(-0.587785252292473,0.,0.809016994374947));
#17976=DIRECTION('center_axis',(0.,-1.,0.));
#17977=DIRECTION('ref_axis',(1.,0.,0.));
#17978=DIRECTION('',(-0.809016994374948,0.,0.587785252292473));
#17979=DIRECTION('center_axis',(0.,-1.,0.));
#17980=DIRECTION('ref_axis',(1.,0.,0.));
#17981=DIRECTION('',(-0.951056516295154,0.,0.309016994374947));
#17982=DIRECTION('center_axis',(0.,-1.,0.));
#17983=DIRECTION('ref_axis',(1.,0.,0.));
#17984=DIRECTION('',(-1.,0.,-1.83697019872103E-16));
#17985=DIRECTION('center_axis',(0.,-1.,0.));
#17986=DIRECTION('ref_axis',(1.,0.,0.));
#17987=DIRECTION('',(-0.951056516295154,0.,-0.309016994374948));
#17988=DIRECTION('center_axis',(0.,-1.,0.));
#17989=DIRECTION('ref_axis',(1.,0.,0.));
#17990=DIRECTION('',(-0.809016994374947,0.,-0.587785252292473));
#17991=DIRECTION('center_axis',(0.,-1.,0.));
#17992=DIRECTION('ref_axis',(1.,0.,0.));
#17993=DIRECTION('',(-0.587785252292473,0.,-0.809016994374948));
#17994=DIRECTION('center_axis',(0.,-1.,0.));
#17995=DIRECTION('ref_axis',(1.,0.,0.));
#17996=DIRECTION('',(-0.309016994374947,0.,-0.951056516295154));
#17997=DIRECTION('center_axis',(0.,-1.,0.));
#17998=DIRECTION('ref_axis',(1.,0.,0.));
#17999=DIRECTION('',(1.22464679914735E-16,0.,-1.));
#18000=DIRECTION('center_axis',(0.,-1.,0.));
#18001=DIRECTION('ref_axis',(1.,0.,0.));
#18002=DIRECTION('',(0.309016994374948,0.,-0.951056516295154));
#18003=DIRECTION('center_axis',(0.,-1.,0.));
#18004=DIRECTION('ref_axis',(1.,0.,0.));
#18005=DIRECTION('',(0.587785252292473,0.,-0.809016994374947));
#18006=DIRECTION('center_axis',(0.,-1.,0.));
#18007=DIRECTION('ref_axis',(1.,0.,0.));
#18008=DIRECTION('',(0.809016994374948,0.,-0.587785252292473));
#18009=DIRECTION('center_axis',(0.,-1.,0.));
#18010=DIRECTION('ref_axis',(1.,0.,0.));
#18011=DIRECTION('',(0.951056516295154,0.,-0.309016994374947));
#18012=DIRECTION('center_axis',(0.,-1.,0.));
#18013=DIRECTION('ref_axis',(1.,0.,0.));
#18014=DIRECTION('',(1.,0.,6.12323399573677E-17));
#18015=DIRECTION('center_axis',(0.,-1.,0.));
#18016=DIRECTION('ref_axis',(1.,0.,0.));
#18017=DIRECTION('',(0.951056516295154,0.,0.309016994374948));
#18018=DIRECTION('center_axis',(0.,-1.,0.));
#18019=DIRECTION('ref_axis',(1.,0.,0.));
#18020=DIRECTION('',(0.809016994374947,0.,0.587785252292473));
#18021=DIRECTION('center_axis',(0.,-1.,0.));
#18022=DIRECTION('ref_axis',(1.,0.,0.));
#18023=DIRECTION('',(0.587785252292473,0.,0.809016994374947));
#18024=DIRECTION('center_axis',(0.,-1.,0.));
#18025=DIRECTION('ref_axis',(1.,0.,0.));
#18026=DIRECTION('',(0.309016994374947,0.,0.951056516295154));
#18027=DIRECTION('center_axis',(0.,-1.,0.));
#18028=DIRECTION('ref_axis',(1.,0.,0.));
#18029=DIRECTION('',(0.,0.,1.));
#18030=DIRECTION('center_axis',(0.,-1.,0.));
#18031=DIRECTION('ref_axis',(1.,0.,0.));
#18032=DIRECTION('',(-0.309016994374948,0.,0.951056516295154));
#18033=DIRECTION('center_axis',(0.,1.,0.));
#18034=DIRECTION('ref_axis',(1.,0.,0.));
#18035=DIRECTION('center_axis',(0.,1.,0.));
#18036=DIRECTION('ref_axis',(6.12323399573677E-17,0.,1.));
#18037=DIRECTION('center_axis',(0.,-1.,0.));
#18038=DIRECTION('ref_axis',(1.,0.,0.));
#18039=DIRECTION('center_axis',(0.,1.,0.));
#18040=DIRECTION('ref_axis',(1.,0.,0.));
#18041=DIRECTION('center_axis',(0.,1.,0.));
#18042=DIRECTION('ref_axis',(1.,0.,0.));
#18043=DIRECTION('',(0.,-1.,0.));
#18044=DIRECTION('center_axis',(0.,-1.,0.));
#18045=DIRECTION('ref_axis',(1.,0.,0.));
#18046=DIRECTION('center_axis',(0.,1.,0.));
#18047=DIRECTION('ref_axis',(1.,0.,0.));
#18048=DIRECTION('',(0.,-1.,0.));
#18049=DIRECTION('',(0.,1.,0.));
#18050=DIRECTION('center_axis',(0.951056516295154,0.,0.309016994374948));
#18051=DIRECTION('ref_axis',(0.309016994374948,0.,-0.951056516295154));
#18052=DIRECTION('',(0.309016994374948,0.,-0.951056516295154));
#18053=DIRECTION('',(0.,1.,0.));
#18054=DIRECTION('',(0.,1.,0.));
#18055=DIRECTION('center_axis',(0.,1.,0.));
#18056=DIRECTION('ref_axis',(1.,0.,0.));
#18057=DIRECTION('center_axis',(0.,1.,0.));
#18058=DIRECTION('ref_axis',(1.,0.,0.));
#18059=DIRECTION('',(0.,-1.,0.));
#18060=DIRECTION('',(0.,1.,0.));
#18061=DIRECTION('center_axis',(0.809016994374947,0.,0.587785252292473));
#18062=DIRECTION('ref_axis',(0.587785252292473,0.,-0.809016994374947));
#18063=DIRECTION('',(0.587785252292473,0.,-0.809016994374947));
#18064=DIRECTION('',(0.,1.,0.));
#18065=DIRECTION('',(0.,1.,0.));
#18066=DIRECTION('center_axis',(0.,1.,0.));
#18067=DIRECTION('ref_axis',(1.,0.,0.));
#18068=DIRECTION('center_axis',(0.,1.,0.));
#18069=DIRECTION('ref_axis',(1.,0.,0.));
#18070=DIRECTION('',(0.,-1.,0.));
#18071=DIRECTION('',(0.,1.,0.));
#18072=DIRECTION('center_axis',(0.587785252292473,0.,0.809016994374948));
#18073=DIRECTION('ref_axis',(0.809016994374948,0.,-0.587785252292473));
#18074=DIRECTION('',(0.809016994374948,0.,-0.587785252292473));
#18075=DIRECTION('',(0.,1.,0.));
#18076=DIRECTION('',(0.,1.,0.));
#18077=DIRECTION('center_axis',(0.,1.,0.));
#18078=DIRECTION('ref_axis',(1.,0.,0.));
#18079=DIRECTION('center_axis',(0.,1.,0.));
#18080=DIRECTION('ref_axis',(1.,0.,0.));
#18081=DIRECTION('',(0.,-1.,0.));
#18082=DIRECTION('',(0.,1.,0.));
#18083=DIRECTION('center_axis',(0.309016994374947,0.,0.951056516295154));
#18084=DIRECTION('ref_axis',(0.951056516295154,0.,-0.309016994374947));
#18085=DIRECTION('',(0.951056516295154,0.,-0.309016994374947));
#18086=DIRECTION('',(0.,1.,0.));
#18087=DIRECTION('',(0.,1.,0.));
#18088=DIRECTION('center_axis',(0.,1.,0.));
#18089=DIRECTION('ref_axis',(1.,0.,0.));
#18090=DIRECTION('center_axis',(0.,1.,0.));
#18091=DIRECTION('ref_axis',(1.,0.,0.));
#18092=DIRECTION('',(0.,-1.,0.));
#18093=DIRECTION('',(0.,1.,0.));
#18094=DIRECTION('center_axis',(-1.83697019872103E-16,0.,1.));
#18095=DIRECTION('ref_axis',(1.,0.,1.83697019872103E-16));
#18096=DIRECTION('',(1.,0.,1.83697019872103E-16));
#18097=DIRECTION('',(0.,1.,0.));
#18098=DIRECTION('',(0.,1.,0.));
#18099=DIRECTION('center_axis',(0.,1.,0.));
#18100=DIRECTION('ref_axis',(1.,0.,0.));
#18101=DIRECTION('center_axis',(0.,1.,0.));
#18102=DIRECTION('ref_axis',(1.,0.,0.));
#18103=DIRECTION('',(0.,-1.,0.));
#18104=DIRECTION('',(0.,1.,0.));
#18105=DIRECTION('center_axis',(-0.309016994374948,0.,0.951056516295154));
#18106=DIRECTION('ref_axis',(0.951056516295154,0.,0.309016994374948));
#18107=DIRECTION('',(0.951056516295154,0.,0.309016994374948));
#18108=DIRECTION('',(0.,1.,0.));
#18109=DIRECTION('',(0.,1.,0.));
#18110=DIRECTION('center_axis',(0.,1.,0.));
#18111=DIRECTION('ref_axis',(1.,0.,0.));
#18112=DIRECTION('center_axis',(0.,1.,0.));
#18113=DIRECTION('ref_axis',(1.,0.,0.));
#18114=DIRECTION('',(0.,-1.,0.));
#18115=DIRECTION('',(0.,1.,0.));
#18116=DIRECTION('center_axis',(-0.587785252292473,0.,0.809016994374947));
#18117=DIRECTION('ref_axis',(0.809016994374947,0.,0.587785252292473));
#18118=DIRECTION('',(0.809016994374947,0.,0.587785252292473));
#18119=DIRECTION('',(0.,1.,0.));
#18120=DIRECTION('',(0.,1.,0.));
#18121=DIRECTION('center_axis',(0.,1.,0.));
#18122=DIRECTION('ref_axis',(1.,0.,0.));
#18123=DIRECTION('center_axis',(0.,1.,0.));
#18124=DIRECTION('ref_axis',(1.,0.,0.));
#18125=DIRECTION('',(0.,-1.,0.));
#18126=DIRECTION('',(0.,1.,0.));
#18127=DIRECTION('center_axis',(-0.809016994374948,0.,0.587785252292473));
#18128=DIRECTION('ref_axis',(0.587785252292473,0.,0.809016994374948));
#18129=DIRECTION('',(0.587785252292473,0.,0.809016994374948));
#18130=DIRECTION('',(0.,1.,0.));
#18131=DIRECTION('',(0.,1.,0.));
#18132=DIRECTION('center_axis',(0.,1.,0.));
#18133=DIRECTION('ref_axis',(1.,0.,0.));
#18134=DIRECTION('center_axis',(0.,1.,0.));
#18135=DIRECTION('ref_axis',(1.,0.,0.));
#18136=DIRECTION('',(0.,-1.,0.));
#18137=DIRECTION('',(0.,1.,0.));
#18138=DIRECTION('center_axis',(-0.951056516295154,0.,0.309016994374947));
#18139=DIRECTION('ref_axis',(0.309016994374947,0.,0.951056516295154));
#18140=DIRECTION('',(0.309016994374947,0.,0.951056516295154));
#18141=DIRECTION('',(0.,1.,0.));
#18142=DIRECTION('',(0.,1.,0.));
#18143=DIRECTION('center_axis',(0.,1.,0.));
#18144=DIRECTION('ref_axis',(1.,0.,0.));
#18145=DIRECTION('center_axis',(0.,1.,0.));
#18146=DIRECTION('ref_axis',(1.,0.,0.));
#18147=DIRECTION('',(0.,-1.,0.));
#18148=DIRECTION('',(0.,1.,0.));
#18149=DIRECTION('center_axis',(-1.,0.,-1.22464679914735E-16));
#18150=DIRECTION('ref_axis',(-1.22464679914735E-16,0.,1.));
#18151=DIRECTION('',(-1.22464679914735E-16,0.,1.));
#18152=DIRECTION('',(0.,1.,0.));
#18153=DIRECTION('',(0.,1.,0.));
#18154=DIRECTION('center_axis',(0.,1.,0.));
#18155=DIRECTION('ref_axis',(1.,0.,0.));
#18156=DIRECTION('center_axis',(0.,1.,0.));
#18157=DIRECTION('ref_axis',(1.,0.,0.));
#18158=DIRECTION('',(0.,-1.,0.));
#18159=DIRECTION('',(0.,1.,0.));
#18160=DIRECTION('center_axis',(-0.951056516295154,0.,-0.309016994374948));
#18161=DIRECTION('ref_axis',(-0.309016994374948,0.,0.951056516295154));
#18162=DIRECTION('',(-0.309016994374948,0.,0.951056516295154));
#18163=DIRECTION('',(0.,1.,0.));
#18164=DIRECTION('',(0.,1.,0.));
#18165=DIRECTION('center_axis',(0.,1.,0.));
#18166=DIRECTION('ref_axis',(1.,0.,0.));
#18167=DIRECTION('center_axis',(0.,1.,0.));
#18168=DIRECTION('ref_axis',(1.,0.,0.));
#18169=DIRECTION('',(0.,-1.,0.));
#18170=DIRECTION('',(0.,1.,0.));
#18171=DIRECTION('center_axis',(-0.809016994374947,0.,-0.587785252292473));
#18172=DIRECTION('ref_axis',(-0.587785252292473,0.,0.809016994374947));
#18173=DIRECTION('',(-0.587785252292473,0.,0.809016994374947));
#18174=DIRECTION('',(0.,1.,0.));
#18175=DIRECTION('',(0.,1.,0.));
#18176=DIRECTION('center_axis',(0.,1.,0.));
#18177=DIRECTION('ref_axis',(1.,0.,0.));
#18178=DIRECTION('center_axis',(0.,1.,0.));
#18179=DIRECTION('ref_axis',(1.,0.,0.));
#18180=DIRECTION('',(0.,-1.,0.));
#18181=DIRECTION('',(0.,1.,0.));
#18182=DIRECTION('center_axis',(-0.587785252292473,0.,-0.809016994374948));
#18183=DIRECTION('ref_axis',(-0.809016994374948,0.,0.587785252292473));
#18184=DIRECTION('',(-0.809016994374948,0.,0.587785252292473));
#18185=DIRECTION('',(0.,1.,0.));
#18186=DIRECTION('',(0.,1.,0.));
#18187=DIRECTION('center_axis',(0.,1.,0.));
#18188=DIRECTION('ref_axis',(1.,0.,0.));
#18189=DIRECTION('center_axis',(0.,1.,0.));
#18190=DIRECTION('ref_axis',(1.,0.,0.));
#18191=DIRECTION('',(0.,-1.,0.));
#18192=DIRECTION('',(0.,1.,0.));
#18193=DIRECTION('center_axis',(-0.309016994374947,0.,-0.951056516295154));
#18194=DIRECTION('ref_axis',(-0.951056516295154,0.,0.309016994374947));
#18195=DIRECTION('',(-0.951056516295154,0.,0.309016994374947));
#18196=DIRECTION('',(0.,1.,0.));
#18197=DIRECTION('',(0.,1.,0.));
#18198=DIRECTION('center_axis',(0.,1.,0.));
#18199=DIRECTION('ref_axis',(1.,0.,0.));
#18200=DIRECTION('center_axis',(0.,1.,0.));
#18201=DIRECTION('ref_axis',(1.,0.,0.));
#18202=DIRECTION('',(0.,-1.,0.));
#18203=DIRECTION('',(0.,1.,0.));
#18204=DIRECTION('center_axis',(6.12323399573677E-17,0.,-1.));
#18205=DIRECTION('ref_axis',(-1.,0.,-6.12323399573677E-17));
#18206=DIRECTION('',(-1.,0.,-6.12323399573677E-17));
#18207=DIRECTION('',(0.,1.,0.));
#18208=DIRECTION('',(0.,1.,0.));
#18209=DIRECTION('center_axis',(0.,1.,0.));
#18210=DIRECTION('ref_axis',(1.,0.,0.));
#18211=DIRECTION('center_axis',(0.,1.,0.));
#18212=DIRECTION('ref_axis',(1.,0.,0.));
#18213=DIRECTION('',(0.,-1.,0.));
#18214=DIRECTION('',(0.,1.,0.));
#18215=DIRECTION('center_axis',(0.309016994374948,0.,-0.951056516295154));
#18216=DIRECTION('ref_axis',(-0.951056516295154,0.,-0.309016994374948));
#18217=DIRECTION('',(-0.951056516295154,0.,-0.309016994374948));
#18218=DIRECTION('',(0.,1.,0.));
#18219=DIRECTION('',(0.,1.,0.));
#18220=DIRECTION('center_axis',(0.,1.,0.));
#18221=DIRECTION('ref_axis',(1.,0.,0.));
#18222=DIRECTION('center_axis',(0.,1.,0.));
#18223=DIRECTION('ref_axis',(1.,0.,0.));
#18224=DIRECTION('',(0.,-1.,0.));
#18225=DIRECTION('',(0.,1.,0.));
#18226=DIRECTION('center_axis',(0.587785252292473,0.,-0.809016994374947));
#18227=DIRECTION('ref_axis',(-0.809016994374947,0.,-0.587785252292473));
#18228=DIRECTION('',(-0.809016994374947,0.,-0.587785252292473));
#18229=DIRECTION('',(0.,1.,0.));
#18230=DIRECTION('',(0.,1.,0.));
#18231=DIRECTION('center_axis',(0.,1.,0.));
#18232=DIRECTION('ref_axis',(1.,0.,0.));
#18233=DIRECTION('center_axis',(0.,1.,0.));
#18234=DIRECTION('ref_axis',(1.,0.,0.));
#18235=DIRECTION('',(0.,-1.,0.));
#18236=DIRECTION('',(0.,1.,0.));
#18237=DIRECTION('center_axis',(0.809016994374947,0.,-0.587785252292473));
#18238=DIRECTION('ref_axis',(-0.587785252292473,0.,-0.809016994374947));
#18239=DIRECTION('',(-0.587785252292473,0.,-0.809016994374947));
#18240=DIRECTION('',(0.,1.,0.));
#18241=DIRECTION('',(0.,1.,0.));
#18242=DIRECTION('center_axis',(0.,1.,0.));
#18243=DIRECTION('ref_axis',(1.,0.,0.));
#18244=DIRECTION('center_axis',(0.,1.,0.));
#18245=DIRECTION('ref_axis',(1.,0.,0.));
#18246=DIRECTION('',(0.,-1.,0.));
#18247=DIRECTION('',(0.,1.,0.));
#18248=DIRECTION('center_axis',(0.951056516295154,0.,-0.309016994374947));
#18249=DIRECTION('ref_axis',(-0.309016994374947,0.,-0.951056516295154));
#18250=DIRECTION('',(-0.309016994374947,0.,-0.951056516295154));
#18251=DIRECTION('',(0.,1.,0.));
#18252=DIRECTION('',(0.,1.,0.));
#18253=DIRECTION('center_axis',(0.,1.,0.));
#18254=DIRECTION('ref_axis',(1.,0.,0.));
#18255=DIRECTION('center_axis',(0.,1.,0.));
#18256=DIRECTION('ref_axis',(1.,0.,0.));
#18257=DIRECTION('',(0.,-1.,0.));
#18258=DIRECTION('',(0.,1.,0.));
#18259=DIRECTION('center_axis',(1.,0.,0.));
#18260=DIRECTION('ref_axis',(0.,0.,-1.));
#18261=DIRECTION('',(0.,0.,-1.));
#18262=DIRECTION('',(0.,1.,0.));
#18263=DIRECTION('',(0.,1.,0.));
#18264=DIRECTION('center_axis',(0.,1.,0.));
#18265=DIRECTION('ref_axis',(1.,0.,0.));
#18266=DIRECTION('center_axis',(0.,1.,0.));
#18267=DIRECTION('ref_axis',(1.,0.,0.));
#18268=DIRECTION('center_axis',(0.,1.,0.));
#18269=DIRECTION('ref_axis',(1.,0.,0.));
#18270=DIRECTION('axis',(0.,0.,1.));
#18271=DIRECTION('refdir',(1.,0.,0.));
#18272=DIRECTION('axis',(0.,0.,1.));
#18273=DIRECTION('refdir',(1.,0.,0.));
#18274=DIRECTION('center_axis',(0.,0.,1.));
#18275=DIRECTION('ref_axis',(1.,0.,0.));
#18276=DIRECTION('center_axis',(0.,0.,1.));
#18277=DIRECTION('ref_axis',(1.,0.,0.));
#18278=DIRECTION('',(0.,0.,1.));
#18279=DIRECTION('center_axis',(0.,0.,-1.));
#18280=DIRECTION('ref_axis',(1.,0.,0.));
#18281=DIRECTION('center_axis',(0.,0.,1.));
#18282=DIRECTION('ref_axis',(1.,0.,0.));
#18283=DIRECTION('center_axis',(-0.996917333733128,-0.0784590957278475,
0.));
#18284=DIRECTION('ref_axis',(0.0784590957278475,-0.996917333733128,0.));
#18285=DIRECTION('',(0.,0.,-1.));
#18286=DIRECTION('',(0.0784590957278475,-0.996917333733128,0.));
#18287=DIRECTION('',(0.,0.,1.));
#18288=DIRECTION('',(-0.0784590957278475,0.996917333733128,0.));
#18289=DIRECTION('center_axis',(0.,0.,1.));
#18290=DIRECTION('ref_axis',(1.,0.,0.));
#18291=DIRECTION('center_axis',(0.,0.,-1.));
#18292=DIRECTION('ref_axis',(1.,0.,0.));
#18293=DIRECTION('',(-0.996917333733128,-0.0784590957278448,0.));
#18294=DIRECTION('',(0.0784590957278475,-0.996917333733128,0.));
#18295=DIRECTION('center_axis',(0.0784590957278448,-0.996917333733128,0.));
#18296=DIRECTION('ref_axis',(0.996917333733128,0.0784590957278448,0.));
#18297=DIRECTION('',(0.996917333733128,0.0784590957278448,0.));
#18298=DIRECTION('',(0.,0.,1.));
#18299=DIRECTION('center_axis',(0.996917333733128,0.0784590957278475,0.));
#18300=DIRECTION('ref_axis',(-0.0784590957278475,0.996917333733128,0.));
#18301=DIRECTION('',(0.,0.,1.));
#18302=DIRECTION('',(-0.0784590957278475,0.996917333733128,0.));
#18303=DIRECTION('center_axis',(0.,0.,1.));
#18304=DIRECTION('ref_axis',(1.,0.,0.));
#18305=DIRECTION('center_axis',(0.,0.,1.));
#18306=DIRECTION('ref_axis',(1.,0.,0.));
#18307=DIRECTION('center_axis',(0.,0.,1.));
#18308=DIRECTION('ref_axis',(1.,0.,0.));
#18309=DIRECTION('center_axis',(0.,0.,1.));
#18310=DIRECTION('ref_axis',(1.,0.,0.));
#18311=DIRECTION('center_axis',(0.,0.,1.));
#18312=DIRECTION('ref_axis',(1.,0.,0.));
#18313=DIRECTION('center_axis',(0.,0.,1.));
#18314=DIRECTION('ref_axis',(1.,0.,0.));
#18315=DIRECTION('center_axis',(0.,0.,1.));
#18316=DIRECTION('ref_axis',(1.,0.,0.));
#18317=DIRECTION('center_axis',(0.,0.,-1.));
#18318=DIRECTION('ref_axis',(1.,0.,0.));
#18319=DIRECTION('center_axis',(0.,0.,1.));
#18320=DIRECTION('ref_axis',(1.,0.,0.));
#18321=DIRECTION('',(0.,0.,-1.));
#18322=DIRECTION('center_axis',(0.,0.,1.));
#18323=DIRECTION('ref_axis',(1.,0.,0.));
#18324=DIRECTION('',(0.,0.,-1.));
#18325=DIRECTION('center_axis',(0.,0.,1.));
#18326=DIRECTION('ref_axis',(1.,0.,0.));
#18327=DIRECTION('center_axis',(0.,0.,1.));
#18328=DIRECTION('ref_axis',(1.,0.,0.));
#18329=DIRECTION('center_axis',(0.,0.,1.));
#18330=DIRECTION('ref_axis',(1.,0.,0.));
#18331=DIRECTION('',(0.,0.,-1.));
#18332=DIRECTION('center_axis',(0.,0.,1.));
#18333=DIRECTION('ref_axis',(1.,0.,0.));
#18334=DIRECTION('center_axis',(0.,0.,1.));
#18335=DIRECTION('ref_axis',(1.,0.,0.));
#18336=DIRECTION('axis',(0.,0.,1.));
#18337=DIRECTION('refdir',(1.,0.,0.));
#18338=DIRECTION('center_axis',(0.,0.,1.));
#18339=DIRECTION('ref_axis',(1.,0.,0.));
#18340=DIRECTION('center_axis',(0.,0.,-1.));
#18341=DIRECTION('ref_axis',(1.,0.,0.));
#18342=DIRECTION('',(0.,0.,-1.));
#18343=DIRECTION('center_axis',(0.,0.,-1.));
#18344=DIRECTION('ref_axis',(1.,0.,0.));
#18345=DIRECTION('center_axis',(0.,0.,1.));
#18346=DIRECTION('ref_axis',(1.,0.,0.));
#18347=DIRECTION('center_axis',(0.,0.,1.));
#18348=DIRECTION('ref_axis',(1.,0.,0.));
#18349=DIRECTION('',(0.,0.,-1.));
#18350=DIRECTION('center_axis',(0.,0.,1.));
#18351=DIRECTION('ref_axis',(1.,0.,0.));
#18352=DIRECTION('center_axis',(0.,0.,1.));
#18353=DIRECTION('ref_axis',(1.,0.,0.));
#18354=DIRECTION('center_axis',(0.,0.,1.));
#18355=DIRECTION('ref_axis',(1.,0.,0.));
#18356=DIRECTION('axis',(0.,0.,1.));
#18357=DIRECTION('refdir',(1.,0.,0.));
#18358=DIRECTION('center_axis',(0.,0.,1.));
#18359=DIRECTION('ref_axis',(1.,0.,0.));
#18360=DIRECTION('center_axis',(0.,0.,-1.));
#18361=DIRECTION('ref_axis',(1.,0.,0.));
#18362=DIRECTION('',(0.,0.,-1.));
#18363=DIRECTION('center_axis',(0.,0.,-1.));
#18364=DIRECTION('ref_axis',(1.,0.,0.));
#18365=DIRECTION('center_axis',(0.,0.,1.));
#18366=DIRECTION('ref_axis',(1.,0.,0.));
#18367=DIRECTION('center_axis',(0.,0.,1.));
#18368=DIRECTION('ref_axis',(1.,0.,0.));
#18369=DIRECTION('',(0.,0.,-1.));
#18370=DIRECTION('center_axis',(0.,0.,1.));
#18371=DIRECTION('ref_axis',(1.,0.,0.));
#18372=DIRECTION('center_axis',(0.,0.,1.));
#18373=DIRECTION('ref_axis',(1.,0.,0.));
#18374=DIRECTION('center_axis',(0.,0.,1.));
#18375=DIRECTION('ref_axis',(1.,0.,0.));
#18376=DIRECTION('axis',(0.,0.,1.));
#18377=DIRECTION('refdir',(1.,0.,0.));
#18378=DIRECTION('center_axis',(1.,0.,0.));
#18379=DIRECTION('ref_axis',(0.,0.,-1.));
#18380=DIRECTION('',(1.,0.,0.));
#18381=DIRECTION('center_axis',(0.,0.,1.));
#18382=DIRECTION('ref_axis',(1.,0.,0.));
#18383=DIRECTION('center_axis',(0.,0.,-1.));
#18384=DIRECTION('ref_axis',(1.,0.,0.));
#18385=DIRECTION('',(0.,0.,-1.));
#18386=DIRECTION('center_axis',(0.,0.,-1.));
#18387=DIRECTION('ref_axis',(1.,0.,0.));
#18388=DIRECTION('center_axis',(0.,0.,1.));
#18389=DIRECTION('ref_axis',(1.,0.,0.));
#18390=DIRECTION('center_axis',(0.,0.,1.));
#18391=DIRECTION('ref_axis',(1.,0.,0.));
#18392=DIRECTION('',(0.,0.,-1.));
#18393=DIRECTION('center_axis',(0.,0.,1.));
#18394=DIRECTION('ref_axis',(1.,0.,0.));
#18395=DIRECTION('center_axis',(0.,0.,1.));
#18396=DIRECTION('ref_axis',(1.,0.,0.));
#18397=DIRECTION('center_axis',(0.,0.,1.));
#18398=DIRECTION('ref_axis',(1.,0.,0.));
#18399=DIRECTION('axis',(0.,0.,1.));
#18400=DIRECTION('refdir',(1.,0.,0.));
#18401=DIRECTION('center_axis',(0.0784590957278448,-0.996917333733128,0.));
#18402=DIRECTION('ref_axis',(0.996917333733128,0.0784590957278448,0.));
#18403=DIRECTION('',(-0.996917333733128,-0.0784590957278448,0.));
#18404=DIRECTION('',(0.,0.,1.));
#18405=DIRECTION('',(0.996917333733128,0.0784590957278448,0.));
#18406=DIRECTION('',(0.,0.,1.));
#18407=DIRECTION('center_axis',(-0.996917333733128,-0.078459095727846,0.));
#18408=DIRECTION('ref_axis',(0.078459095727846,-0.996917333733128,0.));
#18409=DIRECTION('',(-0.078459095727846,0.996917333733128,0.));
#18410=DIRECTION('',(0.078459095727846,-0.996917333733128,0.));
#18411=DIRECTION('',(0.,0.,1.));
#18412=DIRECTION('center_axis',(-0.078459095727845,0.996917333733128,0.));
#18413=DIRECTION('ref_axis',(-0.996917333733128,-0.078459095727845,0.));
#18414=DIRECTION('',(0.996917333733128,0.078459095727845,0.));
#18415=DIRECTION('',(-0.996917333733128,-0.078459095727845,0.));
#18416=DIRECTION('',(0.,0.,1.));
#18417=DIRECTION('center_axis',(0.996917333733128,0.078459095727846,0.));
#18418=DIRECTION('ref_axis',(-0.078459095727846,0.996917333733128,0.));
#18419=DIRECTION('',(0.078459095727846,-0.996917333733128,0.));
#18420=DIRECTION('',(-0.078459095727846,0.996917333733128,0.));
#18421=DIRECTION('center_axis',(0.,0.,1.));
#18422=DIRECTION('ref_axis',(1.,0.,0.));
#18423=DIRECTION('center_axis',(0.,0.,1.));
#18424=DIRECTION('ref_axis',(1.,0.,0.));
#18425=DIRECTION('axis',(0.,0.,1.));
#18426=DIRECTION('refdir',(1.,0.,0.));
#18427=DIRECTION('center_axis',(0.,0.,1.));
#18428=DIRECTION('ref_axis',(1.,0.,0.));
#18429=DIRECTION('center_axis',(0.,0.,-1.));
#18430=DIRECTION('ref_axis',(1.,0.,0.));
#18431=DIRECTION('',(0.,0.,-1.));
#18432=DIRECTION('center_axis',(0.,0.,-1.));
#18433=DIRECTION('ref_axis',(1.,0.,0.));
#18434=DIRECTION('center_axis',(0.,0.,1.));
#18435=DIRECTION('ref_axis',(1.,0.,0.));
#18436=DIRECTION('center_axis',(0.,0.,1.));
#18437=DIRECTION('ref_axis',(1.,0.,0.));
#18438=DIRECTION('',(0.,0.,-1.));
#18439=DIRECTION('center_axis',(0.,0.,1.));
#18440=DIRECTION('ref_axis',(1.,0.,0.));
#18441=DIRECTION('center_axis',(0.,0.,1.));
#18442=DIRECTION('ref_axis',(1.,0.,0.));
#18443=DIRECTION('center_axis',(0.,0.,1.));
#18444=DIRECTION('ref_axis',(1.,0.,0.));
#18445=DIRECTION('axis',(0.,0.,1.));
#18446=DIRECTION('refdir',(1.,0.,0.));
#18447=DIRECTION('center_axis',(0.,1.,0.));
#18448=DIRECTION('ref_axis',(1.,0.,0.));
#18449=DIRECTION('center_axis',(0.,1.,0.));
#18450=DIRECTION('ref_axis',(1.,0.,0.));
#18451=DIRECTION('center_axis',(0.866025403784439,0.,-0.5));
#18452=DIRECTION('ref_axis',(0.5,0.,0.866025403784439));
#18453=DIRECTION('',(0.5,0.,0.866025403784439));
#18454=DIRECTION('',(0.,-1.,0.));
#18455=DIRECTION('',(0.5,0.,0.866025403784439));
#18456=DIRECTION('',(0.,-1.,0.));
#18457=DIRECTION('center_axis',(1.20185167898973E-16,0.,-1.));
#18458=DIRECTION('ref_axis',(1.,0.,1.20185167898973E-16));
#18459=DIRECTION('',(1.,0.,1.20185167898973E-16));
#18460=DIRECTION('',(0.,-1.,0.));
#18461=DIRECTION('',(1.,0.,1.20185167898973E-16));
#18462=DIRECTION('center_axis',(-0.866025403784439,0.,-0.5));
#18463=DIRECTION('ref_axis',(0.5,0.,-0.866025403784439));
#18464=DIRECTION('',(0.5,0.,-0.866025403784439));
#18465=DIRECTION('',(0.,-1.,0.));
#18466=DIRECTION('',(0.5,0.,-0.866025403784439));
#18467=DIRECTION('center_axis',(-0.866025403784439,0.,0.5));
#18468=DIRECTION('ref_axis',(-0.5,0.,-0.866025403784439));
#18469=DIRECTION('',(-0.5,0.,-0.866025403784439));
#18470=DIRECTION('',(0.,-1.,0.));
#18471=DIRECTION('',(-0.5,0.,-0.866025403784439));
#18472=DIRECTION('center_axis',(-2.40370335797945E-16,0.,1.));
#18473=DIRECTION('ref_axis',(-1.,0.,-2.40370335797945E-16));
#18474=DIRECTION('',(-1.,0.,-2.40370335797945E-16));
#18475=DIRECTION('',(0.,-1.,0.));
#18476=DIRECTION('',(-1.,0.,-2.40370335797945E-16));
#18477=DIRECTION('center_axis',(0.866025403784439,0.,0.5));
#18478=DIRECTION('ref_axis',(-0.5,0.,0.866025403784439));
#18479=DIRECTION('',(-0.5,0.,0.866025403784439));
#18480=DIRECTION('',(-0.5,0.,0.866025403784439));
#18481=DIRECTION('center_axis',(0.,-1.,0.));
#18482=DIRECTION('ref_axis',(0.,0.,-1.));
#18483=DIRECTION('center_axis',(0.,1.,0.));
#18484=DIRECTION('ref_axis',(0.,0.,1.));
#18485=DIRECTION('center_axis',(0.,-1.,0.));
#18486=DIRECTION('ref_axis',(1.,0.,0.));
#18487=DIRECTION('center_axis',(0.,-1.,0.));
#18488=DIRECTION('ref_axis',(1.,0.,0.));
#18489=DIRECTION('center_axis',(0.,-1.,0.));
#18490=DIRECTION('ref_axis',(1.,0.,0.));
#18491=DIRECTION('',(0.707106781186548,0.707106781186547,8.65956056235494E-17));
#18492=DIRECTION('center_axis',(0.,-1.,0.));
#18493=DIRECTION('ref_axis',(1.,0.,0.));
#18494=DIRECTION('',(0.,1.,0.));
#18495=DIRECTION('axis',(0.,0.,1.));
#18496=DIRECTION('refdir',(1.,0.,0.));
#18497=DIRECTION('center_axis',(0.996917333733128,0.,-0.0784590957278449));
#18498=DIRECTION('ref_axis',(-0.0784590957278449,0.,-0.996917333733128));
#18499=DIRECTION('',(0.0784590957278449,0.,0.996917333733128));
#18500=DIRECTION('',(0.,1.,0.));
#18501=DIRECTION('',(-0.0784590957278449,0.,-0.996917333733128));
#18502=DIRECTION('',(0.,-1.,0.));
#18503=DIRECTION('center_axis',(-0.0784590957278449,0.,-0.996917333733128));
#18504=DIRECTION('ref_axis',(-0.996917333733128,0.,0.0784590957278449));
#18505=DIRECTION('',(0.996917333733128,0.,-0.0784590957278449));
#18506=DIRECTION('',(0.,-1.,0.));
#18507=DIRECTION('',(-0.996917333733128,0.,0.0784590957278449));
#18508=DIRECTION('center_axis',(-0.996917333733128,0.,0.0784590957278449));
#18509=DIRECTION('ref_axis',(0.0784590957278449,0.,0.996917333733128));
#18510=DIRECTION('',(-0.0784590957278449,0.,-0.996917333733128));
#18511=DIRECTION('',(0.,1.,0.));
#18512=DIRECTION('',(0.0784590957278449,0.,0.996917333733128));
#18513=DIRECTION('center_axis',(0.,1.,0.));
#18514=DIRECTION('ref_axis',(0.996917333733128,0.,-0.0784590957278449));
#18515=DIRECTION('center_axis',(0.,-1.,0.));
#18516=DIRECTION('ref_axis',(0.996917333733128,0.,-0.0784590957278449));
#18517=DIRECTION('',(-0.233445363855906,0.,0.972369920397677));
#18518=DIRECTION('center_axis',(0.,-1.,0.));
#18519=DIRECTION('ref_axis',(0.996917333733128,0.,-0.0784590957278449));
#18520=DIRECTION('',(-0.38268343236509,0.,0.923879532511287));
#18521=DIRECTION('center_axis',(0.,-1.,0.));
#18522=DIRECTION('ref_axis',(0.996917333733128,0.,-0.0784590957278449));
#18523=DIRECTION('',(-0.522498564715949,0.,0.852640164354092));
#18524=DIRECTION('center_axis',(0.,-1.,0.));
#18525=DIRECTION('ref_axis',(0.996917333733128,0.,-0.0784590957278449));
#18526=DIRECTION('',(-0.649448048330184,0.,0.760405965600031));
#18527=DIRECTION('center_axis',(0.,-1.,0.));
#18528=DIRECTION('ref_axis',(0.996917333733128,0.,-0.0784590957278449));
#18529=DIRECTION('',(-0.760405965600031,0.,0.649448048330184));
#18530=DIRECTION('center_axis',(0.,-1.,0.));
#18531=DIRECTION('ref_axis',(0.996917333733128,0.,-0.0784590957278449));
#18532=DIRECTION('',(-0.852640164354092,0.,0.522498564715949));
#18533=DIRECTION('center_axis',(0.,-1.,0.));
#18534=DIRECTION('ref_axis',(0.996917333733128,0.,-0.0784590957278449));
#18535=DIRECTION('',(-0.923879532511287,0.,0.38268343236509));
#18536=DIRECTION('center_axis',(0.,-1.,0.));
#18537=DIRECTION('ref_axis',(0.996917333733128,0.,-0.0784590957278449));
#18538=DIRECTION('',(-0.972369920397677,0.,0.233445363855905));
#18539=DIRECTION('center_axis',(0.,-1.,0.));
#18540=DIRECTION('ref_axis',(0.996917333733128,0.,-0.0784590957278449));
#18541=DIRECTION('',(-0.996917333733128,0.,0.0784590957278448));
#18542=DIRECTION('center_axis',(0.,-1.,0.));
#18543=DIRECTION('ref_axis',(0.996917333733128,0.,-0.0784590957278449));
#18544=DIRECTION('',(-0.996917333733128,0.,-0.0784590957278451));
#18545=DIRECTION('center_axis',(0.,-1.,0.));
#18546=DIRECTION('ref_axis',(0.996917333733128,0.,-0.0784590957278449));
#18547=DIRECTION('',(-0.972369920397677,0.,-0.233445363855906));
#18548=DIRECTION('center_axis',(0.,-1.,0.));
#18549=DIRECTION('ref_axis',(0.996917333733128,0.,-0.0784590957278449));
#18550=DIRECTION('',(-0.923879532511287,0.,-0.38268343236509));
#18551=DIRECTION('center_axis',(0.,-1.,0.));
#18552=DIRECTION('ref_axis',(0.996917333733128,0.,-0.0784590957278449));
#18553=DIRECTION('',(-0.852640164354092,0.,-0.522498564715949));
#18554=DIRECTION('center_axis',(0.,-1.,0.));
#18555=DIRECTION('ref_axis',(0.996917333733128,0.,-0.0784590957278449));
#18556=DIRECTION('',(-0.760405965600031,0.,-0.649448048330184));
#18557=DIRECTION('center_axis',(0.,-1.,0.));
#18558=DIRECTION('ref_axis',(0.996917333733128,0.,-0.0784590957278449));
#18559=DIRECTION('',(-0.649448048330184,0.,-0.760405965600031));
#18560=DIRECTION('center_axis',(0.,-1.,0.));
#18561=DIRECTION('ref_axis',(0.996917333733128,0.,-0.0784590957278449));
#18562=DIRECTION('',(-0.522498564715949,0.,-0.852640164354092));
#18563=DIRECTION('center_axis',(0.,-1.,0.));
#18564=DIRECTION('ref_axis',(0.996917333733128,0.,-0.0784590957278449));
#18565=DIRECTION('',(-0.38268343236509,0.,-0.923879532511287));
#18566=DIRECTION('center_axis',(0.,-1.,0.));
#18567=DIRECTION('ref_axis',(0.996917333733128,0.,-0.0784590957278449));
#18568=DIRECTION('',(-0.233445363855905,0.,-0.972369920397677));
#18569=DIRECTION('center_axis',(0.,-1.,0.));
#18570=DIRECTION('ref_axis',(0.996917333733128,0.,-0.0784590957278449));
#18571=DIRECTION('',(-0.0784590957278448,0.,-0.996917333733128));
#18572=DIRECTION('center_axis',(0.,-1.,0.));
#18573=DIRECTION('ref_axis',(0.996917333733128,0.,-0.0784590957278449));
#18574=DIRECTION('',(0.0784590957278451,0.,-0.996917333733128));
#18575=DIRECTION('center_axis',(0.,-1.,0.));
#18576=DIRECTION('ref_axis',(0.996917333733128,0.,-0.0784590957278449));
#18577=DIRECTION('',(0.233445363855906,0.,-0.972369920397677));
#18578=DIRECTION('center_axis',(0.,-1.,0.));
#18579=DIRECTION('ref_axis',(0.996917333733128,0.,-0.0784590957278449));
#18580=DIRECTION('',(0.38268343236509,0.,-0.923879532511287));
#18581=DIRECTION('center_axis',(0.,-1.,0.));
#18582=DIRECTION('ref_axis',(0.996917333733128,0.,-0.0784590957278449));
#18583=DIRECTION('',(0.522498564715949,0.,-0.852640164354092));
#18584=DIRECTION('center_axis',(0.,-1.,0.));
#18585=DIRECTION('ref_axis',(0.996917333733128,0.,-0.0784590957278449));
#18586=DIRECTION('',(0.649448048330184,0.,-0.760405965600031));
#18587=DIRECTION('center_axis',(0.,-1.,0.));
#18588=DIRECTION('ref_axis',(0.996917333733128,0.,-0.0784590957278449));
#18589=DIRECTION('',(0.760405965600031,0.,-0.649448048330184));
#18590=DIRECTION('center_axis',(0.,-1.,0.));
#18591=DIRECTION('ref_axis',(0.996917333733128,0.,-0.0784590957278449));
#18592=DIRECTION('',(0.852640164354092,0.,-0.522498564715949));
#18593=DIRECTION('center_axis',(0.,-1.,0.));
#18594=DIRECTION('ref_axis',(0.996917333733128,0.,-0.0784590957278449));
#18595=DIRECTION('',(0.923879532511287,0.,-0.38268343236509));
#18596=DIRECTION('center_axis',(0.,-1.,0.));
#18597=DIRECTION('ref_axis',(0.996917333733128,0.,-0.0784590957278449));
#18598=DIRECTION('',(0.972369920397677,0.,-0.233445363855905));
#18599=DIRECTION('center_axis',(0.,-1.,0.));
#18600=DIRECTION('ref_axis',(0.996917333733128,0.,-0.0784590957278449));
#18601=DIRECTION('',(0.996917333733128,0.,-0.0784590957278449));
#18602=DIRECTION('center_axis',(0.,-1.,0.));
#18603=DIRECTION('ref_axis',(0.996917333733128,0.,-0.0784590957278449));
#18604=DIRECTION('',(0.996917333733128,0.,0.078459095727845));
#18605=DIRECTION('center_axis',(0.,-1.,0.));
#18606=DIRECTION('ref_axis',(0.996917333733128,0.,-0.0784590957278449));
#18607=DIRECTION('',(0.972369920397677,0.,0.233445363855906));
#18608=DIRECTION('center_axis',(0.,-1.,0.));
#18609=DIRECTION('ref_axis',(0.996917333733128,0.,-0.0784590957278449));
#18610=DIRECTION('',(0.923879532511287,0.,0.38268343236509));
#18611=DIRECTION('center_axis',(0.,-1.,0.));
#18612=DIRECTION('ref_axis',(0.996917333733128,0.,-0.0784590957278449));
#18613=DIRECTION('',(0.852640164354092,0.,0.522498564715949));
#18614=DIRECTION('center_axis',(0.,-1.,0.));
#18615=DIRECTION('ref_axis',(0.996917333733128,0.,-0.0784590957278449));
#18616=DIRECTION('',(0.760405965600031,0.,0.649448048330184));
#18617=DIRECTION('center_axis',(0.,-1.,0.));
#18618=DIRECTION('ref_axis',(0.996917333733128,0.,-0.0784590957278449));
#18619=DIRECTION('',(0.649448048330184,0.,0.760405965600031));
#18620=DIRECTION('center_axis',(0.,-1.,0.));
#18621=DIRECTION('ref_axis',(0.996917333733128,0.,-0.0784590957278449));
#18622=DIRECTION('',(0.522498564715949,0.,0.852640164354092));
#18623=DIRECTION('center_axis',(0.,-1.,0.));
#18624=DIRECTION('ref_axis',(0.996917333733128,0.,-0.0784590957278449));
#18625=DIRECTION('',(0.38268343236509,0.,0.923879532511287));
#18626=DIRECTION('center_axis',(0.,-1.,0.));
#18627=DIRECTION('ref_axis',(0.996917333733128,0.,-0.0784590957278449));
#18628=DIRECTION('',(0.233445363855905,0.,0.972369920397677));
#18629=DIRECTION('center_axis',(0.,-1.,0.));
#18630=DIRECTION('ref_axis',(0.996917333733128,0.,-0.0784590957278449));
#18631=DIRECTION('',(0.0784590957278449,0.,0.996917333733128));
#18632=DIRECTION('center_axis',(0.,-1.,0.));
#18633=DIRECTION('ref_axis',(0.996917333733128,0.,-0.0784590957278449));
#18634=DIRECTION('',(-0.0784590957278452,0.,0.996917333733128));
#18635=DIRECTION('center_axis',(0.,1.,0.));
#18636=DIRECTION('ref_axis',(0.996917333733128,0.,-0.0784590957278449));
#18637=DIRECTION('center_axis',(0.,1.,0.));
#18638=DIRECTION('ref_axis',(0.078459095727845,0.,0.996917333733128));
#18639=DIRECTION('center_axis',(0.,-1.,0.));
#18640=DIRECTION('ref_axis',(0.996917333733128,0.,-0.0784590957278449));
#18641=DIRECTION('center_axis',(0.,1.,0.));
#18642=DIRECTION('ref_axis',(0.996917333733128,0.,-0.0784590957278449));
#18643=DIRECTION('center_axis',(0.,1.,0.));
#18644=DIRECTION('ref_axis',(0.996917333733128,0.,-0.0784590957278449));
#18645=DIRECTION('',(0.,-1.,0.));
#18646=DIRECTION('center_axis',(0.,-1.,0.));
#18647=DIRECTION('ref_axis',(0.996917333733128,0.,-0.0784590957278449));
#18648=DIRECTION('center_axis',(0.,1.,0.));
#18649=DIRECTION('ref_axis',(0.996917333733128,0.,-0.0784590957278449));
#18650=DIRECTION('',(0.,1.,0.));
#18651=DIRECTION('',(0.,1.,0.));
#18652=DIRECTION('center_axis',(0.996917333733128,0.,0.0784590957278452));
#18653=DIRECTION('ref_axis',(0.0784590957278452,0.,-0.996917333733128));
#18654=DIRECTION('',(0.0784590957278452,0.,-0.996917333733128));
#18655=DIRECTION('center_axis',(0.,1.,0.));
#18656=DIRECTION('ref_axis',(0.996917333733128,0.,-0.0784590957278449));
#18657=DIRECTION('center_axis',(0.,1.,0.));
#18658=DIRECTION('ref_axis',(0.996917333733128,0.,-0.0784590957278449));
#18659=DIRECTION('',(0.,1.,0.));
#18660=DIRECTION('',(0.,1.,0.));
#18661=DIRECTION('center_axis',(0.972369920397677,0.,0.233445363855906));
#18662=DIRECTION('ref_axis',(0.233445363855906,0.,-0.972369920397677));
#18663=DIRECTION('',(0.233445363855906,0.,-0.972369920397677));
#18664=DIRECTION('center_axis',(0.,1.,0.));
#18665=DIRECTION('ref_axis',(0.996917333733128,0.,-0.0784590957278449));
#18666=DIRECTION('center_axis',(0.,1.,0.));
#18667=DIRECTION('ref_axis',(0.996917333733128,0.,-0.0784590957278449));
#18668=DIRECTION('',(0.,1.,0.));
#18669=DIRECTION('',(0.,1.,0.));
#18670=DIRECTION('center_axis',(0.923879532511287,0.,0.38268343236509));
#18671=DIRECTION('ref_axis',(0.38268343236509,0.,-0.923879532511287));
#18672=DIRECTION('',(0.38268343236509,0.,-0.923879532511287));
#18673=DIRECTION('center_axis',(0.,1.,0.));
#18674=DIRECTION('ref_axis',(0.996917333733128,0.,-0.0784590957278449));
#18675=DIRECTION('center_axis',(0.,1.,0.));
#18676=DIRECTION('ref_axis',(0.996917333733128,0.,-0.0784590957278449));
#18677=DIRECTION('',(0.,1.,0.));
#18678=DIRECTION('',(0.,1.,0.));
#18679=DIRECTION('center_axis',(0.852640164354092,0.,0.522498564715949));
#18680=DIRECTION('ref_axis',(0.522498564715949,0.,-0.852640164354092));
#18681=DIRECTION('',(0.522498564715949,0.,-0.852640164354092));
#18682=DIRECTION('center_axis',(0.,1.,0.));
#18683=DIRECTION('ref_axis',(0.996917333733128,0.,-0.0784590957278449));
#18684=DIRECTION('center_axis',(0.,1.,0.));
#18685=DIRECTION('ref_axis',(0.996917333733128,0.,-0.0784590957278449));
#18686=DIRECTION('',(0.,1.,0.));
#18687=DIRECTION('',(0.,1.,0.));
#18688=DIRECTION('center_axis',(0.760405965600031,0.,0.649448048330184));
#18689=DIRECTION('ref_axis',(0.649448048330184,0.,-0.760405965600031));
#18690=DIRECTION('',(0.649448048330184,0.,-0.760405965600031));
#18691=DIRECTION('center_axis',(0.,1.,0.));
#18692=DIRECTION('ref_axis',(0.996917333733128,0.,-0.0784590957278449));
#18693=DIRECTION('center_axis',(0.,1.,0.));
#18694=DIRECTION('ref_axis',(0.996917333733128,0.,-0.0784590957278449));
#18695=DIRECTION('',(0.,1.,0.));
#18696=DIRECTION('',(0.,1.,0.));
#18697=DIRECTION('center_axis',(0.649448048330184,0.,0.760405965600031));
#18698=DIRECTION('ref_axis',(0.760405965600031,0.,-0.649448048330184));
#18699=DIRECTION('',(0.760405965600031,0.,-0.649448048330184));
#18700=DIRECTION('center_axis',(0.,1.,0.));
#18701=DIRECTION('ref_axis',(0.996917333733128,0.,-0.0784590957278449));
#18702=DIRECTION('center_axis',(0.,1.,0.));
#18703=DIRECTION('ref_axis',(0.996917333733128,0.,-0.0784590957278449));
#18704=DIRECTION('',(0.,1.,0.));
#18705=DIRECTION('',(0.,1.,0.));
#18706=DIRECTION('center_axis',(0.522498564715949,0.,0.852640164354092));
#18707=DIRECTION('ref_axis',(0.852640164354092,0.,-0.522498564715949));
#18708=DIRECTION('',(0.852640164354092,0.,-0.522498564715949));
#18709=DIRECTION('center_axis',(0.,1.,0.));
#18710=DIRECTION('ref_axis',(0.996917333733128,0.,-0.0784590957278449));
#18711=DIRECTION('center_axis',(0.,1.,0.));
#18712=DIRECTION('ref_axis',(0.996917333733128,0.,-0.0784590957278449));
#18713=DIRECTION('',(0.,1.,0.));
#18714=DIRECTION('',(0.,1.,0.));
#18715=DIRECTION('center_axis',(0.38268343236509,0.,0.923879532511287));
#18716=DIRECTION('ref_axis',(0.923879532511287,0.,-0.38268343236509));
#18717=DIRECTION('',(0.923879532511287,0.,-0.38268343236509));
#18718=DIRECTION('center_axis',(0.,1.,0.));
#18719=DIRECTION('ref_axis',(0.996917333733128,0.,-0.0784590957278449));
#18720=DIRECTION('center_axis',(0.,1.,0.));
#18721=DIRECTION('ref_axis',(0.996917333733128,0.,-0.0784590957278449));
#18722=DIRECTION('',(0.,1.,0.));
#18723=DIRECTION('',(0.,1.,0.));
#18724=DIRECTION('center_axis',(0.233445363855905,0.,0.972369920397677));
#18725=DIRECTION('ref_axis',(0.972369920397677,0.,-0.233445363855905));
#18726=DIRECTION('',(0.972369920397677,0.,-0.233445363855905));
#18727=DIRECTION('center_axis',(0.,1.,0.));
#18728=DIRECTION('ref_axis',(0.996917333733128,0.,-0.0784590957278449));
#18729=DIRECTION('center_axis',(0.,1.,0.));
#18730=DIRECTION('ref_axis',(0.996917333733128,0.,-0.0784590957278449));
#18731=DIRECTION('',(0.,1.,0.));
#18732=DIRECTION('',(0.,1.,0.));
#18733=DIRECTION('center_axis',(0.0784590957278448,0.,0.996917333733128));
#18734=DIRECTION('ref_axis',(0.996917333733128,0.,-0.0784590957278448));
#18735=DIRECTION('',(0.996917333733128,0.,-0.0784590957278448));
#18736=DIRECTION('center_axis',(0.,1.,0.));
#18737=DIRECTION('ref_axis',(0.996917333733128,0.,-0.0784590957278449));
#18738=DIRECTION('center_axis',(0.,1.,0.));
#18739=DIRECTION('ref_axis',(0.996917333733128,0.,-0.0784590957278449));
#18740=DIRECTION('',(0.,1.,0.));
#18741=DIRECTION('',(0.,1.,0.));
#18742=DIRECTION('center_axis',(-0.0784590957278451,0.,0.996917333733128));
#18743=DIRECTION('ref_axis',(0.996917333733128,0.,0.0784590957278451));
#18744=DIRECTION('',(0.996917333733128,0.,0.0784590957278451));
#18745=DIRECTION('center_axis',(0.,1.,0.));
#18746=DIRECTION('ref_axis',(0.996917333733128,0.,-0.0784590957278449));
#18747=DIRECTION('center_axis',(0.,1.,0.));
#18748=DIRECTION('ref_axis',(0.996917333733128,0.,-0.0784590957278449));
#18749=DIRECTION('',(0.,1.,0.));
#18750=DIRECTION('',(0.,1.,0.));
#18751=DIRECTION('center_axis',(-0.233445363855906,0.,0.972369920397677));
#18752=DIRECTION('ref_axis',(0.972369920397677,0.,0.233445363855906));
#18753=DIRECTION('',(0.972369920397677,0.,0.233445363855906));
#18754=DIRECTION('center_axis',(0.,1.,0.));
#18755=DIRECTION('ref_axis',(0.996917333733128,0.,-0.0784590957278449));
#18756=DIRECTION('center_axis',(0.,1.,0.));
#18757=DIRECTION('ref_axis',(0.996917333733128,0.,-0.0784590957278449));
#18758=DIRECTION('',(0.,1.,0.));
#18759=DIRECTION('',(0.,1.,0.));
#18760=DIRECTION('center_axis',(-0.38268343236509,0.,0.923879532511287));
#18761=DIRECTION('ref_axis',(0.923879532511287,0.,0.38268343236509));
#18762=DIRECTION('',(0.923879532511287,0.,0.38268343236509));
#18763=DIRECTION('center_axis',(0.,1.,0.));
#18764=DIRECTION('ref_axis',(0.996917333733128,0.,-0.0784590957278449));
#18765=DIRECTION('center_axis',(0.,1.,0.));
#18766=DIRECTION('ref_axis',(0.996917333733128,0.,-0.0784590957278449));
#18767=DIRECTION('',(0.,1.,0.));
#18768=DIRECTION('',(0.,1.,0.));
#18769=DIRECTION('center_axis',(-0.522498564715949,0.,0.852640164354092));
#18770=DIRECTION('ref_axis',(0.852640164354092,0.,0.522498564715949));
#18771=DIRECTION('',(0.852640164354092,0.,0.522498564715949));
#18772=DIRECTION('center_axis',(0.,1.,0.));
#18773=DIRECTION('ref_axis',(0.996917333733128,0.,-0.0784590957278449));
#18774=DIRECTION('center_axis',(0.,1.,0.));
#18775=DIRECTION('ref_axis',(0.996917333733128,0.,-0.0784590957278449));
#18776=DIRECTION('',(0.,1.,0.));
#18777=DIRECTION('',(0.,1.,0.));
#18778=DIRECTION('center_axis',(-0.649448048330184,0.,0.760405965600031));
#18779=DIRECTION('ref_axis',(0.760405965600031,0.,0.649448048330184));
#18780=DIRECTION('',(0.760405965600031,0.,0.649448048330184));
#18781=DIRECTION('center_axis',(0.,1.,0.));
#18782=DIRECTION('ref_axis',(0.996917333733128,0.,-0.0784590957278449));
#18783=DIRECTION('center_axis',(0.,1.,0.));
#18784=DIRECTION('ref_axis',(0.996917333733128,0.,-0.0784590957278449));
#18785=DIRECTION('',(0.,1.,0.));
#18786=DIRECTION('',(0.,1.,0.));
#18787=DIRECTION('center_axis',(-0.760405965600031,0.,0.649448048330184));
#18788=DIRECTION('ref_axis',(0.649448048330184,0.,0.760405965600031));
#18789=DIRECTION('',(0.649448048330184,0.,0.760405965600031));
#18790=DIRECTION('center_axis',(0.,1.,0.));
#18791=DIRECTION('ref_axis',(0.996917333733128,0.,-0.0784590957278449));
#18792=DIRECTION('center_axis',(0.,1.,0.));
#18793=DIRECTION('ref_axis',(0.996917333733128,0.,-0.0784590957278449));
#18794=DIRECTION('',(0.,1.,0.));
#18795=DIRECTION('',(0.,1.,0.));
#18796=DIRECTION('center_axis',(-0.852640164354092,0.,0.522498564715949));
#18797=DIRECTION('ref_axis',(0.522498564715949,0.,0.852640164354092));
#18798=DIRECTION('',(0.522498564715949,0.,0.852640164354092));
#18799=DIRECTION('center_axis',(0.,1.,0.));
#18800=DIRECTION('ref_axis',(0.996917333733128,0.,-0.0784590957278449));
#18801=DIRECTION('center_axis',(0.,1.,0.));
#18802=DIRECTION('ref_axis',(0.996917333733128,0.,-0.0784590957278449));
#18803=DIRECTION('',(0.,1.,0.));
#18804=DIRECTION('',(0.,1.,0.));
#18805=DIRECTION('center_axis',(-0.923879532511287,0.,0.38268343236509));
#18806=DIRECTION('ref_axis',(0.38268343236509,0.,0.923879532511287));
#18807=DIRECTION('',(0.38268343236509,0.,0.923879532511287));
#18808=DIRECTION('center_axis',(0.,1.,0.));
#18809=DIRECTION('ref_axis',(0.996917333733128,0.,-0.0784590957278449));
#18810=DIRECTION('center_axis',(0.,1.,0.));
#18811=DIRECTION('ref_axis',(0.996917333733128,0.,-0.0784590957278449));
#18812=DIRECTION('',(0.,1.,0.));
#18813=DIRECTION('',(0.,1.,0.));
#18814=DIRECTION('center_axis',(-0.972369920397677,0.,0.233445363855905));
#18815=DIRECTION('ref_axis',(0.233445363855905,0.,0.972369920397677));
#18816=DIRECTION('',(0.233445363855905,0.,0.972369920397677));
#18817=DIRECTION('center_axis',(0.,1.,0.));
#18818=DIRECTION('ref_axis',(0.996917333733128,0.,-0.0784590957278449));
#18819=DIRECTION('center_axis',(0.,1.,0.));
#18820=DIRECTION('ref_axis',(0.996917333733128,0.,-0.0784590957278449));
#18821=DIRECTION('',(0.,1.,0.));
#18822=DIRECTION('',(0.,1.,0.));
#18823=DIRECTION('center_axis',(-0.996917333733128,0.,0.0784590957278448));
#18824=DIRECTION('ref_axis',(0.0784590957278448,0.,0.996917333733128));
#18825=DIRECTION('',(0.0784590957278448,0.,0.996917333733128));
#18826=DIRECTION('center_axis',(0.,1.,0.));
#18827=DIRECTION('ref_axis',(0.996917333733128,0.,-0.0784590957278449));
#18828=DIRECTION('center_axis',(0.,1.,0.));
#18829=DIRECTION('ref_axis',(0.996917333733128,0.,-0.0784590957278449));
#18830=DIRECTION('',(0.,1.,0.));
#18831=DIRECTION('',(0.,1.,0.));
#18832=DIRECTION('center_axis',(-0.996917333733128,0.,-0.0784590957278451));
#18833=DIRECTION('ref_axis',(-0.0784590957278451,0.,0.996917333733128));
#18834=DIRECTION('',(-0.0784590957278451,0.,0.996917333733128));
#18835=DIRECTION('center_axis',(0.,1.,0.));
#18836=DIRECTION('ref_axis',(0.996917333733128,0.,-0.0784590957278449));
#18837=DIRECTION('center_axis',(0.,1.,0.));
#18838=DIRECTION('ref_axis',(0.996917333733128,0.,-0.0784590957278449));
#18839=DIRECTION('',(0.,1.,0.));
#18840=DIRECTION('',(0.,1.,0.));
#18841=DIRECTION('center_axis',(-0.972369920397677,0.,-0.233445363855906));
#18842=DIRECTION('ref_axis',(-0.233445363855906,0.,0.972369920397677));
#18843=DIRECTION('',(-0.233445363855906,0.,0.972369920397677));
#18844=DIRECTION('center_axis',(0.,1.,0.));
#18845=DIRECTION('ref_axis',(0.996917333733128,0.,-0.0784590957278449));
#18846=DIRECTION('center_axis',(0.,1.,0.));
#18847=DIRECTION('ref_axis',(0.996917333733128,0.,-0.0784590957278449));
#18848=DIRECTION('',(0.,1.,0.));
#18849=DIRECTION('',(0.,1.,0.));
#18850=DIRECTION('center_axis',(-0.923879532511287,0.,-0.38268343236509));
#18851=DIRECTION('ref_axis',(-0.38268343236509,0.,0.923879532511287));
#18852=DIRECTION('',(-0.38268343236509,0.,0.923879532511287));
#18853=DIRECTION('center_axis',(0.,1.,0.));
#18854=DIRECTION('ref_axis',(0.996917333733128,0.,-0.0784590957278449));
#18855=DIRECTION('center_axis',(0.,1.,0.));
#18856=DIRECTION('ref_axis',(0.996917333733128,0.,-0.0784590957278449));
#18857=DIRECTION('',(0.,1.,0.));
#18858=DIRECTION('',(0.,1.,0.));
#18859=DIRECTION('center_axis',(-0.852640164354092,0.,-0.522498564715949));
#18860=DIRECTION('ref_axis',(-0.522498564715949,0.,0.852640164354092));
#18861=DIRECTION('',(-0.522498564715949,0.,0.852640164354092));
#18862=DIRECTION('center_axis',(0.,1.,0.));
#18863=DIRECTION('ref_axis',(0.996917333733128,0.,-0.0784590957278449));
#18864=DIRECTION('center_axis',(0.,1.,0.));
#18865=DIRECTION('ref_axis',(0.996917333733128,0.,-0.0784590957278449));
#18866=DIRECTION('',(0.,1.,0.));
#18867=DIRECTION('',(0.,1.,0.));
#18868=DIRECTION('center_axis',(-0.760405965600031,0.,-0.649448048330184));
#18869=DIRECTION('ref_axis',(-0.649448048330184,0.,0.760405965600031));
#18870=DIRECTION('',(-0.649448048330184,0.,0.760405965600031));
#18871=DIRECTION('center_axis',(0.,1.,0.));
#18872=DIRECTION('ref_axis',(0.996917333733128,0.,-0.0784590957278449));
#18873=DIRECTION('center_axis',(0.,1.,0.));
#18874=DIRECTION('ref_axis',(0.996917333733128,0.,-0.0784590957278449));
#18875=DIRECTION('',(0.,1.,0.));
#18876=DIRECTION('',(0.,1.,0.));
#18877=DIRECTION('center_axis',(-0.649448048330184,0.,-0.760405965600031));
#18878=DIRECTION('ref_axis',(-0.760405965600031,0.,0.649448048330184));
#18879=DIRECTION('',(-0.760405965600031,0.,0.649448048330184));
#18880=DIRECTION('center_axis',(0.,1.,0.));
#18881=DIRECTION('ref_axis',(0.996917333733128,0.,-0.0784590957278449));
#18882=DIRECTION('center_axis',(0.,1.,0.));
#18883=DIRECTION('ref_axis',(0.996917333733128,0.,-0.0784590957278449));
#18884=DIRECTION('',(0.,1.,0.));
#18885=DIRECTION('',(0.,1.,0.));
#18886=DIRECTION('center_axis',(-0.522498564715949,0.,-0.852640164354092));
#18887=DIRECTION('ref_axis',(-0.852640164354092,0.,0.522498564715949));
#18888=DIRECTION('',(-0.852640164354092,0.,0.522498564715949));
#18889=DIRECTION('center_axis',(0.,1.,0.));
#18890=DIRECTION('ref_axis',(0.996917333733128,0.,-0.0784590957278449));
#18891=DIRECTION('center_axis',(0.,1.,0.));
#18892=DIRECTION('ref_axis',(0.996917333733128,0.,-0.0784590957278449));
#18893=DIRECTION('',(0.,1.,0.));
#18894=DIRECTION('',(0.,1.,0.));
#18895=DIRECTION('center_axis',(-0.38268343236509,0.,-0.923879532511287));
#18896=DIRECTION('ref_axis',(-0.923879532511287,0.,0.38268343236509));
#18897=DIRECTION('',(-0.923879532511287,0.,0.38268343236509));
#18898=DIRECTION('center_axis',(0.,1.,0.));
#18899=DIRECTION('ref_axis',(0.996917333733128,0.,-0.0784590957278449));
#18900=DIRECTION('center_axis',(0.,1.,0.));
#18901=DIRECTION('ref_axis',(0.996917333733128,0.,-0.0784590957278449));
#18902=DIRECTION('',(0.,1.,0.));
#18903=DIRECTION('',(0.,1.,0.));
#18904=DIRECTION('center_axis',(-0.233445363855905,0.,-0.972369920397677));
#18905=DIRECTION('ref_axis',(-0.972369920397677,0.,0.233445363855905));
#18906=DIRECTION('',(-0.972369920397677,0.,0.233445363855905));
#18907=DIRECTION('center_axis',(0.,1.,0.));
#18908=DIRECTION('ref_axis',(0.996917333733128,0.,-0.0784590957278449));
#18909=DIRECTION('center_axis',(0.,1.,0.));
#18910=DIRECTION('ref_axis',(0.996917333733128,0.,-0.0784590957278449));
#18911=DIRECTION('',(0.,1.,0.));
#18912=DIRECTION('',(0.,1.,0.));
#18913=DIRECTION('center_axis',(-0.0784590957278449,0.,-0.996917333733128));
#18914=DIRECTION('ref_axis',(-0.996917333733128,0.,0.0784590957278449));
#18915=DIRECTION('',(-0.996917333733128,0.,0.0784590957278449));
#18916=DIRECTION('center_axis',(0.,1.,0.));
#18917=DIRECTION('ref_axis',(0.996917333733128,0.,-0.0784590957278449));
#18918=DIRECTION('center_axis',(0.,1.,0.));
#18919=DIRECTION('ref_axis',(0.996917333733128,0.,-0.0784590957278449));
#18920=DIRECTION('',(0.,1.,0.));
#18921=DIRECTION('',(0.,1.,0.));
#18922=DIRECTION('center_axis',(0.078459095727845,0.,-0.996917333733128));
#18923=DIRECTION('ref_axis',(-0.996917333733128,0.,-0.078459095727845));
#18924=DIRECTION('',(-0.996917333733128,0.,-0.078459095727845));
#18925=DIRECTION('center_axis',(0.,1.,0.));
#18926=DIRECTION('ref_axis',(0.996917333733128,0.,-0.0784590957278449));
#18927=DIRECTION('center_axis',(0.,1.,0.));
#18928=DIRECTION('ref_axis',(0.996917333733128,0.,-0.0784590957278449));
#18929=DIRECTION('',(0.,1.,0.));
#18930=DIRECTION('',(0.,1.,0.));
#18931=DIRECTION('center_axis',(0.233445363855906,0.,-0.972369920397677));
#18932=DIRECTION('ref_axis',(-0.972369920397677,0.,-0.233445363855906));
#18933=DIRECTION('',(-0.972369920397677,0.,-0.233445363855906));
#18934=DIRECTION('center_axis',(0.,1.,0.));
#18935=DIRECTION('ref_axis',(0.996917333733128,0.,-0.0784590957278449));
#18936=DIRECTION('center_axis',(0.,1.,0.));
#18937=DIRECTION('ref_axis',(0.996917333733128,0.,-0.0784590957278449));
#18938=DIRECTION('',(0.,1.,0.));
#18939=DIRECTION('',(0.,1.,0.));
#18940=DIRECTION('center_axis',(0.38268343236509,0.,-0.923879532511287));
#18941=DIRECTION('ref_axis',(-0.923879532511287,0.,-0.38268343236509));
#18942=DIRECTION('',(-0.923879532511287,0.,-0.38268343236509));
#18943=DIRECTION('center_axis',(0.,1.,0.));
#18944=DIRECTION('ref_axis',(0.996917333733128,0.,-0.0784590957278449));
#18945=DIRECTION('center_axis',(0.,1.,0.));
#18946=DIRECTION('ref_axis',(0.996917333733128,0.,-0.0784590957278449));
#18947=DIRECTION('',(0.,1.,0.));
#18948=DIRECTION('',(0.,1.,0.));
#18949=DIRECTION('center_axis',(0.522498564715949,0.,-0.852640164354092));
#18950=DIRECTION('ref_axis',(-0.852640164354092,0.,-0.522498564715949));
#18951=DIRECTION('',(-0.852640164354092,0.,-0.522498564715949));
#18952=DIRECTION('center_axis',(0.,1.,0.));
#18953=DIRECTION('ref_axis',(0.996917333733128,0.,-0.0784590957278449));
#18954=DIRECTION('center_axis',(0.,1.,0.));
#18955=DIRECTION('ref_axis',(0.996917333733128,0.,-0.0784590957278449));
#18956=DIRECTION('',(0.,1.,0.));
#18957=DIRECTION('',(0.,1.,0.));
#18958=DIRECTION('center_axis',(0.649448048330184,0.,-0.760405965600031));
#18959=DIRECTION('ref_axis',(-0.760405965600031,0.,-0.649448048330184));
#18960=DIRECTION('',(-0.760405965600031,0.,-0.649448048330184));
#18961=DIRECTION('center_axis',(0.,1.,0.));
#18962=DIRECTION('ref_axis',(0.996917333733128,0.,-0.0784590957278449));
#18963=DIRECTION('center_axis',(0.,1.,0.));
#18964=DIRECTION('ref_axis',(0.996917333733128,0.,-0.0784590957278449));
#18965=DIRECTION('',(0.,1.,0.));
#18966=DIRECTION('',(0.,1.,0.));
#18967=DIRECTION('center_axis',(0.760405965600031,0.,-0.649448048330184));
#18968=DIRECTION('ref_axis',(-0.649448048330184,0.,-0.760405965600031));
#18969=DIRECTION('',(-0.649448048330184,0.,-0.760405965600031));
#18970=DIRECTION('center_axis',(0.,1.,0.));
#18971=DIRECTION('ref_axis',(0.996917333733128,0.,-0.0784590957278449));
#18972=DIRECTION('center_axis',(0.,1.,0.));
#18973=DIRECTION('ref_axis',(0.996917333733128,0.,-0.0784590957278449));
#18974=DIRECTION('',(0.,1.,0.));
#18975=DIRECTION('',(0.,1.,0.));
#18976=DIRECTION('center_axis',(0.852640164354092,0.,-0.522498564715949));
#18977=DIRECTION('ref_axis',(-0.522498564715949,0.,-0.852640164354092));
#18978=DIRECTION('',(-0.522498564715949,0.,-0.852640164354092));
#18979=DIRECTION('center_axis',(0.,1.,0.));
#18980=DIRECTION('ref_axis',(0.996917333733128,0.,-0.0784590957278449));
#18981=DIRECTION('center_axis',(0.,1.,0.));
#18982=DIRECTION('ref_axis',(0.996917333733128,0.,-0.0784590957278449));
#18983=DIRECTION('',(0.,1.,0.));
#18984=DIRECTION('',(0.,1.,0.));
#18985=DIRECTION('center_axis',(0.923879532511287,0.,-0.38268343236509));
#18986=DIRECTION('ref_axis',(-0.38268343236509,0.,-0.923879532511287));
#18987=DIRECTION('',(-0.38268343236509,0.,-0.923879532511287));
#18988=DIRECTION('center_axis',(0.,1.,0.));
#18989=DIRECTION('ref_axis',(0.996917333733128,0.,-0.0784590957278449));
#18990=DIRECTION('center_axis',(0.,1.,0.));
#18991=DIRECTION('ref_axis',(0.996917333733128,0.,-0.0784590957278449));
#18992=DIRECTION('',(0.,1.,0.));
#18993=DIRECTION('center_axis',(0.972369920397677,0.,-0.233445363855905));
#18994=DIRECTION('ref_axis',(-0.233445363855905,0.,-0.972369920397677));
#18995=DIRECTION('',(-0.233445363855905,0.,-0.972369920397677));
#18996=DIRECTION('',(0.,1.,0.));
#18997=DIRECTION('center_axis',(0.,1.,0.));
#18998=DIRECTION('ref_axis',(0.996917333733128,0.,-0.0784590957278449));
#18999=DIRECTION('center_axis',(0.,1.,0.));
#19000=DIRECTION('ref_axis',(0.996917333733128,0.,-0.0784590957278449));
#19001=DIRECTION('',(0.,1.,0.));
#19002=DIRECTION('',(0.,1.,0.));
#19003=DIRECTION('center_axis',(0.996917333733128,0.,-0.0784590957278449));
#19004=DIRECTION('ref_axis',(-0.0784590957278449,0.,-0.996917333733128));
#19005=DIRECTION('',(-0.0784590957278449,0.,-0.996917333733128));
#19006=DIRECTION('center_axis',(0.,1.,0.));
#19007=DIRECTION('ref_axis',(0.996917333733128,0.,-0.0784590957278449));
#19008=DIRECTION('center_axis',(0.,1.,0.));
#19009=DIRECTION('ref_axis',(0.996917333733128,0.,-0.0784590957278449));
#19010=DIRECTION('center_axis',(0.,1.,0.));
#19011=DIRECTION('ref_axis',(0.996917333733128,0.,-0.0784590957278449));
#19012=DIRECTION('axis',(0.,0.,1.));
#19013=DIRECTION('refdir',(1.,0.,0.));
#19014=DIRECTION('center_axis',(0.866025403784439,0.,-0.5));
#19015=DIRECTION('ref_axis',(0.5,0.,0.866025403784439));
#19016=DIRECTION('',(-0.5,0.,-0.866025403784439));
#19017=DIRECTION('',(0.,-1.,0.));
#19018=DIRECTION('',(0.5,0.,0.866025403784439));
#19019=DIRECTION('',(0.,-1.,0.));
#19020=DIRECTION('center_axis',(1.60246890531964E-16,0.,-1.));
#19021=DIRECTION('ref_axis',(1.,0.,1.60246890531964E-16));
#19022=DIRECTION('',(-1.,0.,-1.60246890531964E-16));
#19023=DIRECTION('',(0.,-1.,0.));
#19024=DIRECTION('',(1.,0.,1.60246890531964E-16));
#19025=DIRECTION('center_axis',(-0.866025403784439,0.,-0.5));
#19026=DIRECTION('ref_axis',(0.5,0.,-0.866025403784439));
#19027=DIRECTION('',(-0.5,0.,0.866025403784439));
#19028=DIRECTION('',(0.,-1.,0.));
#19029=DIRECTION('',(0.5,0.,-0.866025403784439));
#19030=DIRECTION('center_axis',(-0.866025403784439,0.,0.5));
#19031=DIRECTION('ref_axis',(-0.5,0.,-0.866025403784439));
#19032=DIRECTION('',(0.5,0.,0.866025403784439));
#19033=DIRECTION('',(0.,-1.,0.));
#19034=DIRECTION('',(-0.5,0.,-0.866025403784439));
#19035=DIRECTION('center_axis',(-1.60246890531964E-16,0.,1.));
#19036=DIRECTION('ref_axis',(-1.,0.,-1.60246890531964E-16));
#19037=DIRECTION('',(1.,0.,1.60246890531964E-16));
#19038=DIRECTION('',(0.,-1.,0.));
#19039=DIRECTION('',(-1.,0.,-1.60246890531964E-16));
#19040=DIRECTION('center_axis',(0.866025403784439,0.,0.5));
#19041=DIRECTION('ref_axis',(-0.5,0.,0.866025403784439));
#19042=DIRECTION('',(0.5,0.,-0.866025403784439));
#19043=DIRECTION('',(-0.5,0.,0.866025403784439));
#19044=DIRECTION('center_axis',(0.,1.,0.));
#19045=DIRECTION('ref_axis',(1.,0.,0.));
#19046=DIRECTION('center_axis',(0.,-1.,0.));
#19047=DIRECTION('ref_axis',(0.,0.,-1.));
#19048=DIRECTION('center_axis',(0.,1.,0.));
#19049=DIRECTION('ref_axis',(1.,0.,0.));
#19050=DIRECTION('center_axis',(0.,1.,0.));
#19051=DIRECTION('ref_axis',(1.,0.,0.));
#19052=DIRECTION('center_axis',(0.,1.,0.));
#19053=DIRECTION('ref_axis',(0.,0.,1.));
#19054=DIRECTION('center_axis',(0.,-1.,0.));
#19055=DIRECTION('ref_axis',(1.,0.,0.));
#19056=DIRECTION('center_axis',(0.,-1.,0.));
#19057=DIRECTION('ref_axis',(1.,0.,0.));
#19058=DIRECTION('center_axis',(0.,-1.,0.));
#19059=DIRECTION('ref_axis',(1.,0.,0.));
#19060=DIRECTION('',(0.707106781186547,0.707106781186548,8.65956056235493E-17));
#19061=DIRECTION('center_axis',(0.,-1.,0.));
#19062=DIRECTION('ref_axis',(1.,0.,0.));
#19063=DIRECTION('center_axis',(0.,-1.,0.));
#19064=DIRECTION('ref_axis',(1.,0.,0.));
#19065=DIRECTION('',(0.,1.,0.));
#19066=DIRECTION('center_axis',(0.,1.,0.));
#19067=DIRECTION('ref_axis',(1.,0.,0.));
#19068=DIRECTION('center_axis',(0.,-1.,0.));
#19069=DIRECTION('ref_axis',(1.,0.,0.));
#19070=DIRECTION('',(-0.707106781186547,0.707106781186548,-8.65956056235493E-17));
#19071=DIRECTION('center_axis',(0.,-1.,0.));
#19072=DIRECTION('ref_axis',(0.,0.,-1.));
#19073=DIRECTION('center_axis',(0.,-1.,0.));
#19074=DIRECTION('ref_axis',(1.,0.,0.));
#19075=DIRECTION('center_axis',(0.,1.,0.));
#19076=DIRECTION('ref_axis',(1.,0.,0.));
#19077=DIRECTION('center_axis',(0.,1.,0.));
#19078=DIRECTION('ref_axis',(1.,0.,0.));
#19079=DIRECTION('',(-0.447213595499958,0.894427190999916,-5.47678698264203E-17));
#19080=DIRECTION('center_axis',(0.,-1.,0.));
#19081=DIRECTION('ref_axis',(1.,0.,0.));
#19082=DIRECTION('',(0.,1.,0.));
#19083=DIRECTION('',(0.,0.,1.));
#19084=DIRECTION('',(1.,0.,0.));
#19085=DIRECTION('',(0.,0.,1.));
#19086=DIRECTION('',(1.,0.,0.));
#19087=DIRECTION('',(0.,0.,1.));
#19088=DIRECTION('',(1.,0.,0.));
#19089=DIRECTION('',(0.,0.,1.));
#19090=DIRECTION('',(1.,0.,0.));
#19091=DIRECTION('',(0.,0.,1.));
#19092=DIRECTION('',(1.,0.,0.));
#19093=DIRECTION('',(0.,0.,1.));
#19094=DIRECTION('',(1.,0.,0.));
#19095=DIRECTION('',(0.,0.,1.));
#19096=DIRECTION('',(1.,0.,0.));
#19097=DIRECTION('',(0.,0.,1.));
#19098=DIRECTION('',(1.,0.,0.));
#19099=DIRECTION('',(0.,0.,1.));
#19100=DIRECTION('',(1.,0.,0.));
#19101=DIRECTION('',(0.,0.,1.));
#19102=DIRECTION('',(1.,0.,0.));
#19103=DIRECTION('',(0.,0.,1.));
#19104=DIRECTION('',(1.,0.,0.));
#19105=DIRECTION('',(0.,0.,1.));
#19106=DIRECTION('',(1.,0.,0.));
#19107=DIRECTION('',(0.,-1.,2.22044604925031E-16));
#19108=DIRECTION('',(1.,0.,0.));
#19109=DIRECTION('',(0.,-1.,2.22044604925031E-16));
#19110=DIRECTION('',(1.,0.,0.));
#19111=DIRECTION('',(0.,-1.,2.22044604925031E-16));
#19112=DIRECTION('',(1.,0.,0.));
#19113=DIRECTION('',(0.,-1.,2.22044604925031E-16));
#19114=DIRECTION('',(1.,0.,0.));
#19115=DIRECTION('',(0.,-1.,2.22044604925031E-16));
#19116=DIRECTION('',(1.,0.,0.));
#19117=DIRECTION('',(0.,-1.,2.22044604925031E-16));
#19118=DIRECTION('',(1.,0.,0.));
#19119=DIRECTION('',(0.,-1.,2.22044604925031E-16));
#19120=DIRECTION('',(1.,0.,0.));
#19121=DIRECTION('',(0.,-1.,2.22044604925031E-16));
#19122=DIRECTION('',(1.,0.,0.));
#19123=DIRECTION('',(0.,-1.,2.22044604925031E-16));
#19124=DIRECTION('',(1.,0.,0.));
#19125=DIRECTION('',(0.,-1.,2.22044604925031E-16));
#19126=DIRECTION('',(1.,0.,0.));
#19127=DIRECTION('',(0.,-1.,2.22044604925031E-16));
#19128=DIRECTION('',(1.,0.,0.));
#19129=DIRECTION('',(0.,-1.,2.22044604925031E-16));
#19130=DIRECTION('',(1.,0.,0.));
#19131=DIRECTION('',(0.,-1.,2.22044604925031E-16));
#19132=DIRECTION('',(1.,0.,0.));
#19133=DIRECTION('',(0.,-1.,2.22044604925031E-16));
#19134=DIRECTION('',(1.,0.,0.));
#19135=DIRECTION('',(0.,-1.,2.22044604925031E-16));
#19136=DIRECTION('',(1.,0.,0.));
#19137=DIRECTION('',(0.,-1.,2.22044604925031E-16));
#19138=DIRECTION('',(1.,0.,0.));
#19139=DIRECTION('',(0.,-1.,2.22044604925031E-16));
#19140=DIRECTION('',(1.,0.,0.));
#19141=DIRECTION('',(0.,-1.,2.22044604925031E-16));
#19142=DIRECTION('',(1.,0.,0.));
#19143=DIRECTION('',(0.,0.,1.));
#19144=DIRECTION('',(2.22044604925031E-16,-1.,0.));
#19145=DIRECTION('',(0.,0.,1.));
#19146=DIRECTION('',(1.,0.,0.));
#19147=DIRECTION('',(0.,0.,1.));
#19148=DIRECTION('',(1.,0.,0.));
#19149=DIRECTION('',(0.,0.,1.));
#19150=DIRECTION('',(1.,0.,0.));
#19151=DIRECTION('',(0.,0.,1.));
#19152=DIRECTION('',(1.,0.,0.));
#19153=DIRECTION('',(0.,0.,1.));
#19154=DIRECTION('',(1.,0.,0.));
#19155=DIRECTION('',(0.,0.,1.));
#19156=DIRECTION('',(1.,0.,0.));
#19157=DIRECTION('',(0.,-1.,2.22044604925031E-16));
#19158=DIRECTION('',(1.,0.,0.));
#19159=DIRECTION('',(0.,-1.,2.22044604925031E-16));
#19160=DIRECTION('',(1.,0.,0.));
#19161=DIRECTION('',(0.,-1.,2.22044604925031E-16));
#19162=DIRECTION('',(1.,0.,0.));
#19163=DIRECTION('',(0.,-1.,2.22044604925031E-16));
#19164=DIRECTION('',(1.,0.,0.));
#19165=DIRECTION('',(0.,0.,1.));
#19166=DIRECTION('',(1.,0.,0.));
#19167=DIRECTION('',(0.,-1.,2.22044604925031E-16));
#19168=DIRECTION('',(1.,0.,0.));
#19169=DIRECTION('',(0.,-1.,2.22044604925031E-16));
#19170=DIRECTION('',(1.,0.,0.));
#19171=DIRECTION('',(0.,-1.,2.22044604925031E-16));
#19172=DIRECTION('',(1.,0.,0.));
#19173=DIRECTION('',(0.,-1.,2.22044604925031E-16));
#19174=DIRECTION('',(1.,0.,0.));
#19175=DIRECTION('',(0.,-1.,2.22044604925031E-16));
#19176=DIRECTION('',(1.,0.,0.));
#19177=DIRECTION('',(0.,-1.,2.22044604925031E-16));
#19178=DIRECTION('',(1.,0.,0.));
#19179=DIRECTION('',(0.,-1.,2.22044604925031E-16));
#19180=DIRECTION('',(1.,0.,0.));
#19181=DIRECTION('',(0.,-1.,2.22044604925031E-16));
#19182=DIRECTION('',(1.,0.,0.));
#19183=DIRECTION('',(0.,-1.,2.22044604925031E-16));
#19184=DIRECTION('',(1.,0.,0.));
#19185=DIRECTION('',(0.,-1.,2.22044604925031E-16));
#19186=DIRECTION('',(1.,0.,0.));
#19187=DIRECTION('',(0.,0.,1.));
#19188=DIRECTION('',(1.,0.,0.));
#19189=DIRECTION('',(0.,0.,1.));
#19190=DIRECTION('',(1.,0.,0.));
#19191=DIRECTION('',(0.,0.,1.));
#19192=DIRECTION('',(1.,0.,0.));
#19193=DIRECTION('',(0.,0.,1.));
#19194=DIRECTION('',(1.,0.,0.));
#19195=DIRECTION('',(0.,0.,1.));
#19196=DIRECTION('',(1.,0.,0.));
#19197=DIRECTION('',(0.,0.,1.));
#19198=DIRECTION('',(1.,0.,0.));
#19199=DIRECTION('',(0.,0.,1.));
#19200=DIRECTION('',(1.,0.,0.));
#19201=DIRECTION('',(0.,0.,1.));
#19202=DIRECTION('',(2.22044604925031E-16,-1.,0.));
#19203=DIRECTION('',(0.,-1.,2.22044604925031E-16));
#19204=DIRECTION('',(1.,0.,0.));
#19205=DIRECTION('',(0.,-1.,2.22044604925031E-16));
#19206=DIRECTION('',(1.,0.,0.));
#19207=DIRECTION('',(0.,0.,1.));
#19208=DIRECTION('',(1.,0.,0.));
#19209=DIRECTION('',(0.,0.,1.));
#19210=DIRECTION('',(1.,0.,0.));
#19211=DIRECTION('',(0.,0.,1.));
#19212=DIRECTION('',(1.,0.,0.));
#19213=DIRECTION('',(0.,0.,1.));
#19214=DIRECTION('',(1.,0.,0.));
#19215=DIRECTION('',(0.,0.,1.));
#19216=DIRECTION('',(1.,0.,0.));
#19217=DIRECTION('',(0.,0.,1.));
#19218=DIRECTION('',(1.,0.,0.));
#19219=DIRECTION('',(0.,0.,1.));
#19220=DIRECTION('',(2.22044604925031E-16,-1.,0.));
#19221=DIRECTION('',(0.,-1.,2.22044604925031E-16));
#19222=DIRECTION('',(1.,0.,0.));
#19223=DIRECTION('',(0.,-1.,2.22044604925031E-16));
#19224=DIRECTION('',(1.,0.,0.));
#19225=DIRECTION('',(0.,0.,1.));
#19226=DIRECTION('',(1.,0.,0.));
#19227=DIRECTION('',(0.,0.,1.));
#19228=DIRECTION('',(1.,0.,0.));
#19229=DIRECTION('',(0.,0.,1.));
#19230=DIRECTION('',(1.,0.,0.));
#19231=DIRECTION('',(0.,0.,1.));
#19232=DIRECTION('',(1.,0.,0.));
#19233=CARTESIAN_POINT('',(0.,0.,0.));
#19234=CARTESIAN_POINT('',(0.,0.,0.));
#19235=CARTESIAN_POINT('',(0.,0.,0.));
#19236=CARTESIAN_POINT('Origin',(11.1868272016355,8.18682720163547,-1.1));
#19237=CARTESIAN_POINT('',(11.0218272016355,8.18682720163547,-1.));
#19238=CARTESIAN_POINT('Origin',(11.1868272016355,8.18682720163547,-1.));
#19239=CARTESIAN_POINT('',(11.0218272016355,8.18682720163547,0.));
#19240=CARTESIAN_POINT('',(11.0218272016355,8.18682720163547,-1.1));
#19241=CARTESIAN_POINT('Origin',(11.1868272016355,8.18682720163547,0.));
#19242=CARTESIAN_POINT('Origin',(11.1868272016355,9.81317279836453,-1.1));
#19243=CARTESIAN_POINT('',(11.0218272016355,9.81317279836453,-1.));
#19244=CARTESIAN_POINT('Origin',(11.1868272016355,9.81317279836453,-1.));
#19245=CARTESIAN_POINT('',(11.0218272016355,9.81317279836453,0.));
#19246=CARTESIAN_POINT('',(11.0218272016355,9.81317279836453,-1.1));
#19247=CARTESIAN_POINT('Origin',(11.1868272016355,9.81317279836453,0.));
#19248=CARTESIAN_POINT('Origin',(12.8131727983645,9.81317279836453,-1.1));
#19249=CARTESIAN_POINT('',(12.6481727983645,9.81317279836453,-1.));
#19250=CARTESIAN_POINT('Origin',(12.8131727983645,9.81317279836453,-1.));
#19251=CARTESIAN_POINT('',(12.6481727983645,9.81317279836453,0.));
#19252=CARTESIAN_POINT('',(12.6481727983645,9.81317279836453,-1.1));
#19253=CARTESIAN_POINT('Origin',(12.8131727983645,9.81317279836453,0.));
#19254=CARTESIAN_POINT('Origin',(12.8131727983645,8.18682720163547,-1.1));
#19255=CARTESIAN_POINT('',(12.6481727983645,8.18682720163547,-1.));
#19256=CARTESIAN_POINT('Origin',(12.8131727983645,8.18682720163547,-1.));
#19257=CARTESIAN_POINT('',(12.6481727983645,8.18682720163547,0.));
#19258=CARTESIAN_POINT('',(12.6481727983645,8.18682720163547,-1.1));
#19259=CARTESIAN_POINT('Origin',(12.8131727983645,8.18682720163547,0.));
#19260=CARTESIAN_POINT('Origin',(-1.76776695296637,-1.76776695296637,-1.1));
#19261=CARTESIAN_POINT('',(-1.97776695296637,-1.76776695296637,-1.));
#19262=CARTESIAN_POINT('Origin',(-1.76776695296637,-1.76776695296637,-1.));
#19263=CARTESIAN_POINT('',(-1.97776695296637,-1.76776695296637,0.));
#19264=CARTESIAN_POINT('',(-1.97776695296637,-1.76776695296637,-1.1));
#19265=CARTESIAN_POINT('Origin',(-1.76776695296637,-1.76776695296637,0.));
#19266=CARTESIAN_POINT('Origin',(-1.76776695296637,1.76776695296637,-1.1));
#19267=CARTESIAN_POINT('',(-1.97776695296637,1.76776695296637,-1.));
#19268=CARTESIAN_POINT('Origin',(-1.76776695296637,1.76776695296637,-1.));
#19269=CARTESIAN_POINT('',(-1.97776695296637,1.76776695296637,0.));
#19270=CARTESIAN_POINT('',(-1.97776695296637,1.76776695296637,-1.1));
#19271=CARTESIAN_POINT('Origin',(-1.76776695296637,1.76776695296637,0.));
#19272=CARTESIAN_POINT('Origin',(1.76776695296637,1.76776695296637,-1.1));
#19273=CARTESIAN_POINT('',(1.55776695296637,1.76776695296637,-1.));
#19274=CARTESIAN_POINT('Origin',(1.76776695296637,1.76776695296637,-1.));
#19275=CARTESIAN_POINT('',(1.55776695296637,1.76776695296637,0.));
#19276=CARTESIAN_POINT('',(1.55776695296637,1.76776695296637,-1.1));
#19277=CARTESIAN_POINT('Origin',(1.76776695296637,1.76776695296637,0.));
#19278=CARTESIAN_POINT('Origin',(1.76776695296637,-1.76776695296637,-1.1));
#19279=CARTESIAN_POINT('',(1.55776695296637,-1.76776695296637,-1.));
#19280=CARTESIAN_POINT('Origin',(1.76776695296637,-1.76776695296637,-1.));
#19281=CARTESIAN_POINT('',(1.55776695296637,-1.76776695296637,0.));
#19282=CARTESIAN_POINT('',(1.55776695296637,-1.76776695296637,-1.1));
#19283=CARTESIAN_POINT('Origin',(1.76776695296637,-1.76776695296637,0.));
#19284=CARTESIAN_POINT('Origin',(18.5,6.,-1.1));
#19285=CARTESIAN_POINT('',(18.335,6.,-1.));
#19286=CARTESIAN_POINT('Origin',(18.5,6.,-1.));
#19287=CARTESIAN_POINT('',(18.335,6.,0.));
#19288=CARTESIAN_POINT('',(18.335,6.,-1.1));
#19289=CARTESIAN_POINT('Origin',(18.5,6.,0.));
#19290=CARTESIAN_POINT('Origin',(12.5,6.,-1.1));
#19291=CARTESIAN_POINT('',(12.335,6.,-1.));
#19292=CARTESIAN_POINT('Origin',(12.5,6.,-1.));
#19293=CARTESIAN_POINT('',(12.335,6.,0.));
#19294=CARTESIAN_POINT('',(12.335,6.,-1.1));
#19295=CARTESIAN_POINT('Origin',(12.5,6.,0.));
#19296=CARTESIAN_POINT('Origin',(6.5,6.,-1.1));
#19297=CARTESIAN_POINT('',(6.335,6.,-1.));
#19298=CARTESIAN_POINT('Origin',(6.5,6.,-1.));
#19299=CARTESIAN_POINT('',(6.335,6.,0.));
#19300=CARTESIAN_POINT('',(6.335,6.,-1.1));
#19301=CARTESIAN_POINT('Origin',(6.5,6.,0.));
#19302=CARTESIAN_POINT('Origin',(0.5,6.,-1.1));
#19303=CARTESIAN_POINT('',(0.335,6.,-1.));
#19304=CARTESIAN_POINT('Origin',(0.5,6.,-1.));
#19305=CARTESIAN_POINT('',(0.335,6.,0.));
#19306=CARTESIAN_POINT('',(0.335,6.,-1.1));
#19307=CARTESIAN_POINT('Origin',(0.5,6.,0.));
#19308=CARTESIAN_POINT('Origin',(21.,11.5,-1.));
#19309=CARTESIAN_POINT('',(21.,11.5,-1.));
#19310=CARTESIAN_POINT('',(-3.5,11.5,-1.));
#19311=CARTESIAN_POINT('',(21.,11.5,-1.));
#19312=CARTESIAN_POINT('',(-3.5,11.5,0.));
#19313=CARTESIAN_POINT('',(-3.5,11.5,-1.));
#19314=CARTESIAN_POINT('',(21.,11.5,0.));
#19315=CARTESIAN_POINT('',(21.,11.5,0.));
#19316=CARTESIAN_POINT('',(21.,11.5,-1.));
#19317=CARTESIAN_POINT('Origin',(21.,-4.,-1.));
#19318=CARTESIAN_POINT('',(21.,-4.,-1.));
#19319=CARTESIAN_POINT('',(21.,-4.,-1.));
#19320=CARTESIAN_POINT('',(21.,-4.,0.));
#19321=CARTESIAN_POINT('',(21.,-4.,0.));
#19322=CARTESIAN_POINT('',(21.,-4.,-1.));
#19323=CARTESIAN_POINT('Origin',(-3.5,-4.,-1.));
#19324=CARTESIAN_POINT('',(-3.5,-4.,-1.));
#19325=CARTESIAN_POINT('',(-3.5,-4.,-1.));
#19326=CARTESIAN_POINT('',(-3.5,-4.,0.));
#19327=CARTESIAN_POINT('',(-3.5,-4.,0.));
#19328=CARTESIAN_POINT('',(-3.5,-4.,-1.));
#19329=CARTESIAN_POINT('Origin',(-3.5,11.5,-1.));
#19330=CARTESIAN_POINT('',(-3.5,11.5,-1.));
#19331=CARTESIAN_POINT('',(-3.5,11.5,0.));
#19332=CARTESIAN_POINT('Origin',(8.75,3.75,0.));
#19333=CARTESIAN_POINT('Origin',(8.75,3.75,-1.));
#19334=CARTESIAN_POINT('',(0.,0.,0.));
#19335=CARTESIAN_POINT('Origin',(-2.5,11.5,-1.8));
#19336=CARTESIAN_POINT('',(-2.5,11.5,-1.8));
#19337=CARTESIAN_POINT('',(-3.5,11.5,-1.8));
#19338=CARTESIAN_POINT('',(-2.5,11.5,-1.8));
#19339=CARTESIAN_POINT('',(-3.5,11.5,-1.));
#19340=CARTESIAN_POINT('',(-3.5,11.5,-1.8));
#19341=CARTESIAN_POINT('',(-2.5,11.5,-1.));
#19342=CARTESIAN_POINT('',(-2.5,11.5,-1.));
#19343=CARTESIAN_POINT('',(-2.5,11.5,-1.8));
#19344=CARTESIAN_POINT('Origin',(-2.5,-4.,-1.8));
#19345=CARTESIAN_POINT('',(-2.5,-4.,-1.8));
#19346=CARTESIAN_POINT('',(-2.5,-4.,-1.8));
#19347=CARTESIAN_POINT('',(-2.5,-4.,-1.));
#19348=CARTESIAN_POINT('',(-2.5,-4.,-1.));
#19349=CARTESIAN_POINT('',(-2.5,-4.,-1.8));
#19350=CARTESIAN_POINT('Origin',(-3.5,-4.,-1.8));
#19351=CARTESIAN_POINT('',(-3.5,-4.,-1.8));
#19352=CARTESIAN_POINT('',(-3.5,-4.,-1.8));
#19353=CARTESIAN_POINT('',(-3.5,-4.,-1.));
#19354=CARTESIAN_POINT('',(-3.5,-4.,-1.));
#19355=CARTESIAN_POINT('',(-3.5,-4.,-1.8));
#19356=CARTESIAN_POINT('Origin',(-3.5,11.5,-1.8));
#19357=CARTESIAN_POINT('',(-3.5,11.5,-1.8));
#19358=CARTESIAN_POINT('',(-3.5,11.5,-1.));
#19359=CARTESIAN_POINT('Origin',(-3.,3.75,-1.));
#19360=CARTESIAN_POINT('Origin',(-3.,3.75,-1.8));
#19361=CARTESIAN_POINT('',(0.,0.,0.));
#19362=CARTESIAN_POINT('Origin',(21.,11.5,-1.8));
#19363=CARTESIAN_POINT('',(21.,11.5,-1.8));
#19364=CARTESIAN_POINT('',(20.,11.5,-1.8));
#19365=CARTESIAN_POINT('',(21.,11.5,-1.8));
#19366=CARTESIAN_POINT('',(20.,11.5,-1.));
#19367=CARTESIAN_POINT('',(20.,11.5,-1.8));
#19368=CARTESIAN_POINT('',(21.,11.5,-1.));
#19369=CARTESIAN_POINT('',(21.,11.5,-1.));
#19370=CARTESIAN_POINT('',(21.,11.5,-1.8));
#19371=CARTESIAN_POINT('Origin',(21.,-4.,-1.8));
#19372=CARTESIAN_POINT('',(21.,-4.,-1.8));
#19373=CARTESIAN_POINT('',(21.,-4.,-1.8));
#19374=CARTESIAN_POINT('',(21.,-4.,-1.));
#19375=CARTESIAN_POINT('',(21.,-4.,-1.));
#19376=CARTESIAN_POINT('',(21.,-4.,-1.8));
#19377=CARTESIAN_POINT('Origin',(20.,-4.,-1.8));
#19378=CARTESIAN_POINT('',(20.,-4.,-1.8));
#19379=CARTESIAN_POINT('',(20.,-4.,-1.8));
#19380=CARTESIAN_POINT('',(20.,-4.,-1.));
#19381=CARTESIAN_POINT('',(20.,-4.,-1.));
#19382=CARTESIAN_POINT('',(20.,-4.,-1.8));
#19383=CARTESIAN_POINT('Origin',(20.,11.5,-1.8));
#19384=CARTESIAN_POINT('',(20.,11.5,-1.8));
#19385=CARTESIAN_POINT('',(20.,11.5,-1.));
#19386=CARTESIAN_POINT('Origin',(20.5,3.75,-1.));
#19387=CARTESIAN_POINT('Origin',(20.5,3.75,-1.8));
#19388=CARTESIAN_POINT('',(0.,0.,0.));
#19389=CARTESIAN_POINT('Origin',(1.,0.,5.4));
#19390=CARTESIAN_POINT('',(1.27573508221731,0.25,5.4));
#19391=CARTESIAN_POINT('',(1.3,-3.265531974911E-17,5.65));
#19392=CARTESIAN_POINT('Ctrl Pts',(1.27573508221731,0.25,5.4));
#19393=CARTESIAN_POINT('Ctrl Pts',(1.27573508221731,0.25,5.4314757779847));
#19394=CARTESIAN_POINT('Ctrl Pts',(1.27702069216276,0.243693465283356,5.46499438091527));
#19395=CARTESIAN_POINT('Ctrl Pts',(1.28163032180518,0.218156065105989,5.52656503879345));
#19396=CARTESIAN_POINT('Ctrl Pts',(1.28488408143016,0.198929339789528,5.55462405080375));
#19397=CARTESIAN_POINT('Ctrl Pts',(1.29096514782826,0.15462510881767,5.5989282817756));
#19398=CARTESIAN_POINT('Ctrl Pts',(1.29419244883598,0.126565646309025,5.61815583615436));
#19399=CARTESIAN_POINT('Ctrl Pts',(1.29874124129215,0.0649934270822326,
5.6436938378755));
#19400=CARTESIAN_POINT('Ctrl Pts',(1.3,0.0314742746963997,5.65));
#19401=CARTESIAN_POINT('Ctrl Pts',(1.3,6.24500451351651E-17,5.65));
#19402=CARTESIAN_POINT('Ctrl Pts',(1.3,-3.46944695195361E-17,5.65));
#19403=CARTESIAN_POINT('Ctrl Pts',(1.3,-0.0314742746963997,5.65));
#19404=CARTESIAN_POINT('Ctrl Pts',(1.29874124129215,-0.0649934270822321,
5.6436938378755));
#19405=CARTESIAN_POINT('Ctrl Pts',(1.29419244883598,-0.126565646309024,
5.61815583615436));
#19406=CARTESIAN_POINT('Ctrl Pts',(1.29096514782826,-0.15462510881767,5.5989282817756));
#19407=CARTESIAN_POINT('Ctrl Pts',(1.28488408143016,-0.198929339789528,
5.55462405080375));
#19408=CARTESIAN_POINT('Ctrl Pts',(1.28163032180518,-0.218156065105989,
5.52656503879345));
#19409=CARTESIAN_POINT('Ctrl Pts',(1.27702069216276,-0.243693465283357,
5.46499438091527));
#19410=CARTESIAN_POINT('Ctrl Pts',(1.27573508221731,-0.25,5.4314757779847));
#19411=CARTESIAN_POINT('Ctrl Pts',(1.27573508221731,-0.25,5.3685242220153));
#19412=CARTESIAN_POINT('Ctrl Pts',(1.27702069216276,-0.243693465283357,
5.33500561908473));
#19413=CARTESIAN_POINT('Ctrl Pts',(1.28163032180518,-0.218156065105989,
5.27343496120655));
#19414=CARTESIAN_POINT('Ctrl Pts',(1.28488408143016,-0.198929339789528,
5.24537594919626));
#19415=CARTESIAN_POINT('Ctrl Pts',(1.29096514782826,-0.15462510881767,5.2010717182244));
#19416=CARTESIAN_POINT('Ctrl Pts',(1.29419244883598,-0.126565646309025,
5.18184416384564));
#19417=CARTESIAN_POINT('Ctrl Pts',(1.29874124129215,-0.064993427082233,
5.1563061621245));
#19418=CARTESIAN_POINT('Ctrl Pts',(1.3,-0.0314742746963997,5.15));
#19419=CARTESIAN_POINT('Ctrl Pts',(1.3,0.0314742746963996,5.15));
#19420=CARTESIAN_POINT('Ctrl Pts',(1.29874124129215,0.0649934270822325,
5.1563061621245));
#19421=CARTESIAN_POINT('Ctrl Pts',(1.29419244883598,0.126565646309025,5.18184416384564));
#19422=CARTESIAN_POINT('Ctrl Pts',(1.29096514782826,0.15462510881767,5.2010717182244));
#19423=CARTESIAN_POINT('Ctrl Pts',(1.28488408143016,0.198929339789528,5.24537594919626));
#19424=CARTESIAN_POINT('Ctrl Pts',(1.28163032180518,0.21815606510599,5.27343496120655));
#19425=CARTESIAN_POINT('Ctrl Pts',(1.27702069216276,0.243693465283357,5.33500561908473));
#19426=CARTESIAN_POINT('Ctrl Pts',(1.27573508221731,0.25,5.3685242220153));
#19427=CARTESIAN_POINT('Ctrl Pts',(1.27573508221731,0.25,5.4));
#19428=CARTESIAN_POINT('',(2.2,-3.06161699786838E-17,5.65));
#19429=CARTESIAN_POINT('',(1.,-3.06161699786838E-17,5.65));
#19430=CARTESIAN_POINT('',(2.18574929943944,0.25,5.4));
#19431=CARTESIAN_POINT('Ctrl Pts',(2.18574929943944,0.25,5.4));
#19432=CARTESIAN_POINT('Ctrl Pts',(2.18574929943944,0.25,5.36858020459885));
#19433=CARTESIAN_POINT('Ctrl Pts',(2.1864966418499,0.243715184304782,5.33508482465665));
#19434=CARTESIAN_POINT('Ctrl Pts',(2.18919078893771,0.218193365136867,5.27349811248658));
#19435=CARTESIAN_POINT('Ctrl Pts',(2.19109812170418,0.198957838484313,5.24540444789104));
#19436=CARTESIAN_POINT('Ctrl Pts',(2.19467432003671,0.15459567835042,5.20104228775715));
#19437=CARTESIAN_POINT('Ctrl Pts',(2.19657626523243,0.126501958673344,5.18180666233484));
#19438=CARTESIAN_POINT('Ctrl Pts',(2.19925807248334,0.0649150608388436,
5.15628477026131));
#19439=CARTESIAN_POINT('Ctrl Pts',(2.2,0.0314196165789469,5.15));
#19440=CARTESIAN_POINT('Ctrl Pts',(2.2,-0.0314196165789469,5.15));
#19441=CARTESIAN_POINT('Ctrl Pts',(2.19925807248334,-0.0649150608388436,
5.15628477026131));
#19442=CARTESIAN_POINT('Ctrl Pts',(2.19657626523243,-0.126501958673344,
5.18180666233484));
#19443=CARTESIAN_POINT('Ctrl Pts',(2.19467432003671,-0.15459567835042,5.20104228775715));
#19444=CARTESIAN_POINT('Ctrl Pts',(2.19109812170418,-0.198957838484313,
5.24540444789104));
#19445=CARTESIAN_POINT('Ctrl Pts',(2.18919078893771,-0.218193365136867,
5.27349811248658));
#19446=CARTESIAN_POINT('Ctrl Pts',(2.1864966418499,-0.243715184304782,5.33508482465665));
#19447=CARTESIAN_POINT('Ctrl Pts',(2.18574929943944,-0.25,5.36858020459885));
#19448=CARTESIAN_POINT('Ctrl Pts',(2.18574929943944,-0.25,5.43141979540115));
#19449=CARTESIAN_POINT('Ctrl Pts',(2.1864966418499,-0.243715184304782,5.46491517534335));
#19450=CARTESIAN_POINT('Ctrl Pts',(2.18919078893771,-0.218193365136866,
5.52650188751342));
#19451=CARTESIAN_POINT('Ctrl Pts',(2.19109812170418,-0.198957838484313,
5.55459555210896));
#19452=CARTESIAN_POINT('Ctrl Pts',(2.19467432003671,-0.15459567835042,5.59895771224286));
#19453=CARTESIAN_POINT('Ctrl Pts',(2.19657626523243,-0.126501958673343,
5.61819333766516));
#19454=CARTESIAN_POINT('Ctrl Pts',(2.19925807248334,-0.0649150608388435,
5.64371522973869));
#19455=CARTESIAN_POINT('Ctrl Pts',(2.2,-0.0314196165789469,5.65));
#19456=CARTESIAN_POINT('Ctrl Pts',(2.2,-8.32667268468867E-17,5.65));
#19457=CARTESIAN_POINT('Ctrl Pts',(2.2,6.24500451351651E-17,5.65));
#19458=CARTESIAN_POINT('Ctrl Pts',(2.2,0.0314196165789471,5.65));
#19459=CARTESIAN_POINT('Ctrl Pts',(2.19925807248334,0.0649150608388437,
5.64371522973869));
#19460=CARTESIAN_POINT('Ctrl Pts',(2.19657626523243,0.126501958673344,5.61819333766516));
#19461=CARTESIAN_POINT('Ctrl Pts',(2.19467432003671,0.15459567835042,5.59895771224285));
#19462=CARTESIAN_POINT('Ctrl Pts',(2.19109812170418,0.198957838484313,5.55459555210896));
#19463=CARTESIAN_POINT('Ctrl Pts',(2.18919078893771,0.218193365136867,5.52650188751342));
#19464=CARTESIAN_POINT('Ctrl Pts',(2.1864966418499,0.243715184304782,5.46491517534335));
#19465=CARTESIAN_POINT('Ctrl Pts',(2.18574929943944,0.25,5.43141979540115));
#19466=CARTESIAN_POINT('Ctrl Pts',(2.18574929943944,0.25,5.4));
#19467=CARTESIAN_POINT('Origin',(-1.4142135623731,-1.41421356237309,8.5));
#19468=CARTESIAN_POINT('',(-1.5792135623731,-1.41421356237309,8.5));
#19469=CARTESIAN_POINT('Origin',(-1.4142135623731,-1.41421356237309,8.5));
#19470=CARTESIAN_POINT('',(-1.5792135623731,-1.41421356237309,9.2));
#19471=CARTESIAN_POINT('',(-1.5792135623731,-1.41421356237309,8.5));
#19472=CARTESIAN_POINT('Origin',(-1.4142135623731,-1.41421356237309,9.2));
#19473=CARTESIAN_POINT('Origin',(-1.4142135623731,-1.41421356237309,8.5));
#19474=CARTESIAN_POINT('Origin',(-1.41421356237309,1.4142135623731,8.5));
#19475=CARTESIAN_POINT('',(-1.57921356237309,1.4142135623731,8.5));
#19476=CARTESIAN_POINT('Origin',(-1.41421356237309,1.4142135623731,8.5));
#19477=CARTESIAN_POINT('',(-1.57921356237309,1.4142135623731,9.2));
#19478=CARTESIAN_POINT('',(-1.57921356237309,1.4142135623731,8.5));
#19479=CARTESIAN_POINT('Origin',(-1.41421356237309,1.4142135623731,9.2));
#19480=CARTESIAN_POINT('Origin',(-1.41421356237309,1.4142135623731,8.5));
#19481=CARTESIAN_POINT('Origin',(1.4142135623731,1.41421356237309,8.5));
#19482=CARTESIAN_POINT('',(1.2492135623731,1.41421356237309,8.5));
#19483=CARTESIAN_POINT('Origin',(1.4142135623731,1.41421356237309,8.5));
#19484=CARTESIAN_POINT('',(1.2492135623731,1.41421356237309,9.2));
#19485=CARTESIAN_POINT('',(1.2492135623731,1.41421356237309,8.5));
#19486=CARTESIAN_POINT('Origin',(1.4142135623731,1.41421356237309,9.2));
#19487=CARTESIAN_POINT('Origin',(1.4142135623731,1.41421356237309,8.5));
#19488=CARTESIAN_POINT('Origin',(1.41421356237309,-1.4142135623731,8.5));
#19489=CARTESIAN_POINT('',(1.24921356237309,-1.4142135623731,8.5));
#19490=CARTESIAN_POINT('Origin',(1.41421356237309,-1.4142135623731,8.5));
#19491=CARTESIAN_POINT('',(1.24921356237309,-1.4142135623731,9.2));
#19492=CARTESIAN_POINT('',(1.24921356237309,-1.4142135623731,8.5));
#19493=CARTESIAN_POINT('Origin',(1.41421356237309,-1.4142135623731,9.2));
#19494=CARTESIAN_POINT('Origin',(1.41421356237309,-1.4142135623731,8.5));
#19495=CARTESIAN_POINT('Origin',(-1.76776695296637,-1.76776695296637,1.4));
#19496=CARTESIAN_POINT('',(-1.8139637388702,-1.24480341984751,1.4));
#19497=CARTESIAN_POINT('',(-1.24480341984751,-1.81396373887019,1.4));
#19498=CARTESIAN_POINT('Origin',(0.,0.,1.4));
#19499=CARTESIAN_POINT('Origin',(-1.76776695296637,-1.76776695296637,1.4));
#19500=CARTESIAN_POINT('Origin',(-1.76776695296637,-1.76776695296637,0.8));
#19501=CARTESIAN_POINT('',(-1.8139637388702,-1.24480341984751,0.8));
#19502=CARTESIAN_POINT('',(-1.8139637388702,-1.24480341984751,0.8));
#19503=CARTESIAN_POINT('',(-1.24480341984751,-1.81396373887019,0.8));
#19504=CARTESIAN_POINT('Origin',(-1.76776695296637,-1.76776695296637,0.8));
#19505=CARTESIAN_POINT('',(-1.24480341984751,-1.81396373887019,0.8));
#19506=CARTESIAN_POINT('Origin',(-1.76776695296637,1.76776695296637,0.8));
#19507=CARTESIAN_POINT('',(-1.81396373887019,1.24480341984751,1.4));
#19508=CARTESIAN_POINT('',(-1.81396373887019,1.24480341984751,0.8));
#19509=CARTESIAN_POINT('',(-1.81396373887019,1.24480341984751,0.8));
#19510=CARTESIAN_POINT('',(-1.24480341984751,1.81396373887019,1.4));
#19511=CARTESIAN_POINT('Origin',(-1.76776695296637,1.76776695296637,1.4));
#19512=CARTESIAN_POINT('',(-1.24480341984751,1.81396373887019,0.8));
#19513=CARTESIAN_POINT('',(-1.24480341984751,1.81396373887019,0.8));
#19514=CARTESIAN_POINT('Origin',(-1.76776695296637,1.76776695296637,0.8));
#19515=CARTESIAN_POINT('Origin',(-1.76776695296637,1.76776695296637,1.4));
#19516=CARTESIAN_POINT('Origin',(0.,0.,1.4));
#19517=CARTESIAN_POINT('Origin',(1.76776695296637,1.76776695296637,0.8));
#19518=CARTESIAN_POINT('',(1.24480341984751,1.81396373887019,1.4));
#19519=CARTESIAN_POINT('',(1.24480341984751,1.81396373887019,0.8));
#19520=CARTESIAN_POINT('',(1.24480341984751,1.81396373887019,0.8));
#19521=CARTESIAN_POINT('',(1.81396373887019,1.24480341984751,1.4));
#19522=CARTESIAN_POINT('Origin',(1.76776695296637,1.76776695296637,1.4));
#19523=CARTESIAN_POINT('',(1.81396373887019,1.24480341984751,0.8));
#19524=CARTESIAN_POINT('',(1.81396373887019,1.24480341984751,0.8));
#19525=CARTESIAN_POINT('Origin',(1.76776695296637,1.76776695296637,0.8));
#19526=CARTESIAN_POINT('Origin',(1.76776695296637,1.76776695296637,1.4));
#19527=CARTESIAN_POINT('Origin',(0.,0.,1.4));
#19528=CARTESIAN_POINT('Origin',(1.76776695296637,-1.76776695296637,0.8));
#19529=CARTESIAN_POINT('',(1.81396373887019,-1.24480341984751,1.4));
#19530=CARTESIAN_POINT('',(1.81396373887019,-1.24480341984751,0.8));
#19531=CARTESIAN_POINT('',(1.81396373887019,-1.24480341984751,0.8));
#19532=CARTESIAN_POINT('',(1.24480341984751,-1.8139637388702,1.4));
#19533=CARTESIAN_POINT('Origin',(1.76776695296637,-1.76776695296637,1.4));
#19534=CARTESIAN_POINT('',(1.24480341984751,-1.8139637388702,0.8));
#19535=CARTESIAN_POINT('',(1.24480341984751,-1.8139637388702,0.8));
#19536=CARTESIAN_POINT('Origin',(1.76776695296637,-1.76776695296637,0.8));
#19537=CARTESIAN_POINT('Origin',(1.76776695296637,-1.76776695296637,1.4));
#19538=CARTESIAN_POINT('Origin',(0.,0.,1.4));
#19539=CARTESIAN_POINT('Origin',(0.,0.,0.));
#19540=CARTESIAN_POINT('',(-2.2,-2.69422295812418E-16,9.2));
#19541=CARTESIAN_POINT('Origin',(0.,0.,9.2));
#19542=CARTESIAN_POINT('',(-2.2,-2.69422295812418E-16,0.8));
#19543=CARTESIAN_POINT('',(-2.2,-2.69422295812418E-16,0.));
#19544=CARTESIAN_POINT('Origin',(0.,0.,0.8));
#19545=CARTESIAN_POINT('Origin',(0.,0.,0.8));
#19546=CARTESIAN_POINT('Origin',(0.,0.,0.8));
#19547=CARTESIAN_POINT('Origin',(0.,0.,0.8));
#19548=CARTESIAN_POINT('Origin',(0.,0.,0.8));
#19549=CARTESIAN_POINT('Origin',(0.,0.,0.8));
#19550=CARTESIAN_POINT('',(-3.,-3.67394039744206E-16,0.8));
#19551=CARTESIAN_POINT('Origin',(0.,0.,0.8));
#19552=CARTESIAN_POINT('',(-2.04276695296637,-1.76776695296637,0.8));
#19553=CARTESIAN_POINT('Origin',(-1.76776695296637,-1.76776695296637,0.8));
#19554=CARTESIAN_POINT('',(1.49276695296637,1.76776695296637,0.8));
#19555=CARTESIAN_POINT('Origin',(1.76776695296637,1.76776695296637,0.8));
#19556=CARTESIAN_POINT('',(1.49276695296637,-1.76776695296637,0.8));
#19557=CARTESIAN_POINT('Origin',(1.76776695296637,-1.76776695296637,0.8));
#19558=CARTESIAN_POINT('',(-2.04276695296637,1.76776695296637,0.8));
#19559=CARTESIAN_POINT('Origin',(-1.76776695296637,1.76776695296637,0.8));
#19560=CARTESIAN_POINT('Origin',(-1.76776695296637,-1.76776695296637,-0.1));
#19561=CARTESIAN_POINT('',(-2.04276695296637,-1.76776695296637,0.));
#19562=CARTESIAN_POINT('Origin',(-1.76776695296637,-1.76776695296637,0.));
#19563=CARTESIAN_POINT('',(-2.04276695296637,-1.76776695296637,-0.1));
#19564=CARTESIAN_POINT('Origin',(-1.76776695296637,1.76776695296637,-0.1));
#19565=CARTESIAN_POINT('',(-2.04276695296637,1.76776695296637,0.));
#19566=CARTESIAN_POINT('Origin',(-1.76776695296637,1.76776695296637,0.));
#19567=CARTESIAN_POINT('',(-2.04276695296637,1.76776695296637,-0.1));
#19568=CARTESIAN_POINT('Origin',(1.76776695296637,1.76776695296637,-0.1));
#19569=CARTESIAN_POINT('',(1.49276695296637,1.76776695296637,0.));
#19570=CARTESIAN_POINT('Origin',(1.76776695296637,1.76776695296637,0.));
#19571=CARTESIAN_POINT('',(1.49276695296637,1.76776695296637,-0.1));
#19572=CARTESIAN_POINT('Origin',(1.76776695296637,-1.76776695296637,-0.1));
#19573=CARTESIAN_POINT('',(1.49276695296637,-1.76776695296637,0.));
#19574=CARTESIAN_POINT('Origin',(1.76776695296637,-1.76776695296637,0.));
#19575=CARTESIAN_POINT('',(1.49276695296637,-1.76776695296637,-0.1));
#19576=CARTESIAN_POINT('Origin',(0.,0.,6.));
#19577=CARTESIAN_POINT('',(-1.6,-1.95943487863577E-16,6.));
#19578=CARTESIAN_POINT('Origin',(0.,0.,6.));
#19579=CARTESIAN_POINT('',(-1.6,1.95943487863577E-16,9.2));
#19580=CARTESIAN_POINT('',(-1.6,-1.95943487863577E-16,6.));
#19581=CARTESIAN_POINT('Origin',(0.,0.,9.2));
#19582=CARTESIAN_POINT('Origin',(0.,0.,6.));
#19583=CARTESIAN_POINT('',(-1.3,-1.59204083889156E-16,6.));
#19584=CARTESIAN_POINT('Origin',(0.,0.,6.));
#19585=CARTESIAN_POINT('Origin',(0.,0.,0.));
#19586=CARTESIAN_POINT('',(-3.,-3.67394039744206E-16,0.));
#19587=CARTESIAN_POINT('',(-3.,-3.67394039744206E-16,0.));
#19588=CARTESIAN_POINT('Origin',(0.,0.,0.));
#19589=CARTESIAN_POINT('Origin',(0.,0.,0.));
#19590=CARTESIAN_POINT('',(-1.3,-1.59204083889156E-16,0.));
#19591=CARTESIAN_POINT('',(-1.3,-1.59204083889156E-16,0.));
#19592=CARTESIAN_POINT('Origin',(0.,0.,0.));
#19593=CARTESIAN_POINT('Origin',(0.,0.,9.2));
#19594=CARTESIAN_POINT('Origin',(0.,0.,0.));
#19595=CARTESIAN_POINT('',(0.,0.,0.));
#19596=CARTESIAN_POINT('Origin',(0.,0.,7.));
#19597=CARTESIAN_POINT('',(-1.1,-1.34711147906209E-16,8.));
#19598=CARTESIAN_POINT('Origin',(0.,0.,8.));
#19599=CARTESIAN_POINT('',(-1.1,-1.34711147906209E-16,7.));
#19600=CARTESIAN_POINT('',(-1.1,-1.34711147906209E-16,7.));
#19601=CARTESIAN_POINT('Origin',(0.,0.,7.));
#19602=CARTESIAN_POINT('Origin',(0.,0.,7.));
#19603=CARTESIAN_POINT('',(-1.59,-1.94718841064429E-16,8.));
#19604=CARTESIAN_POINT('Origin',(0.,0.,8.));
#19605=CARTESIAN_POINT('',(-1.59,-1.94718841064429E-16,7.));
#19606=CARTESIAN_POINT('',(-1.59,-1.94718841064429E-16,7.));
#19607=CARTESIAN_POINT('Origin',(0.,0.,7.));
#19608=CARTESIAN_POINT('Origin',(0.,0.,8.));
#19609=CARTESIAN_POINT('Origin',(0.,0.,7.));
#19610=CARTESIAN_POINT('',(0.,0.,0.));
#19611=CARTESIAN_POINT('Origin',(-1.4142135623731,-1.41421356237309,9.1));
#19612=CARTESIAN_POINT('',(-1.6301780125076,-1.47733531993816,9.2));
#19613=CARTESIAN_POINT('',(-1.6301780125076,-1.47733531993816,9.6));
#19614=CARTESIAN_POINT('',(-1.6301780125076,-1.47733531993816,9.1));
#19615=CARTESIAN_POINT('',(-1.47733531993816,-1.6301780125076,9.2));
#19616=CARTESIAN_POINT('Origin',(-1.4142135623731,-1.41421356237309,9.2));
#19617=CARTESIAN_POINT('',(-1.47733531993816,-1.6301780125076,9.6));
#19618=CARTESIAN_POINT('',(-1.47733531993816,-1.6301780125076,9.1));
#19619=CARTESIAN_POINT('Origin',(-1.4142135623731,-1.41421356237309,9.6));
#19620=CARTESIAN_POINT('Origin',(-1.41421356237309,1.4142135623731,9.1));
#19621=CARTESIAN_POINT('',(-1.47733531993816,1.6301780125076,9.2));
#19622=CARTESIAN_POINT('',(-1.47733531993816,1.6301780125076,9.6));
#19623=CARTESIAN_POINT('',(-1.47733531993816,1.6301780125076,9.1));
#19624=CARTESIAN_POINT('',(-1.6301780125076,1.47733531993816,9.2));
#19625=CARTESIAN_POINT('Origin',(-1.41421356237309,1.4142135623731,9.2));
#19626=CARTESIAN_POINT('',(-1.6301780125076,1.47733531993816,9.6));
#19627=CARTESIAN_POINT('',(-1.6301780125076,1.47733531993816,9.1));
#19628=CARTESIAN_POINT('Origin',(-1.41421356237309,1.4142135623731,9.6));
#19629=CARTESIAN_POINT('Origin',(1.4142135623731,1.41421356237309,9.1));
#19630=CARTESIAN_POINT('',(1.6301780125076,1.47733531993816,9.2));
#19631=CARTESIAN_POINT('',(1.6301780125076,1.47733531993816,9.6));
#19632=CARTESIAN_POINT('',(1.6301780125076,1.47733531993816,9.1));
#19633=CARTESIAN_POINT('',(1.47733531993816,1.6301780125076,9.2));
#19634=CARTESIAN_POINT('Origin',(1.4142135623731,1.41421356237309,9.2));
#19635=CARTESIAN_POINT('',(1.47733531993816,1.6301780125076,9.6));
#19636=CARTESIAN_POINT('',(1.47733531993816,1.6301780125076,9.1));
#19637=CARTESIAN_POINT('Origin',(1.4142135623731,1.41421356237309,9.6));
#19638=CARTESIAN_POINT('Origin',(1.41421356237309,-1.4142135623731,9.1));
#19639=CARTESIAN_POINT('',(1.47733531993816,-1.6301780125076,9.2));
#19640=CARTESIAN_POINT('',(1.47733531993816,-1.6301780125076,9.6));
#19641=CARTESIAN_POINT('',(1.47733531993816,-1.6301780125076,9.1));
#19642=CARTESIAN_POINT('',(1.6301780125076,-1.47733531993816,9.2));
#19643=CARTESIAN_POINT('Origin',(1.41421356237309,-1.4142135623731,9.2));
#19644=CARTESIAN_POINT('',(1.6301780125076,-1.47733531993816,9.6));
#19645=CARTESIAN_POINT('',(1.6301780125076,-1.47733531993816,9.1));
#19646=CARTESIAN_POINT('Origin',(1.41421356237309,-1.4142135623731,9.6));
#19647=CARTESIAN_POINT('Origin',(0.,0.,9.2));
#19648=CARTESIAN_POINT('Origin',(0.,0.,9.2));
#19649=CARTESIAN_POINT('Origin',(0.,0.,9.2));
#19650=CARTESIAN_POINT('Origin',(0.,0.,9.2));
#19651=CARTESIAN_POINT('Origin',(0.,0.,9.2));
#19652=CARTESIAN_POINT('',(-1.59,-1.94718841064429E-16,9.2));
#19653=CARTESIAN_POINT('Origin',(0.,0.,9.2));
#19654=CARTESIAN_POINT('Origin',(0.,0.,9.2));
#19655=CARTESIAN_POINT('Origin',(0.,0.,9.6));
#19656=CARTESIAN_POINT('Origin',(0.,0.,9.2));
#19657=CARTESIAN_POINT('Origin',(0.,0.,9.6));
#19658=CARTESIAN_POINT('Origin',(0.,0.,9.2));
#19659=CARTESIAN_POINT('Origin',(0.,0.,9.6));
#19660=CARTESIAN_POINT('Origin',(0.,0.,9.2));
#19661=CARTESIAN_POINT('Origin',(0.,0.,9.6));
#19662=CARTESIAN_POINT('Origin',(0.,0.,9.));
#19663=CARTESIAN_POINT('',(-1.59,-1.94718841064429E-16,9.));
#19664=CARTESIAN_POINT('',(-1.59,-1.94718841064429E-16,9.));
#19665=CARTESIAN_POINT('Origin',(0.,0.,9.));
#19666=CARTESIAN_POINT('Origin',(0.,0.,9.));
#19667=CARTESIAN_POINT('',(-1.1,-1.34711147906209E-16,9.));
#19668=CARTESIAN_POINT('Origin',(0.,0.,9.));
#19669=CARTESIAN_POINT('Origin',(0.,0.,9.2));
#19670=CARTESIAN_POINT('',(-1.1,-1.34711147906209E-16,9.6));
#19671=CARTESIAN_POINT('Origin',(0.,0.,9.6));
#19672=CARTESIAN_POINT('',(-1.1,-1.34711147906209E-16,9.2));
#19673=CARTESIAN_POINT('Origin',(0.,0.,9.6));
#19674=CARTESIAN_POINT('',(0.,0.,0.));
#19675=CARTESIAN_POINT('Origin',(11.1868272016355,8.18682720163547,-0.1));
#19676=CARTESIAN_POINT('',(10.9618272016355,8.18682720163547,0.));
#19677=CARTESIAN_POINT('Origin',(11.1868272016355,8.18682720163547,0.));
#19678=CARTESIAN_POINT('',(10.9618272016355,8.18682720163547,0.8));
#19679=CARTESIAN_POINT('',(10.9618272016355,8.18682720163547,-0.1));
#19680=CARTESIAN_POINT('Origin',(11.1868272016355,8.18682720163547,0.8));
#19681=CARTESIAN_POINT('Origin',(11.1868272016355,9.81317279836453,-0.1));
#19682=CARTESIAN_POINT('',(10.9618272016355,9.81317279836453,0.));
#19683=CARTESIAN_POINT('Origin',(11.1868272016355,9.81317279836453,0.));
#19684=CARTESIAN_POINT('',(10.9618272016355,9.81317279836453,0.8));
#19685=CARTESIAN_POINT('',(10.9618272016355,9.81317279836453,-0.1));
#19686=CARTESIAN_POINT('Origin',(11.1868272016355,9.81317279836453,0.8));
#19687=CARTESIAN_POINT('Origin',(12.8131727983645,9.81317279836453,-0.1));
#19688=CARTESIAN_POINT('',(12.5881727983645,9.81317279836453,0.));
#19689=CARTESIAN_POINT('Origin',(12.8131727983645,9.81317279836453,0.));
#19690=CARTESIAN_POINT('',(12.5881727983645,9.81317279836453,0.8));
#19691=CARTESIAN_POINT('',(12.5881727983645,9.81317279836453,-0.1));
#19692=CARTESIAN_POINT('Origin',(12.8131727983645,9.81317279836453,0.8));
#19693=CARTESIAN_POINT('Origin',(12.8131727983645,8.18682720163547,-0.1));
#19694=CARTESIAN_POINT('',(12.5881727983645,8.18682720163547,0.));
#19695=CARTESIAN_POINT('Origin',(12.8131727983645,8.18682720163547,0.));
#19696=CARTESIAN_POINT('',(12.5881727983645,8.18682720163547,0.8));
#19697=CARTESIAN_POINT('',(12.5881727983645,8.18682720163547,-0.1));
#19698=CARTESIAN_POINT('Origin',(12.8131727983645,8.18682720163547,0.8));
#19699=CARTESIAN_POINT('Origin',(12.,9.,0.8));
#19700=CARTESIAN_POINT('',(11.4,9.,15.));
#19701=CARTESIAN_POINT('Origin',(12.,9.,15.));
#19702=CARTESIAN_POINT('',(11.4,9.,0.8));
#19703=CARTESIAN_POINT('',(11.4,9.,0.8));
#19704=CARTESIAN_POINT('Origin',(12.,9.,0.8));
#19705=CARTESIAN_POINT('Origin',(12.,9.,15.));
#19706=CARTESIAN_POINT('Origin',(12.,9.,0.));
#19707=CARTESIAN_POINT('',(10.5,9.,0.8));
#19708=CARTESIAN_POINT('Origin',(12.,9.,0.8));
#19709=CARTESIAN_POINT('',(10.5,9.,0.));
#19710=CARTESIAN_POINT('',(10.5,9.,0.));
#19711=CARTESIAN_POINT('Origin',(12.,9.,0.));
#19712=CARTESIAN_POINT('Origin',(12.,9.,0.8));
#19713=CARTESIAN_POINT('Origin',(12.,9.,0.));
#19714=CARTESIAN_POINT('',(0.,0.,0.));
#19715=CARTESIAN_POINT('Origin',(12.59,9.,12.));
#19716=CARTESIAN_POINT('',(12.59,9.13388427838995,11.9035634923901));
#19717=CARTESIAN_POINT('',(12.59,9.13388427838995,12.0964365076099));
#19718=CARTESIAN_POINT('',(12.59,9.13388427838995,10.9));
#19719=CARTESIAN_POINT('Origin',(12.59,9.,12.));
#19720=CARTESIAN_POINT('Origin',(12.59,9.,12.));
#19721=CARTESIAN_POINT('',(12.59,8.86611572161005,11.9035634923901));
#19722=CARTESIAN_POINT('Ctrl Pts',(12.59,8.86611572161005,11.9035634923901));
#19723=CARTESIAN_POINT('Ctrl Pts',(12.5911984034061,8.87139683465861,11.8962316423768));
#19724=CARTESIAN_POINT('Ctrl Pts',(12.5924406412882,8.87720755102006,11.8894472111884));
#19725=CARTESIAN_POINT('Ctrl Pts',(12.5965106411141,8.89791616804014,11.8687385941683));
#19726=CARTESIAN_POINT('Ctrl Pts',(12.5995440949832,8.91639978640534,11.8560565239921));
#19727=CARTESIAN_POINT('Ctrl Pts',(12.603817074383,8.95702258499573,11.8391843843662));
#19728=CARTESIAN_POINT('Ctrl Pts',(12.605,8.97917005966722,11.835));
#19729=CARTESIAN_POINT('Ctrl Pts',(12.605,9.02082994033278,11.835));
#19730=CARTESIAN_POINT('Ctrl Pts',(12.603817074383,9.04297741500427,11.8391843843662));
#19731=CARTESIAN_POINT('Ctrl Pts',(12.5995440949832,9.08360021359466,11.8560565239921));
#19732=CARTESIAN_POINT('Ctrl Pts',(12.5965106411141,9.10208383195986,11.8687385941683));
#19733=CARTESIAN_POINT('Ctrl Pts',(12.5924406412882,9.12279244897994,11.8894472111884));
#19734=CARTESIAN_POINT('Ctrl Pts',(12.5911984034061,9.12860316534139,11.8962316423768));
#19735=CARTESIAN_POINT('Ctrl Pts',(12.59,9.13388427838995,11.9035634923901));
#19736=CARTESIAN_POINT('',(12.59,8.86611572161005,12.0964365076099));
#19737=CARTESIAN_POINT('Origin',(12.59,9.,12.));
#19738=CARTESIAN_POINT('',(12.605,9.,12.165));
#19739=CARTESIAN_POINT('Ctrl Pts',(12.605,9.,12.165));
#19740=CARTESIAN_POINT('Ctrl Pts',(12.605,8.97917005966722,12.165));
#19741=CARTESIAN_POINT('Ctrl Pts',(12.603817074383,8.95702258499573,12.1608156156338));
#19742=CARTESIAN_POINT('Ctrl Pts',(12.5995440949832,8.91639978640534,12.1439434760079));
#19743=CARTESIAN_POINT('Ctrl Pts',(12.5965106411141,8.89791616804014,12.1312614058317));
#19744=CARTESIAN_POINT('Ctrl Pts',(12.5924406412882,8.87720755102006,12.1105527888116));
#19745=CARTESIAN_POINT('Ctrl Pts',(12.5911984034061,8.87139683465861,12.1037683576232));
#19746=CARTESIAN_POINT('Ctrl Pts',(12.59,8.86611572161005,12.0964365076099));
#19747=CARTESIAN_POINT('',(13.,9.,12.165));
#19748=CARTESIAN_POINT('',(12.59,9.,12.165));
#19749=CARTESIAN_POINT('Origin',(13.,9.,12.));
#19750=CARTESIAN_POINT('Ctrl Pts',(12.59,9.13388427838995,12.0964365076099));
#19751=CARTESIAN_POINT('Ctrl Pts',(12.5911984034061,9.12860316534139,12.1037683576232));
#19752=CARTESIAN_POINT('Ctrl Pts',(12.5924406412882,9.12279244897994,12.1105527888116));
#19753=CARTESIAN_POINT('Ctrl Pts',(12.5965106411141,9.10208383195986,12.1312614058317));
#19754=CARTESIAN_POINT('Ctrl Pts',(12.5995440949832,9.08360021359466,12.1439434760079));
#19755=CARTESIAN_POINT('Ctrl Pts',(12.603817074383,9.04297741500427,12.1608156156338));
#19756=CARTESIAN_POINT('Ctrl Pts',(12.605,9.02082994033278,12.165));
#19757=CARTESIAN_POINT('Ctrl Pts',(12.605,9.,12.165));
#19758=CARTESIAN_POINT('Origin',(12.59,9.,12.));
#19759=CARTESIAN_POINT('',(12.59,8.86611572161005,10.9));
#19760=CARTESIAN_POINT('Origin',(6.,7.9,12.));
#19761=CARTESIAN_POINT('',(6.,8.,13.));
#19762=CARTESIAN_POINT('',(6.,8.5,13.));
#19763=CARTESIAN_POINT('',(6.,7.9,13.));
#19764=CARTESIAN_POINT('',(5.5,8.,12.8660254037844));
#19765=CARTESIAN_POINT('Origin',(6.,8.,12.));
#19766=CARTESIAN_POINT('',(5.5,8.5,12.8660254037844));
#19767=CARTESIAN_POINT('',(5.5,7.9,12.8660254037844));
#19768=CARTESIAN_POINT('',(5.,8.5,12.));
#19769=CARTESIAN_POINT('Origin',(6.,8.5,12.));
#19770=CARTESIAN_POINT('',(5.,9.5,12.));
#19771=CARTESIAN_POINT('',(5.,7.9,12.));
#19772=CARTESIAN_POINT('',(5.5,9.5,12.8660254037844));
#19773=CARTESIAN_POINT('Origin',(6.,9.5,12.));
#19774=CARTESIAN_POINT('',(5.5,10.,12.8660254037844));
#19775=CARTESIAN_POINT('',(5.5,7.9,12.8660254037844));
#19776=CARTESIAN_POINT('',(6.,10.,13.));
#19777=CARTESIAN_POINT('Origin',(6.,10.,12.));
#19778=CARTESIAN_POINT('',(6.,9.5,13.));
#19779=CARTESIAN_POINT('',(6.,7.9,13.));
#19780=CARTESIAN_POINT('',(6.,7.9,13.));
#19781=CARTESIAN_POINT('',(6.,10.,11.));
#19782=CARTESIAN_POINT('Origin',(6.,10.,12.));
#19783=CARTESIAN_POINT('',(6.,9.5,11.));
#19784=CARTESIAN_POINT('',(6.,7.9,11.));
#19785=CARTESIAN_POINT('',(6.,7.9,11.));
#19786=CARTESIAN_POINT('',(5.5,10.,11.1339745962156));
#19787=CARTESIAN_POINT('Origin',(6.,10.,12.));
#19788=CARTESIAN_POINT('',(5.5,9.5,11.1339745962156));
#19789=CARTESIAN_POINT('',(5.5,7.9,11.1339745962156));
#19790=CARTESIAN_POINT('Origin',(6.,9.5,12.));
#19791=CARTESIAN_POINT('',(5.5,8.5,11.1339745962156));
#19792=CARTESIAN_POINT('Origin',(6.,8.5,12.));
#19793=CARTESIAN_POINT('',(5.5,8.,11.1339745962156));
#19794=CARTESIAN_POINT('',(5.5,7.9,11.1339745962156));
#19795=CARTESIAN_POINT('',(6.,8.,11.));
#19796=CARTESIAN_POINT('Origin',(6.,8.,12.));
#19797=CARTESIAN_POINT('',(6.,8.5,11.));
#19798=CARTESIAN_POINT('',(6.,7.9,11.));
#19799=CARTESIAN_POINT('',(6.,7.9,11.));
#19800=CARTESIAN_POINT('Origin',(6.,8.,12.));
#19801=CARTESIAN_POINT('',(6.,7.9,13.));
#19802=CARTESIAN_POINT('Origin',(6.,8.5,12.));
#19803=CARTESIAN_POINT('',(5.5,8.5,13.));
#19804=CARTESIAN_POINT('',(5.5,8.5,11.5));
#19805=CARTESIAN_POINT('',(7.625,8.5,13.));
#19806=CARTESIAN_POINT('',(7.11803398874989,8.5,13.));
#19807=CARTESIAN_POINT('',(7.625,8.5,13.));
#19808=CARTESIAN_POINT('',(7.11803398874989,8.5,11.));
#19809=CARTESIAN_POINT('Origin',(6.,8.5,12.));
#19810=CARTESIAN_POINT('',(7.625,8.5,11.));
#19811=CARTESIAN_POINT('',(5.5,8.5,11.));
#19812=CARTESIAN_POINT('',(7.625,8.5,11.));
#19813=CARTESIAN_POINT('',(5.5,8.5,11.5));
#19814=CARTESIAN_POINT('Origin',(5.5,10.,11.));
#19815=CARTESIAN_POINT('',(5.5,8.,13.));
#19816=CARTESIAN_POINT('',(5.5,8.,11.));
#19817=CARTESIAN_POINT('',(5.5,10.,13.));
#19818=CARTESIAN_POINT('Origin',(5.5,8.,11.));
#19819=CARTESIAN_POINT('',(5.5,8.,13.));
#19820=CARTESIAN_POINT('Origin',(5.5,8.,11.));
#19821=CARTESIAN_POINT('',(13.,8.,11.));
#19822=CARTESIAN_POINT('',(5.5,8.,11.));
#19823=CARTESIAN_POINT('',(13.,8.,13.));
#19824=CARTESIAN_POINT('',(13.,8.,11.));
#19825=CARTESIAN_POINT('',(5.5,8.,13.));
#19826=CARTESIAN_POINT('Origin',(9.25,9.,11.));
#19827=CARTESIAN_POINT('',(5.5,9.5,11.));
#19828=CARTESIAN_POINT('',(7.625,9.5,11.));
#19829=CARTESIAN_POINT('',(5.5,10.,11.));
#19830=CARTESIAN_POINT('',(5.5,10.,11.));
#19831=CARTESIAN_POINT('',(13.,10.,11.));
#19832=CARTESIAN_POINT('Origin',(9.25,9.,11.));
#19833=CARTESIAN_POINT('',(5.5,8.,11.));
#19834=CARTESIAN_POINT('',(5.5,8.,11.));
#19835=CARTESIAN_POINT('',(5.5,10.,11.));
#19836=CARTESIAN_POINT('Origin',(5.5,10.,11.));
#19837=CARTESIAN_POINT('',(5.5,9.5,13.));
#19838=CARTESIAN_POINT('',(5.5,9.5,11.5));
#19839=CARTESIAN_POINT('',(5.5,10.,13.));
#19840=CARTESIAN_POINT('',(5.5,10.,13.));
#19841=CARTESIAN_POINT('',(5.5,10.,11.));
#19842=CARTESIAN_POINT('Origin',(5.5,10.,11.));
#19843=CARTESIAN_POINT('',(5.5,10.,11.));
#19844=CARTESIAN_POINT('',(5.5,9.5,11.5));
#19845=CARTESIAN_POINT('Origin',(13.,10.,11.));
#19846=CARTESIAN_POINT('',(13.,10.,13.));
#19847=CARTESIAN_POINT('',(13.,10.,13.));
#19848=CARTESIAN_POINT('',(13.,10.,11.));
#19849=CARTESIAN_POINT('',(13.,10.,11.));
#19850=CARTESIAN_POINT('',(13.,10.,11.));
#19851=CARTESIAN_POINT('Origin',(13.,10.,11.));
#19852=CARTESIAN_POINT('',(13.,10.,13.));
#19853=CARTESIAN_POINT('Origin',(13.,10.,11.));
#19854=CARTESIAN_POINT('Origin',(9.25,9.,13.));
#19855=CARTESIAN_POINT('',(7.625,9.5,13.));
#19856=CARTESIAN_POINT('Origin',(9.25,9.,13.));
#19857=CARTESIAN_POINT('',(13.,8.,13.));
#19858=CARTESIAN_POINT('',(7.11803398874989,9.5,13.));
#19859=CARTESIAN_POINT('',(7.625,9.5,13.));
#19860=CARTESIAN_POINT('',(7.11803398874989,8.5,13.));
#19861=CARTESIAN_POINT('',(11.395,9.,13.));
#19862=CARTESIAN_POINT('Origin',(12.,9.,13.));
#19863=CARTESIAN_POINT('Origin',(12.,9.,10.9));
#19864=CARTESIAN_POINT('',(11.395,9.,11.));
#19865=CARTESIAN_POINT('Origin',(12.,9.,11.));
#19866=CARTESIAN_POINT('',(11.395,9.,10.9));
#19867=CARTESIAN_POINT('Origin',(6.,8.5,12.));
#19868=CARTESIAN_POINT('',(7.11803398874989,9.5,11.));
#19869=CARTESIAN_POINT('',(7.11803398874989,8.5,11.));
#19870=CARTESIAN_POINT('Origin',(6.,9.5,12.));
#19871=CARTESIAN_POINT('Origin',(6.,9.5,12.));
#19872=CARTESIAN_POINT('',(7.625,9.5,11.));
#19873=CARTESIAN_POINT('Origin',(9.25,9.,13.));
#19874=CARTESIAN_POINT('Origin',(5.5,10.,11.));
#19875=CARTESIAN_POINT('',(5.5,8.,11.));
#19876=CARTESIAN_POINT('Origin',(13.,8.,11.));
#19877=CARTESIAN_POINT('',(13.,8.,11.));
#19878=CARTESIAN_POINT('Origin',(5.5,8.,11.));
#19879=CARTESIAN_POINT('Origin',(9.25,9.,11.));
#19880=CARTESIAN_POINT('',(0.,0.,0.));
#19881=CARTESIAN_POINT('Origin',(6.,6.,12.));
#19882=CARTESIAN_POINT('',(5.795,10.,12.));
#19883=CARTESIAN_POINT('Origin',(6.,10.,12.));
#19884=CARTESIAN_POINT('',(5.795,6.,12.));
#19885=CARTESIAN_POINT('',(5.795,6.,12.));
#19886=CARTESIAN_POINT('Origin',(6.,6.,12.));
#19887=CARTESIAN_POINT('Origin',(6.,6.,12.));
#19888=CARTESIAN_POINT('',(5.,10.,12.));
#19889=CARTESIAN_POINT('Origin',(6.,10.,12.));
#19890=CARTESIAN_POINT('',(5.,6.,12.));
#19891=CARTESIAN_POINT('',(5.,6.,12.));
#19892=CARTESIAN_POINT('Origin',(6.,6.,12.));
#19893=CARTESIAN_POINT('Origin',(6.,10.,12.));
#19894=CARTESIAN_POINT('Origin',(6.,6.,12.));
#19895=CARTESIAN_POINT('',(0.,0.,0.));
#19896=CARTESIAN_POINT('Origin',(6.,10.,12.));
#19897=CARTESIAN_POINT('',(5.,10.3,12.));
#19898=CARTESIAN_POINT('Origin',(6.,10.3,12.));
#19899=CARTESIAN_POINT('',(5.,10.,12.));
#19900=CARTESIAN_POINT('',(5.,10.,12.));
#19901=CARTESIAN_POINT('Origin',(6.,10.,12.));
#19902=CARTESIAN_POINT('Origin',(6.,10.3,12.));
#19903=CARTESIAN_POINT('Origin',(6.,10.,12.));
#19904=CARTESIAN_POINT('',(0.,0.,0.));
#19905=CARTESIAN_POINT('Origin',(6.,4.5,12.));
#19906=CARTESIAN_POINT('',(5.8,7.,12.));
#19907=CARTESIAN_POINT('Origin',(6.,7.,12.));
#19908=CARTESIAN_POINT('',(5.8,4.5,12.));
#19909=CARTESIAN_POINT('',(5.8,4.5,12.));
#19910=CARTESIAN_POINT('Origin',(6.,4.5,12.));
#19911=CARTESIAN_POINT('Origin',(6.,7.,12.));
#19912=CARTESIAN_POINT('Origin',(6.,4.5,12.));
#19913=CARTESIAN_POINT('',(0.,0.,0.));
#19914=CARTESIAN_POINT('Origin',(14.,0.,0.97));
#19915=CARTESIAN_POINT('',(13.625,-4.59242549680257E-17,0.97));
#19916=CARTESIAN_POINT('Origin',(14.,0.,0.97));
#19917=CARTESIAN_POINT('',(13.625,4.59242549680257E-17,1.5));
#19918=CARTESIAN_POINT('',(13.625,-4.59242549680257E-17,0.97));
#19919=CARTESIAN_POINT('Origin',(14.,0.,1.5));
#19920=CARTESIAN_POINT('Origin',(14.,0.,0.97));
#19921=CARTESIAN_POINT('',(13.775,-2.75545529808154E-17,0.97));
#19922=CARTESIAN_POINT('Origin',(14.,0.,0.97));
#19923=CARTESIAN_POINT('Origin',(8.,0.,0.97));
#19924=CARTESIAN_POINT('',(7.625,-4.59242549680257E-17,0.97));
#19925=CARTESIAN_POINT('Origin',(8.,0.,0.97));
#19926=CARTESIAN_POINT('',(7.625,4.59242549680257E-17,1.5));
#19927=CARTESIAN_POINT('',(7.625,-4.59242549680257E-17,0.97));
#19928=CARTESIAN_POINT('Origin',(8.,0.,1.5));
#19929=CARTESIAN_POINT('Origin',(8.,0.,0.97));
#19930=CARTESIAN_POINT('',(7.775,-2.75545529808154E-17,0.97));
#19931=CARTESIAN_POINT('Origin',(8.,0.,0.97));
#19932=CARTESIAN_POINT('Origin',(2.,0.,0.97));
#19933=CARTESIAN_POINT('',(1.625,-4.59242549680257E-17,0.97));
#19934=CARTESIAN_POINT('Origin',(2.,0.,0.97));
#19935=CARTESIAN_POINT('',(1.625,4.59242549680257E-17,1.5));
#19936=CARTESIAN_POINT('',(1.625,-4.59242549680257E-17,0.97));
#19937=CARTESIAN_POINT('Origin',(2.,0.,1.5));
#19938=CARTESIAN_POINT('Origin',(2.,0.,0.97));
#19939=CARTESIAN_POINT('',(1.775,-2.75545529808155E-17,0.97));
#19940=CARTESIAN_POINT('Origin',(2.,0.,0.97));
#19941=CARTESIAN_POINT('Origin',(20.,0.,0.97));
#19942=CARTESIAN_POINT('',(19.625,-4.59242549680257E-17,0.97));
#19943=CARTESIAN_POINT('Origin',(20.,0.,0.97));
#19944=CARTESIAN_POINT('',(19.625,4.59242549680257E-17,1.5));
#19945=CARTESIAN_POINT('',(19.625,-4.59242549680257E-17,0.97));
#19946=CARTESIAN_POINT('Origin',(20.,0.,1.5));
#19947=CARTESIAN_POINT('Origin',(20.,0.,0.97));
#19948=CARTESIAN_POINT('',(19.775,-2.75545529808156E-17,0.97));
#19949=CARTESIAN_POINT('Origin',(20.,0.,0.97));
#19950=CARTESIAN_POINT('Origin',(14.,0.,-0.1));
#19951=CARTESIAN_POINT('',(13.775,-2.75545529808154E-17,0.));
#19952=CARTESIAN_POINT('Origin',(14.,0.,0.));
#19953=CARTESIAN_POINT('',(13.775,-2.75545529808154E-17,-0.1));
#19954=CARTESIAN_POINT('Origin',(8.,0.,-0.1));
#19955=CARTESIAN_POINT('',(7.775,-2.75545529808154E-17,0.));
#19956=CARTESIAN_POINT('Origin',(8.,0.,0.));
#19957=CARTESIAN_POINT('',(7.775,-2.75545529808154E-17,-0.1));
#19958=CARTESIAN_POINT('Origin',(2.,0.,-0.1));
#19959=CARTESIAN_POINT('',(1.775,-2.75545529808155E-17,0.));
#19960=CARTESIAN_POINT('Origin',(2.,0.,0.));
#19961=CARTESIAN_POINT('',(1.775,-2.75545529808155E-17,-0.1));
#19962=CARTESIAN_POINT('Origin',(20.,0.,-0.1));
#19963=CARTESIAN_POINT('',(19.775,-2.75545529808156E-17,0.));
#19964=CARTESIAN_POINT('Origin',(20.,0.,0.));
#19965=CARTESIAN_POINT('',(19.775,-2.75545529808156E-17,-0.1));
#19966=CARTESIAN_POINT('Origin',(0.,-0.53,1.));
#19967=CARTESIAN_POINT('',(0.,-0.53,1.));
#19968=CARTESIAN_POINT('',(0.,-0.75,0.85));
#19969=CARTESIAN_POINT('',(0.,-0.53,1.));
#19970=CARTESIAN_POINT('',(22.,-0.75,0.85));
#19971=CARTESIAN_POINT('',(0.,-0.75,0.85));
#19972=CARTESIAN_POINT('',(22.,-0.53,1.));
#19973=CARTESIAN_POINT('',(22.,-0.53,1.));
#19974=CARTESIAN_POINT('',(0.,-0.53,1.));
#19975=CARTESIAN_POINT('Origin',(0.,-0.53,1.15));
#19976=CARTESIAN_POINT('',(0.,-0.53,1.15));
#19977=CARTESIAN_POINT('',(0.,-0.53,1.15));
#19978=CARTESIAN_POINT('',(22.,-0.53,1.15));
#19979=CARTESIAN_POINT('',(22.,-0.53,1.15));
#19980=CARTESIAN_POINT('',(0.,-0.53,1.15));
#19981=CARTESIAN_POINT('Origin',(0.,-0.75,1.3));
#19982=CARTESIAN_POINT('',(0.,-0.75,1.3));
#19983=CARTESIAN_POINT('',(0.,-0.75,1.3));
#19984=CARTESIAN_POINT('',(22.,-0.75,1.3));
#19985=CARTESIAN_POINT('',(22.,-0.75,1.3));
#19986=CARTESIAN_POINT('',(0.,-0.75,1.3));
#19987=CARTESIAN_POINT('Origin',(0.,-0.75,1.5));
#19988=CARTESIAN_POINT('',(0.,-0.75,1.5));
#19989=CARTESIAN_POINT('',(0.,-0.75,1.5));
#19990=CARTESIAN_POINT('',(22.,-0.75,1.5));
#19991=CARTESIAN_POINT('',(22.,-0.75,1.5));
#19992=CARTESIAN_POINT('',(0.,-0.75,1.5));
#19993=CARTESIAN_POINT('Origin',(0.,0.75,1.5));
#19994=CARTESIAN_POINT('',(0.,0.75,1.5));
#19995=CARTESIAN_POINT('',(0.,0.75,1.5));
#19996=CARTESIAN_POINT('',(22.,0.75,1.5));
#19997=CARTESIAN_POINT('',(22.,0.75,1.5));
#19998=CARTESIAN_POINT('',(0.,0.75,1.5));
#19999=CARTESIAN_POINT('Origin',(0.,0.75,1.3));
#20000=CARTESIAN_POINT('',(0.,0.75,1.3));
#20001=CARTESIAN_POINT('',(0.,0.75,1.3));
#20002=CARTESIAN_POINT('',(22.,0.75,1.3));
#20003=CARTESIAN_POINT('',(22.,0.75,1.3));
#20004=CARTESIAN_POINT('',(0.,0.75,1.3));
#20005=CARTESIAN_POINT('Origin',(0.,0.53,1.15));
#20006=CARTESIAN_POINT('',(0.,0.53,1.15));
#20007=CARTESIAN_POINT('',(0.,0.53,1.15));
#20008=CARTESIAN_POINT('',(22.,0.53,1.15));
#20009=CARTESIAN_POINT('',(22.,0.53,1.15));
#20010=CARTESIAN_POINT('',(0.,0.53,1.15));
#20011=CARTESIAN_POINT('Origin',(0.,0.53,1.));
#20012=CARTESIAN_POINT('',(0.,0.53,1.));
#20013=CARTESIAN_POINT('',(0.,0.53,1.));
#20014=CARTESIAN_POINT('',(22.,0.53,1.));
#20015=CARTESIAN_POINT('',(22.,0.53,1.));
#20016=CARTESIAN_POINT('',(0.,0.53,1.));
#20017=CARTESIAN_POINT('Origin',(0.,0.75,0.85));
#20018=CARTESIAN_POINT('',(0.,0.75,0.85));
#20019=CARTESIAN_POINT('',(0.,0.75,0.85));
#20020=CARTESIAN_POINT('',(22.,0.75,0.85));
#20021=CARTESIAN_POINT('',(22.,0.75,0.85));
#20022=CARTESIAN_POINT('',(0.,0.75,0.85));
#20023=CARTESIAN_POINT('Origin',(0.,0.75,0.));
#20024=CARTESIAN_POINT('',(0.,0.75,0.));
#20025=CARTESIAN_POINT('',(0.,0.75,0.));
#20026=CARTESIAN_POINT('',(22.,0.75,0.));
#20027=CARTESIAN_POINT('',(22.,0.75,0.));
#20028=CARTESIAN_POINT('',(0.,0.75,0.));
#20029=CARTESIAN_POINT('Origin',(0.,-0.75,0.));
#20030=CARTESIAN_POINT('',(0.,-0.75,0.));
#20031=CARTESIAN_POINT('',(0.,-0.75,0.));
#20032=CARTESIAN_POINT('',(22.,-0.75,0.));
#20033=CARTESIAN_POINT('',(22.,-0.75,0.));
#20034=CARTESIAN_POINT('',(0.,-0.75,0.));
#20035=CARTESIAN_POINT('Origin',(0.,-0.75,0.85));
#20036=CARTESIAN_POINT('',(0.,-0.75,0.85));
#20037=CARTESIAN_POINT('',(22.,-0.75,0.85));
#20038=CARTESIAN_POINT('Origin',(22.,0.,0.75));
#20039=CARTESIAN_POINT('Origin',(0.,0.,0.75));
#20040=CARTESIAN_POINT('',(0.,0.,0.));
#20041=CARTESIAN_POINT('',(0.,0.,0.));
#20042=CARTESIAN_POINT('Origin',(0.,0.,0.));
#20043=CARTESIAN_POINT('',(-1.070235,-0.308121667383195,-1.31065986708547E-16));
#20044=CARTESIAN_POINT('',(-1.31065986708547E-16,-0.308121667383195,1.070235));
#20045=CARTESIAN_POINT('Origin',(0.,-0.308121667383195,0.));
#20046=CARTESIAN_POINT('Origin',(0.,-0.308121667383195,0.));
#20047=CARTESIAN_POINT('',(-1.31065986708547E-16,0.308121667383195,1.070235));
#20048=CARTESIAN_POINT('Origin',(-1.34711147906209E-16,0.,1.1));
#20049=CARTESIAN_POINT('',(-1.070235,0.308121667383195,1.31065986708547E-16));
#20050=CARTESIAN_POINT('Origin',(0.,0.308121667383195,0.));
#20051=CARTESIAN_POINT('Origin',(0.,0.308121667383195,0.));
#20052=CARTESIAN_POINT('Origin',(0.,0.,0.));
#20053=CARTESIAN_POINT('',(-1.070235,0.5,-1.31065986708547E-16));
#20054=CARTESIAN_POINT('',(-1.070235,0.,-1.31065986708547E-16));
#20055=CARTESIAN_POINT('Origin',(0.,0.5,0.));
#20056=CARTESIAN_POINT('Origin',(0.,0.,0.));
#20057=CARTESIAN_POINT('',(-0.6,-0.44,-7.34788079488412E-17));
#20058=CARTESIAN_POINT('Origin',(0.,-0.44,0.));
#20059=CARTESIAN_POINT('',(-0.6,0.44,-7.34788079488412E-17));
#20060=CARTESIAN_POINT('',(-0.6,0.,-7.34788079488412E-17));
#20061=CARTESIAN_POINT('Origin',(0.,0.44,0.));
#20062=CARTESIAN_POINT('Origin',(0.,0.47,0.));
#20063=CARTESIAN_POINT('',(-0.66,0.5,-8.08266887437253E-17));
#20064=CARTESIAN_POINT('',(-0.63,0.47,-7.71527483462832E-17));
#20065=CARTESIAN_POINT('Origin',(0.,0.5,0.));
#20066=CARTESIAN_POINT('Origin',(1.070235,0.5,0.));
#20067=CARTESIAN_POINT('Origin',(0.,0.,0.));
#20068=CARTESIAN_POINT('',(-1.070235,-0.5,-1.31065986708547E-16));
#20069=CARTESIAN_POINT('Origin',(0.,-0.5,0.));
#20070=CARTESIAN_POINT('',(-1.070235,0.,-1.31065986708547E-16));
#20071=CARTESIAN_POINT('Origin',(0.66,-0.5,0.));
#20072=CARTESIAN_POINT('',(-0.66,-0.5,-8.08266887437253E-17));
#20073=CARTESIAN_POINT('Origin',(0.,-0.5,0.));
#20074=CARTESIAN_POINT('Origin',(0.,-0.47,0.));
#20075=CARTESIAN_POINT('',(-0.63,-0.47,-7.71527483462832E-17));
#20076=CARTESIAN_POINT('',(0.,0.,0.));
#20077=CARTESIAN_POINT('Origin',(0.,0.,0.));
#20078=CARTESIAN_POINT('',(-1.129765,0.308121667383195,-1.38356309103871E-16));
#20079=CARTESIAN_POINT('',(-1.38356309103871E-16,0.308121667383195,1.129765));
#20080=CARTESIAN_POINT('Origin',(0.,0.308121667383195,0.));
#20081=CARTESIAN_POINT('Origin',(0.,0.308121667383195,0.));
#20082=CARTESIAN_POINT('',(-1.38356309103871E-16,-0.308121667383195,1.129765));
#20083=CARTESIAN_POINT('Origin',(-1.34711147906209E-16,0.,1.1));
#20084=CARTESIAN_POINT('',(-1.129765,-0.308121667383195,1.38356309103871E-16));
#20085=CARTESIAN_POINT('Origin',(0.,-0.308121667383195,0.));
#20086=CARTESIAN_POINT('Origin',(0.,-0.308121667383195,0.));
#20087=CARTESIAN_POINT('Origin',(0.,0.,0.));
#20088=CARTESIAN_POINT('',(-1.129765,-0.5,-1.38356309103871E-16));
#20089=CARTESIAN_POINT('Origin',(0.,-0.5,0.));
#20090=CARTESIAN_POINT('',(-1.129765,0.,-1.38356309103871E-16));
#20091=CARTESIAN_POINT('Origin',(1.54,0.5,0.));
#20092=CARTESIAN_POINT('',(-1.54,0.5,-1.88595607068692E-16));
#20093=CARTESIAN_POINT('Origin',(0.,0.5,0.));
#20094=CARTESIAN_POINT('',(-1.129765,0.5,-1.38356309103871E-16));
#20095=CARTESIAN_POINT('Origin',(0.,0.5,0.));
#20096=CARTESIAN_POINT('Origin',(0.,0.47,0.));
#20097=CARTESIAN_POINT('',(-1.6,0.44,-1.95943487863577E-16));
#20098=CARTESIAN_POINT('Origin',(0.,0.44,0.));
#20099=CARTESIAN_POINT('',(-1.57,0.47,-1.92269547466134E-16));
#20100=CARTESIAN_POINT('Origin',(0.,0.,0.));
#20101=CARTESIAN_POINT('',(-1.6,-0.44,-1.95943487863577E-16));
#20102=CARTESIAN_POINT('Origin',(0.,-0.44,0.));
#20103=CARTESIAN_POINT('',(-1.6,0.,-1.95943487863577E-16));
#20104=CARTESIAN_POINT('Origin',(0.,-0.47,0.));
#20105=CARTESIAN_POINT('',(-1.54,-0.5,-1.88595607068692E-16));
#20106=CARTESIAN_POINT('Origin',(0.,-0.5,0.));
#20107=CARTESIAN_POINT('',(-1.57,-0.47,-1.92269547466134E-16));
#20108=CARTESIAN_POINT('Origin',(1.129765,-0.5,0.));
#20109=CARTESIAN_POINT('Origin',(0.,0.,0.));
#20110=CARTESIAN_POINT('',(-1.129765,0.,-1.38356309103871E-16));
#20111=CARTESIAN_POINT('',(0.,0.,0.));
#20112=CARTESIAN_POINT('Origin',(1.1,0.,0.));
#20113=CARTESIAN_POINT('',(1.1,-2.23201749654651E-33,0.29765));
#20114=CARTESIAN_POINT('',(1.1,-2.23201749654651E-33,-0.29765));
#20115=CARTESIAN_POINT('Origin',(1.1,0.,0.));
#20116=CARTESIAN_POINT('Origin',(0.685838782044607,0.,-0.860014630714833));
#20117=CARTESIAN_POINT('',(0.918550922801216,-5.31350540756609E-33,-0.674432891191581));
#20118=CARTESIAN_POINT('',(0.453126641287998,8.49470414473068E-34,-1.04559637023808));
#20119=CARTESIAN_POINT('Origin',(0.685838782044607,0.,-0.860014630714833));
#20120=CARTESIAN_POINT('Origin',(-0.244773027351946,0.,-1.07242070340001));
#20121=CARTESIAN_POINT('',(0.0454142657089739,-2.23201749654651E-33,-1.1386540593921));
#20122=CARTESIAN_POINT('',(-0.534960320412865,-2.23201749654651E-33,-1.00618734740791));
#20123=CARTESIAN_POINT('Origin',(-0.244773027351946,0.,-1.07242070340001));
#20124=CARTESIAN_POINT('Origin',(-0.991065754692661,0.,-0.477272113029314));
#20125=CARTESIAN_POINT('',(-0.86192025974432,8.49470414473067E-34,-0.745445496560469));
#20126=CARTESIAN_POINT('',(-1.120211249641,-5.31350540756609E-33,-0.209098729498159));
#20127=CARTESIAN_POINT('Origin',(-0.991065754692661,0.,-0.477272113029314));
#20128=CARTESIAN_POINT('Origin',(-0.991065754692661,0.,0.477272113029314));
#20129=CARTESIAN_POINT('',(-1.120211249641,-2.23201749654651E-33,0.209098729498159));
#20130=CARTESIAN_POINT('',(-0.86192025974432,-2.23201749654651E-33,0.745445496560469));
#20131=CARTESIAN_POINT('Origin',(-0.991065754692661,0.,0.477272113029314));
#20132=CARTESIAN_POINT('Origin',(-0.244773027351946,0.,1.07242070340001));
#20133=CARTESIAN_POINT('',(-0.534960320412866,-2.23201749654651E-33,1.00618734740791));
#20134=CARTESIAN_POINT('',(0.0454142657089737,-2.23201749654651E-33,1.1386540593921));
#20135=CARTESIAN_POINT('Origin',(-0.244773027351946,0.,1.07242070340001));
#20136=CARTESIAN_POINT('Origin',(0.685838782044607,0.,0.860014630714833));
#20137=CARTESIAN_POINT('',(0.453126641287998,-2.23201749654651E-33,1.04559637023808));
#20138=CARTESIAN_POINT('',(0.918550922801216,-2.23201749654651E-33,0.674432891191581));
#20139=CARTESIAN_POINT('Origin',(0.685838782044607,0.,0.860014630714833));
#20140=CARTESIAN_POINT('',(0.,0.,0.));
#20141=CARTESIAN_POINT('Origin',(0.685838782044607,0.,0.860014630714833));
#20142=CARTESIAN_POINT('',(0.413083465285518,-0.05953,0.993751811093549));
#20143=CARTESIAN_POINT('',(0.876916659919095,-0.05953,0.623857181492959));
#20144=CARTESIAN_POINT('Ctrl Pts',(0.413083465285518,-0.05953,0.993751811093549));
#20145=CARTESIAN_POINT('Ctrl Pts',(0.419070565453383,-0.0925528133349865,
0.991263089003441));
#20146=CARTESIAN_POINT('Ctrl Pts',(0.430199341854858,-0.124911173756694,
0.986608710139579));
#20147=CARTESIAN_POINT('Ctrl Pts',(0.457978755888596,-0.177924977804098,
0.973971221090534));
#20148=CARTESIAN_POINT('Ctrl Pts',(0.473077587363685,-0.199697230012983,
0.966820759530997));
#20149=CARTESIAN_POINT('Ctrl Pts',(0.507057380724533,-0.237895043532788,
0.949440676105255));
#20150=CARTESIAN_POINT('Ctrl Pts',(0.525933334162555,-0.254319232363049,
0.939198248544428));
#20151=CARTESIAN_POINT('Ctrl Pts',(0.564362943424238,-0.28018331644634,
0.916597376014514));
#20152=CARTESIAN_POINT('Ctrl Pts',(0.585840553788742,-0.29104845371857,
0.903141581680914));
#20153=CARTESIAN_POINT('Ctrl Pts',(0.629305439856167,-0.30527573347708,
0.873412008702649));
#20154=CARTESIAN_POINT('Ctrl Pts',(0.651278921914856,-0.308638795020976,
0.857118508332695));
#20155=CARTESIAN_POINT('Ctrl Pts',(0.690705563850638,-0.308638795020976,
0.825676810575914));
#20156=CARTESIAN_POINT('Ctrl Pts',(0.711480111898423,-0.30527573347708,
0.807879894508811));
#20157=CARTESIAN_POINT('Ctrl Pts',(0.750136149454208,-0.29104845371857,
0.772120216227122));
#20158=CARTESIAN_POINT('Ctrl Pts',(0.768033796848072,-0.28018331644634,
0.754175290318038));
#20159=CARTESIAN_POINT('Ctrl Pts',(0.798619410861634,-0.254319232363049,
0.721738358858166));
#20160=CARTESIAN_POINT('Ctrl Pts',(0.812805334167529,-0.237895043532788,
0.705614819529209));
#20161=CARTESIAN_POINT('Ctrl Pts',(0.837310877969633,-0.199697230012983,
0.676354402927683));
#20162=CARTESIAN_POINT('Ctrl Pts',(0.847641868610495,-0.177924977804098,
0.663225258065736));
#20163=CARTESIAN_POINT('Ctrl Pts',(0.866144010579847,-0.124911173756694,
0.638954437806245));
#20164=CARTESIAN_POINT('Ctrl Pts',(0.873158080166742,-0.0925528133349865,
0.62914037979579));
#20165=CARTESIAN_POINT('Ctrl Pts',(0.876916659919095,-0.05953,0.623857181492959));
#20166=CARTESIAN_POINT('',(0.437601487681057,-0.05953,1.03511272300331));
#20167=CARTESIAN_POINT('Origin',(0.685838782044607,-0.05953,0.860014630714833));
#20168=CARTESIAN_POINT('',(0.911784794170997,-0.05953,0.656964154625313));
#20169=CARTESIAN_POINT('Ctrl Pts',(0.911784794170998,-0.0595300000000001,
0.656964154625312));
#20170=CARTESIAN_POINT('Ctrl Pts',(0.909827729890942,-0.0762225747374255,
0.659680317203144));
#20171=CARTESIAN_POINT('Ctrl Pts',(0.907004864562642,-0.0928409665394228,
0.663576540841106));
#20172=CARTESIAN_POINT('Ctrl Pts',(0.895234408667242,-0.144299303100741,
0.679480524217551));
#20173=CARTESIAN_POINT('Ctrl Pts',(0.882797231409153,-0.177024326825049,
0.695831250979106));
#20174=CARTESIAN_POINT('Ctrl Pts',(0.854332839576145,-0.227269801620064,
0.73042219438957));
#20175=CARTESIAN_POINT('Ctrl Pts',(0.834863020612702,-0.251265615809407,
0.752807465209441));
#20176=CARTESIAN_POINT('Ctrl Pts',(0.800439809856111,-0.279889827963178,
0.789147407129766));
#20177=CARTESIAN_POINT('Ctrl Pts',(0.781998747691871,-0.290879136862659,
0.80756613568454));
#20178=CARTESIAN_POINT('Ctrl Pts',(0.742239891936898,-0.305251990234487,
0.844254137480382));
#20179=CARTESIAN_POINT('Ctrl Pts',(0.720906778729541,-0.308638795020976,
0.862505527716294));
#20180=CARTESIAN_POINT('Ctrl Pts',(0.680463863683392,-0.308638795020976,
0.894757676234429));
#20181=CARTESIAN_POINT('Ctrl Pts',(0.657923009631182,-0.305251990234488,
0.91149460735272));
#20182=CARTESIAN_POINT('Ctrl Pts',(0.613307674922609,-0.290879136862659,
0.942092777160053));
#20183=CARTESIAN_POINT('Ctrl Pts',(0.591247219971725,-0.279889827963178,
0.955972930713954));
#20184=CARTESIAN_POINT('Ctrl Pts',(0.548158511259202,-0.251265615809407,
0.981446681891443));
#20185=CARTESIAN_POINT('Ctrl Pts',(0.522002043615455,-0.227269801620063,
0.995447160474328));
#20186=CARTESIAN_POINT('Ctrl Pts',(0.481944444320713,-0.177024326825049,
1.01550068154148));
#20187=CARTESIAN_POINT('Ctrl Pts',(0.463236132117164,-0.14429930310074,
1.0239876538093));
#20188=CARTESIAN_POINT('Ctrl Pts',(0.445111721969657,-0.0928409665394226,
1.03192403056628));
#20189=CARTESIAN_POINT('Ctrl Pts',(0.440685038163619,-0.0762225747374254,
1.03380912944435));
#20190=CARTESIAN_POINT('Ctrl Pts',(0.437601487681056,-0.05953,1.03511272300331));
#20191=CARTESIAN_POINT('Origin',(0.685838782044607,-0.05953,0.860014630714833));
#20192=CARTESIAN_POINT('Origin',(0.,-0.208355,0.));
#20193=CARTESIAN_POINT('',(0.0548532617164168,-0.05953,1.12247250791415));
#20194=CARTESIAN_POINT('Origin',(0.,-0.05953,0.));
#20195=CARTESIAN_POINT('',(-0.536443649899848,-0.05953,0.987512846410683));
#20196=CARTESIAN_POINT('Ctrl Pts',(0.0548532617164173,-0.0595300000000001,
1.12247250791414));
#20197=CARTESIAN_POINT('Ctrl Pts',(0.05150947068137,-0.0762225747374254,
1.12263591311425));
#20198=CARTESIAN_POINT('Ctrl Pts',(0.0467032526342597,-0.0928409665394227,
1.12285816383385));
#20199=CARTESIAN_POINT('Ctrl Pts',(0.0269302585198975,-0.144299303100741,
1.12357162229597));
#20200=CARTESIAN_POINT('Ctrl Pts',(0.006392292392153,-0.177024326825049,
1.12404235695137));
#20201=CARTESIAN_POINT('Ctrl Pts',(-0.0383992541984087,-0.227269801620063,
1.12335509974011));
#20202=CARTESIAN_POINT('Ctrl Pts',(-0.0680399972366993,-0.251265615809407,
1.12208997038458));
#20203=CARTESIAN_POINT('Ctrl Pts',(-0.117914228755037,-0.279889827963178,
1.1178344036749));
#20204=CARTESIAN_POINT('Ctrl Pts',(-0.14381238480104,-0.290879136862659,
1.11490049012186));
#20205=CARTESIAN_POINT('Ctrl Pts',(-0.19728546073067,-0.305251990234488,
1.10669035995599));
#20206=CARTESIAN_POINT('Ctrl Pts',(-0.224855950742601,-0.308638795020976,
1.10139101611326));
#20207=CARTESIAN_POINT('Ctrl Pts',(-0.275287440920027,-0.308638795020976,
1.0898803575765));
#20208=CARTESIAN_POINT('Ctrl Pts',(-0.302426893214945,-0.305251990234488,
1.08269251410343));
#20209=CARTESIAN_POINT('Ctrl Pts',(-0.35416671187353,-0.290879136862659,
1.06688848765783));
#20210=CARTESIAN_POINT('Ctrl Pts',(-0.3787731215897,-0.279889827963178,
1.05829506364875));
#20211=CARTESIAN_POINT('Ctrl Pts',(-0.425554672694338,-0.251265615809407,
1.04048957871266));
#20212=CARTESIAN_POINT('Ctrl Pts',(-0.452808978448581,-0.227269801620063,
1.02876878445619));
#20213=CARTESIAN_POINT('Ctrl Pts',(-0.493462957200432,-0.177024326825049,
1.0099536580922));
#20214=CARTESIAN_POINT('Ctrl Pts',(-0.511762781179148,-0.14429930310074,
1.00061845128527));
#20215=CARTESIAN_POINT('Ctrl Pts',(-0.529268075276157,-0.0928409665394226,
0.991396466802468));
#20216=CARTESIAN_POINT('Ctrl Pts',(-0.533501897135713,-0.0762225747374254,
0.989110885965947));
#20217=CARTESIAN_POINT('Ctrl Pts',(-0.536443649899848,-0.0595300000000001,
0.987512846410683));
#20218=CARTESIAN_POINT('',(-0.843383895613249,-0.05953,0.742736168477219));
#20219=CARTESIAN_POINT('Origin',(0.,-0.05953,0.));
#20220=CARTESIAN_POINT('',(-1.10653577764992,-0.05953,0.196295654879792));
#20221=CARTESIAN_POINT('Ctrl Pts',(-0.843383895613249,-0.0595300000000001,
0.742736168477219));
#20222=CARTESIAN_POINT('Ctrl Pts',(-0.84559647055299,-0.0762225747374255,
0.740223768851062));
#20223=CARTESIAN_POINT('Ctrl Pts',(-0.848766861100456,-0.0928409665394227,
0.736604687327351));
#20224=CARTESIAN_POINT('Ctrl Pts',(-0.861652925570091,-0.144299303100741,
0.721590372101268));
#20225=CARTESIAN_POINT('Ctrl Pts',(-0.87482617317514,-0.177024326825049,
0.705826641853758));
#20226=CARTESIAN_POINT('Ctrl Pts',(-0.902215926359523,-0.227269801620063,
0.670378702718353));
#20227=CARTESIAN_POINT('Ctrl Pts',(-0.919707509403859,-0.251265615809407,
0.646415841396062));
#20228=CARTESIAN_POINT('Ctrl Pts',(-0.947476448101718,-0.279889827963178,
0.604769294586516));
#20229=CARTESIAN_POINT('Ctrl Pts',(-0.961329858300736,-0.290879136862659,
0.582692035672022));
#20230=CARTESIAN_POINT('Ctrl Pts',(-0.988250837578047,-0.305251990234488,
0.535766169015486));
#20231=CARTESIAN_POINT('Ctrl Pts',(-1.00129756308006,-0.308638795020976,
0.510906605094603));
#20232=CARTESIAN_POINT('Ctrl Pts',(-1.02374168767024,-0.308638795020976,
0.46430090015576));
#20233=CARTESIAN_POINT('Ctrl Pts',(-1.03504317708586,-0.305251990234488,
0.438600874831839));
#20234=CARTESIAN_POINT('Ctrl Pts',(-1.05494634094458,-0.290879136862659,
0.388295406390235));
#20235=CARTESIAN_POINT('Ctrl Pts',(-1.06356957703048,-0.279889827963178,
0.363699428370917));
#20236=CARTESIAN_POINT('Ctrl Pts',(-1.0788165083757,-0.251265615809407,
0.316022600643821));
#20237=CARTESIAN_POINT('Ctrl Pts',(-1.08664560412098,-0.227269801620063,
0.287406530683752));
#20238=CARTESIAN_POINT('Ctrl Pts',(-1.09728268713976,-0.177024326825049,
0.243890930799337));
#20239=CARTESIAN_POINT('Ctrl Pts',(-1.10139388218929,-0.144299303100741,
0.22376314604679));
#20240=CARTESIAN_POINT('Ctrl Pts',(-1.10509821673782,-0.0928409665394227,
0.204327142733961));
#20241=CARTESIAN_POINT('Ctrl Pts',(-1.10595102243643,-0.0762225747374254,
0.199591971170104));
#20242=CARTESIAN_POINT('Ctrl Pts',(-1.10653577764992,-0.0595300000000001,
0.196295654879792));
#20243=CARTESIAN_POINT('',(-1.123812,-0.05953,1.37627276864339E-16));
#20244=CARTESIAN_POINT('Origin',(0.,-0.05953,0.));
#20245=CARTESIAN_POINT('',(-1.123812,-0.35718,1.37627276864339E-16));
#20246=CARTESIAN_POINT('',(-1.123812,-0.208355,1.37627276864339E-16));
#20247=CARTESIAN_POINT('Origin',(0.,-0.35718,0.));
#20248=CARTESIAN_POINT('',(-1.10653577764992,-0.05953,-0.196295654879793));
#20249=CARTESIAN_POINT('Origin',(0.,-0.05953,0.));
#20250=CARTESIAN_POINT('',(-0.843383895613249,-0.05953,-0.742736168477219));
#20251=CARTESIAN_POINT('Ctrl Pts',(-1.10653577764992,-0.0595300000000001,
-0.196295654879792));
#20252=CARTESIAN_POINT('Ctrl Pts',(-1.10595102243643,-0.0762225747374255,
-0.199591971170104));
#20253=CARTESIAN_POINT('Ctrl Pts',(-1.10509821673782,-0.0928409665394228,
-0.204327142733962));
#20254=CARTESIAN_POINT('Ctrl Pts',(-1.10139388218929,-0.144299303100741,
-0.22376314604679));
#20255=CARTESIAN_POINT('Ctrl Pts',(-1.09728268713976,-0.177024326825049,
-0.243890930799338));
#20256=CARTESIAN_POINT('Ctrl Pts',(-1.08664560412098,-0.227269801620063,
-0.287406530683753));
#20257=CARTESIAN_POINT('Ctrl Pts',(-1.0788165083757,-0.251265615809407,
-0.316022600643821));
#20258=CARTESIAN_POINT('Ctrl Pts',(-1.06356957703048,-0.279889827963178,
-0.363699428370918));
#20259=CARTESIAN_POINT('Ctrl Pts',(-1.05494634094458,-0.290879136862659,
-0.388295406390235));
#20260=CARTESIAN_POINT('Ctrl Pts',(-1.03504317708586,-0.305251990234488,
-0.438600874831839));
#20261=CARTESIAN_POINT('Ctrl Pts',(-1.02374168767024,-0.308638795020976,
-0.46430090015576));
#20262=CARTESIAN_POINT('Ctrl Pts',(-1.00129756308006,-0.308638795020976,
-0.510906605094603));
#20263=CARTESIAN_POINT('Ctrl Pts',(-0.988250837578047,-0.305251990234488,
-0.535766169015486));
#20264=CARTESIAN_POINT('Ctrl Pts',(-0.961329858300736,-0.290879136862659,
-0.582692035672022));
#20265=CARTESIAN_POINT('Ctrl Pts',(-0.947476448101718,-0.279889827963178,
-0.604769294586516));
#20266=CARTESIAN_POINT('Ctrl Pts',(-0.919707509403859,-0.251265615809407,
-0.646415841396062));
#20267=CARTESIAN_POINT('Ctrl Pts',(-0.902215926359523,-0.227269801620064,
-0.670378702718353));
#20268=CARTESIAN_POINT('Ctrl Pts',(-0.87482617317514,-0.177024326825049,
-0.705826641853758));
#20269=CARTESIAN_POINT('Ctrl Pts',(-0.861652925570091,-0.144299303100741,
-0.721590372101268));
#20270=CARTESIAN_POINT('Ctrl Pts',(-0.848766861100456,-0.0928409665394229,
-0.736604687327351));
#20271=CARTESIAN_POINT('Ctrl Pts',(-0.84559647055299,-0.0762225747374255,
-0.740223768851063));
#20272=CARTESIAN_POINT('Ctrl Pts',(-0.843383895613249,-0.0595300000000001,
-0.742736168477219));
#20273=CARTESIAN_POINT('',(-0.536443649899847,-0.05953,-0.987512846410683));
#20274=CARTESIAN_POINT('Origin',(0.,-0.05953,0.));
#20275=CARTESIAN_POINT('',(0.0548532617164172,-0.05953,-1.12247250791415));
#20276=CARTESIAN_POINT('Ctrl Pts',(-0.536443649899848,-0.0595300000000001,
-0.987512846410683));
#20277=CARTESIAN_POINT('Ctrl Pts',(-0.533501897135712,-0.0762225747374254,
-0.989110885965947));
#20278=CARTESIAN_POINT('Ctrl Pts',(-0.529268075276156,-0.0928409665394227,
-0.991396466802469));
#20279=CARTESIAN_POINT('Ctrl Pts',(-0.511762781179147,-0.144299303100741,
-1.00061845128527));
#20280=CARTESIAN_POINT('Ctrl Pts',(-0.493462957200432,-0.177024326825049,
-1.0099536580922));
#20281=CARTESIAN_POINT('Ctrl Pts',(-0.45280897844858,-0.227269801620063,
-1.02876878445619));
#20282=CARTESIAN_POINT('Ctrl Pts',(-0.425554672694337,-0.251265615809407,
-1.04048957871266));
#20283=CARTESIAN_POINT('Ctrl Pts',(-0.3787731215897,-0.279889827963178,
-1.05829506364875));
#20284=CARTESIAN_POINT('Ctrl Pts',(-0.354166711873529,-0.290879136862659,
-1.06688848765783));
#20285=CARTESIAN_POINT('Ctrl Pts',(-0.302426893214944,-0.305251990234488,
-1.08269251410343));
#20286=CARTESIAN_POINT('Ctrl Pts',(-0.275287440920027,-0.308638795020976,
-1.0898803575765));
#20287=CARTESIAN_POINT('Ctrl Pts',(-0.224855950742601,-0.308638795020976,
-1.10139101611326));
#20288=CARTESIAN_POINT('Ctrl Pts',(-0.19728546073067,-0.305251990234488,
-1.10669035995599));
#20289=CARTESIAN_POINT('Ctrl Pts',(-0.143812384801039,-0.290879136862659,
-1.11490049012186));
#20290=CARTESIAN_POINT('Ctrl Pts',(-0.117914228755037,-0.279889827963178,
-1.1178344036749));
#20291=CARTESIAN_POINT('Ctrl Pts',(-0.0680399972366989,-0.251265615809407,
-1.12208997038458));
#20292=CARTESIAN_POINT('Ctrl Pts',(-0.0383992541984084,-0.227269801620063,
-1.12335509974011));
#20293=CARTESIAN_POINT('Ctrl Pts',(0.00639229239215326,-0.177024326825049,
-1.12404235695137));
#20294=CARTESIAN_POINT('Ctrl Pts',(0.0269302585198977,-0.144299303100741,
-1.12357162229597));
#20295=CARTESIAN_POINT('Ctrl Pts',(0.04670325263426,-0.0928409665394228,
-1.12285816383385));
#20296=CARTESIAN_POINT('Ctrl Pts',(0.0515094706813703,-0.0762225747374255,
-1.12263591311425));
#20297=CARTESIAN_POINT('Ctrl Pts',(0.0548532617164176,-0.0595300000000001,
-1.12247250791414));
#20298=CARTESIAN_POINT('',(0.437601487681057,-0.05953,-1.03511272300331));
#20299=CARTESIAN_POINT('Origin',(0.,-0.05953,0.));
#20300=CARTESIAN_POINT('',(0.911784794170997,-0.05953,-0.656964154625313));
#20301=CARTESIAN_POINT('Ctrl Pts',(0.437601487681056,-0.0595300000000001,
-1.03511272300331));
#20302=CARTESIAN_POINT('Ctrl Pts',(0.440685038163619,-0.0762225747374255,
-1.03380912944435));
#20303=CARTESIAN_POINT('Ctrl Pts',(0.445111721969657,-0.0928409665394228,
-1.03192403056628));
#20304=CARTESIAN_POINT('Ctrl Pts',(0.463236132117164,-0.144299303100741,
-1.0239876538093));
#20305=CARTESIAN_POINT('Ctrl Pts',(0.481944444320713,-0.177024326825049,
-1.01550068154148));
#20306=CARTESIAN_POINT('Ctrl Pts',(0.522002043615455,-0.227269801620064,
-0.995447160474328));
#20307=CARTESIAN_POINT('Ctrl Pts',(0.548158511259203,-0.251265615809407,
-0.981446681891443));
#20308=CARTESIAN_POINT('Ctrl Pts',(0.591247219971725,-0.279889827963178,
-0.955972930713954));
#20309=CARTESIAN_POINT('Ctrl Pts',(0.613307674922609,-0.290879136862659,
-0.942092777160053));
#20310=CARTESIAN_POINT('Ctrl Pts',(0.657923009631182,-0.305251990234487,
-0.91149460735272));
#20311=CARTESIAN_POINT('Ctrl Pts',(0.680463863683393,-0.308638795020976,
-0.894757676234429));
#20312=CARTESIAN_POINT('Ctrl Pts',(0.720906778729542,-0.308638795020976,
-0.862505527716294));
#20313=CARTESIAN_POINT('Ctrl Pts',(0.742239891936899,-0.305251990234488,
-0.844254137480381));
#20314=CARTESIAN_POINT('Ctrl Pts',(0.781998747691872,-0.290879136862659,
-0.80756613568454));
#20315=CARTESIAN_POINT('Ctrl Pts',(0.800439809856112,-0.279889827963178,
-0.789147407129765));
#20316=CARTESIAN_POINT('Ctrl Pts',(0.834863020612702,-0.251265615809407,
-0.752807465209441));
#20317=CARTESIAN_POINT('Ctrl Pts',(0.854332839576145,-0.227269801620064,
-0.73042219438957));
#20318=CARTESIAN_POINT('Ctrl Pts',(0.882797231409153,-0.177024326825049,
-0.695831250979106));
#20319=CARTESIAN_POINT('Ctrl Pts',(0.895234408667242,-0.144299303100741,
-0.679480524217551));
#20320=CARTESIAN_POINT('Ctrl Pts',(0.907004864562642,-0.0928409665394228,
-0.663576540841106));
#20321=CARTESIAN_POINT('Ctrl Pts',(0.909827729890942,-0.0762225747374256,
-0.659680317203144));
#20322=CARTESIAN_POINT('Ctrl Pts',(0.911784794170998,-0.0595300000000001,
-0.656964154625312));
#20323=CARTESIAN_POINT('',(1.08212377959455,-0.05953,-0.303251606722892));
#20324=CARTESIAN_POINT('Origin',(0.,-0.05953,0.));
#20325=CARTESIAN_POINT('',(1.08212377959455,-0.05953,0.303251606722892));
#20326=CARTESIAN_POINT('Ctrl Pts',(1.08212377959455,-0.0595300000000001,
-0.303251606722892));
#20327=CARTESIAN_POINT('Ctrl Pts',(1.0830271513892,-0.0762225747374255,
-0.300028012588062));
#20328=CARTESIAN_POINT('Ctrl Pts',(1.08431331394788,-0.0928409665394228,
-0.2953917518996));
#20329=CARTESIAN_POINT('Ctrl Pts',(1.08940878963422,-0.144299303100741,
-0.276273267473431));
#20330=CARTESIAN_POINT('Ctrl Pts',(1.09443784939331,-0.177024326825049,
-0.256354979351213));
#20331=CARTESIAN_POINT('Ctrl Pts',(1.10373487993589,-0.227269801620064,
-0.212533521233765));
#20332=CARTESIAN_POINT('Ctrl Pts',(1.10909715583869,-0.251265615809407,
-0.183354415742157));
#20333=CARTESIAN_POINT('Ctrl Pts',(1.1160463456491,-0.279889827963178,-0.133783682657561));
#20334=CARTESIAN_POINT('Ctrl Pts',(1.11894887330541,-0.290879136862659,
-0.107881990270302));
#20335=CARTESIAN_POINT('Ctrl Pts',(1.12284346704144,-0.305251990234488,
-0.0539226701638766));
#20336=CARTESIAN_POINT('Ctrl Pts',(1.123812,-0.308638795020976,-0.025864214957475));
#20337=CARTESIAN_POINT('Ctrl Pts',(1.123812,-0.308638795020976,0.025864214957475));
#20338=CARTESIAN_POINT('Ctrl Pts',(1.12284346704144,-0.305251990234488,
0.0539226701638766));
#20339=CARTESIAN_POINT('Ctrl Pts',(1.11894887330541,-0.290879136862659,
0.107881990270302));
#20340=CARTESIAN_POINT('Ctrl Pts',(1.1160463456491,-0.279889827963178,0.133783682657561));
#20341=CARTESIAN_POINT('Ctrl Pts',(1.10909715583869,-0.251265615809407,
0.183354415742157));
#20342=CARTESIAN_POINT('Ctrl Pts',(1.10373487993589,-0.227269801620064,
0.212533521233765));
#20343=CARTESIAN_POINT('Ctrl Pts',(1.09443784939331,-0.177024326825049,
0.256354979351213));
#20344=CARTESIAN_POINT('Ctrl Pts',(1.08940878963422,-0.144299303100741,
0.276273267473431));
#20345=CARTESIAN_POINT('Ctrl Pts',(1.08431331394788,-0.0928409665394228,
0.2953917518996));
#20346=CARTESIAN_POINT('Ctrl Pts',(1.0830271513892,-0.0762225747374255,
0.300028012588062));
#20347=CARTESIAN_POINT('Ctrl Pts',(1.08212377959455,-0.0595300000000001,
0.303251606722892));
#20348=CARTESIAN_POINT('Origin',(0.,-0.05953,0.));
#20349=CARTESIAN_POINT('Origin',(0.,-0.05953,0.));
#20350=CARTESIAN_POINT('',(0.0589974094846122,-0.05953,1.07456964270265));
#20351=CARTESIAN_POINT('Origin',(0.,-0.05953,0.));
#20352=CARTESIAN_POINT('Origin',(-0.244773027351946,-0.05953,1.07242070340001));
#20353=CARTESIAN_POINT('Origin',(-0.244773027351946,0.,1.07242070340001));
#20354=CARTESIAN_POINT('',(-0.519393123750572,-0.05953,0.942555777842682));
#20355=CARTESIAN_POINT('Ctrl Pts',(-0.519393123750572,-0.05953,0.942555777842682));
#20356=CARTESIAN_POINT('Ctrl Pts',(-0.513714466572041,-0.0925528133349865,
0.945684988399766));
#20357=CARTESIAN_POINT('Ctrl Pts',(-0.503136848051455,-0.124911173756694,
0.951483858396181));
#20358=CARTESIAN_POINT('Ctrl Pts',(-0.47593627990192,-0.177924977804098,
0.965323333309091));
#20359=CARTESIAN_POINT('Ctrl Pts',(-0.460931856495794,-0.199697230012983,
0.972669835243841));
#20360=CARTESIAN_POINT('Ctrl Pts',(-0.426157505475872,-0.237895043532788,
0.988400002689705));
#20361=CARTESIAN_POINT('Ctrl Pts',(-0.406380688682952,-0.254319232363049,
0.996771768218699));
#20362=CARTESIAN_POINT('Ctrl Pts',(-0.364750145543744,-0.28018331644634,
1.01272583306292));
#20363=CARTESIAN_POINT('Ctrl Pts',(-0.340838910881557,-0.29104845371857,
1.02112815447116));
#20364=CARTESIAN_POINT('Ctrl Pts',(-0.290495481564827,-0.30527573347708,
1.036574285215));
#20365=CARTESIAN_POINT('Ctrl Pts',(-0.264056468041074,-0.308638795020976,
1.04359501395068));
#20366=CARTESIAN_POINT('Ctrl Pts',(-0.214892249704082,-0.308638795020976,
1.05481642595959));
#20367=CARTESIAN_POINT('Ctrl Pts',(-0.188025341585962,-0.30527573347708,
1.05996242598502));
#20368=CARTESIAN_POINT('Ctrl Pts',(-0.135965654106109,-0.29104845371857,
1.06788913840721));
#20369=CARTESIAN_POINT('Ctrl Pts',(-0.110776745452494,-0.28018331644634,
1.07069360430242));
#20370=CARTESIAN_POINT('Ctrl Pts',(-0.0663467128214646,-0.254319232363049,
1.07438230428002));
#20371=CARTESIAN_POINT('Ctrl Pts',(-0.0448960436540983,-0.237895043532788,
1.07542044338697));
#20372=CARTESIAN_POINT('Ctrl Pts',(-0.00674037211528124,-0.199697230012983,
1.07633607767727));
#20373=CARTESIAN_POINT('Ctrl Pts',(0.00996567398334777,-0.177924977804098,
1.07622728347683));
#20374=CARTESIAN_POINT('Ctrl Pts',(0.0404772621979741,-0.124911173756694,
1.07556023164702));
#20375=CARTESIAN_POINT('Ctrl Pts',(0.0525234025782719,-0.0925528133349865,
1.07492508698591));
#20376=CARTESIAN_POINT('Ctrl Pts',(0.0589974094846124,-0.05953,1.07456964270265));
#20377=CARTESIAN_POINT('Origin',(-0.244773027351946,-0.05953,1.07242070340001));
#20378=CARTESIAN_POINT('Origin',(0.,-0.05953,0.));
#20379=CARTESIAN_POINT('',(-0.803348093619616,-0.05953,0.716109245731214));
#20380=CARTESIAN_POINT('Origin',(0.,-0.05953,0.));
#20381=CARTESIAN_POINT('Origin',(-0.991065754692661,-0.05953,0.477272113029314));
#20382=CARTESIAN_POINT('Origin',(-0.991065754692661,0.,0.477272113029314));
#20383=CARTESIAN_POINT('',(-1.06075609691358,-0.05953,0.181596019242328));
#20384=CARTESIAN_POINT('Ctrl Pts',(-1.06075609691358,-0.05953,0.181596019242328));
#20385=CARTESIAN_POINT('Ctrl Pts',(-1.05966202740332,-0.0925528133349865,
0.187986803072856));
#20386=CARTESIAN_POINT('Ctrl Pts',(-1.05760072925372,-0.124911173756694,
0.199872254546857));
#20387=CARTESIAN_POINT('Ctrl Pts',(-1.05146158959546,-0.177924977804098,
0.22976728653846));
#20388=CARTESIAN_POINT('Ctrl Pts',(-1.04785021111757,-0.199697230012983,
0.246078686169301));
#20389=CARTESIAN_POINT('Ctrl Pts',(-1.03846709802406,-0.237895043532788,
0.283073967563097));
#20390=CARTESIAN_POINT('Ctrl Pts',(-1.03268176429485,-0.254319232363049,
0.303755815985685));
#20391=CARTESIAN_POINT('Ctrl Pts',(-1.01919893537026,-0.28018331644634,
0.346251081972725));
#20392=CARTESIAN_POINT('Ctrl Pts',(-1.01085972381132,-0.29104845371857,
0.370184399726282));
#20393=CARTESIAN_POINT('Ctrl Pts',(-0.99154738033959,-0.30527573347708,
0.419174982698463));
#20394=CARTESIAN_POINT('Ctrl Pts',(-0.980551951791748,-0.308638795020976,
0.444223188605045));
#20395=CARTESIAN_POINT('Ctrl Pts',(-0.958671816228589,-0.308638795020976,
0.489657758261848));
#20396=CARTESIAN_POINT('Ctrl Pts',(-0.945943877838127,-0.30527573347708,
0.51387163140139));
#20397=CARTESIAN_POINT('Ctrl Pts',(-0.91968254693063,-0.29104845371857,
0.559515758398093));
#20398=CARTESIAN_POINT('Ctrl Pts',(-0.906170138993533,-0.28018331644634,
0.580957796077825));
#20399=CARTESIAN_POINT('Ctrl Pts',(-0.8813524085237,-0.254319232363049,
0.617994461173994));
#20400=CARTESIAN_POINT('Ctrl Pts',(-0.868789784891799,-0.237895043532788,
0.635412538795143));
#20401=CARTESIAN_POINT('Ctrl Pts',(-0.845715984518854,-0.199697230012983,
0.66581473268113));
#20402=CARTESIAN_POINT('Ctrl Pts',(-0.835214876415962,-0.177924977804098,
0.678808213394124));
#20403=CARTESIAN_POINT('Ctrl Pts',(-0.815669690204649,-0.124911173756694,
0.702247233627224));
#20404=CARTESIAN_POINT('Ctrl Pts',(-0.807662468433796,-0.0925528133349865,
0.711269279199861));
#20405=CARTESIAN_POINT('Ctrl Pts',(-0.803348093619616,-0.05953,0.716109245731214));
#20406=CARTESIAN_POINT('Origin',(-0.991065754692661,-0.05953,0.477272113029314));
#20407=CARTESIAN_POINT('Origin',(0.,-0.05953,0.));
#20408=CARTESIAN_POINT('',(-1.076188,-0.05953,1.31795018948079E-16));
#20409=CARTESIAN_POINT('Origin',(0.,-0.05953,0.));
#20410=CARTESIAN_POINT('',(-1.06075609691358,-0.05953,-0.181596019242328));
#20411=CARTESIAN_POINT('Origin',(0.,-0.05953,0.));
#20412=CARTESIAN_POINT('Origin',(-0.991065754692661,-0.05953,-0.477272113029314));
#20413=CARTESIAN_POINT('Origin',(-0.991065754692661,0.,-0.477272113029314));
#20414=CARTESIAN_POINT('',(-0.803348093619616,-0.05953,-0.716109245731215));
#20415=CARTESIAN_POINT('Ctrl Pts',(-0.803348093619616,-0.05953,-0.716109245731215));
#20416=CARTESIAN_POINT('Ctrl Pts',(-0.807662468433795,-0.0925528133349865,
-0.711269279199862));
#20417=CARTESIAN_POINT('Ctrl Pts',(-0.815669690204649,-0.124911173756694,
-0.702247233627224));
#20418=CARTESIAN_POINT('Ctrl Pts',(-0.835214876415962,-0.177924977804098,
-0.678808213394124));
#20419=CARTESIAN_POINT('Ctrl Pts',(-0.845715984518854,-0.199697230012983,
-0.66581473268113));
#20420=CARTESIAN_POINT('Ctrl Pts',(-0.868789784891799,-0.237895043532788,
-0.635412538795143));
#20421=CARTESIAN_POINT('Ctrl Pts',(-0.8813524085237,-0.254319232363049,
-0.617994461173994));
#20422=CARTESIAN_POINT('Ctrl Pts',(-0.906170138993533,-0.28018331644634,
-0.580957796077826));
#20423=CARTESIAN_POINT('Ctrl Pts',(-0.91968254693063,-0.29104845371857,
-0.559515758398093));
#20424=CARTESIAN_POINT('Ctrl Pts',(-0.945943877838127,-0.30527573347708,
-0.51387163140139));
#20425=CARTESIAN_POINT('Ctrl Pts',(-0.958671816228589,-0.308638795020976,
-0.489657758261848));
#20426=CARTESIAN_POINT('Ctrl Pts',(-0.980551951791748,-0.308638795020976,
-0.444223188605045));
#20427=CARTESIAN_POINT('Ctrl Pts',(-0.99154738033959,-0.30527573347708,
-0.419174982698463));
#20428=CARTESIAN_POINT('Ctrl Pts',(-1.01085972381132,-0.29104845371857,
-0.370184399726282));
#20429=CARTESIAN_POINT('Ctrl Pts',(-1.01919893537026,-0.28018331644634,
-0.346251081972725));
#20430=CARTESIAN_POINT('Ctrl Pts',(-1.03268176429485,-0.254319232363049,
-0.303755815985685));
#20431=CARTESIAN_POINT('Ctrl Pts',(-1.03846709802406,-0.237895043532788,
-0.283073967563097));
#20432=CARTESIAN_POINT('Ctrl Pts',(-1.04785021111757,-0.199697230012983,
-0.246078686169302));
#20433=CARTESIAN_POINT('Ctrl Pts',(-1.05146158959546,-0.177924977804098,
-0.229767286538461));
#20434=CARTESIAN_POINT('Ctrl Pts',(-1.05760072925372,-0.124911173756694,
-0.199872254546858));
#20435=CARTESIAN_POINT('Ctrl Pts',(-1.05966202740332,-0.0925528133349864,
-0.187986803072857));
#20436=CARTESIAN_POINT('Ctrl Pts',(-1.06075609691358,-0.05953,-0.181596019242328));
#20437=CARTESIAN_POINT('Origin',(-0.991065754692661,-0.05953,-0.477272113029314));
#20438=CARTESIAN_POINT('Origin',(0.,-0.05953,0.));
#20439=CARTESIAN_POINT('',(-0.519393123750572,-0.05953,-0.942555777842682));
#20440=CARTESIAN_POINT('Origin',(0.,-0.05953,0.));
#20441=CARTESIAN_POINT('Origin',(-0.244773027351946,-0.05953,-1.07242070340001));
#20442=CARTESIAN_POINT('Origin',(-0.244773027351946,0.,-1.07242070340001));
#20443=CARTESIAN_POINT('',(0.0589974094846125,-0.05953,-1.07456964270265));
#20444=CARTESIAN_POINT('Ctrl Pts',(0.0589974094846127,-0.05953,-1.07456964270265));
#20445=CARTESIAN_POINT('Ctrl Pts',(0.0525234025782722,-0.0925528133349865,
-1.07492508698591));
#20446=CARTESIAN_POINT('Ctrl Pts',(0.0404772621979744,-0.124911173756694,
-1.07556023164702));
#20447=CARTESIAN_POINT('Ctrl Pts',(0.0099656739833481,-0.177924977804098,
-1.07622728347683));
#20448=CARTESIAN_POINT('Ctrl Pts',(-0.00674037211528096,-0.199697230012983,
-1.07633607767727));
#20449=CARTESIAN_POINT('Ctrl Pts',(-0.044896043654098,-0.237895043532788,
-1.07542044338697));
#20450=CARTESIAN_POINT('Ctrl Pts',(-0.0663467128214644,-0.254319232363049,
-1.07438230428002));
#20451=CARTESIAN_POINT('Ctrl Pts',(-0.110776745452493,-0.28018331644634,
-1.07069360430242));
#20452=CARTESIAN_POINT('Ctrl Pts',(-0.135965654106109,-0.29104845371857,
-1.06788913840721));
#20453=CARTESIAN_POINT('Ctrl Pts',(-0.188025341585962,-0.30527573347708,
-1.05996242598502));
#20454=CARTESIAN_POINT('Ctrl Pts',(-0.214892249704082,-0.308638795020976,
-1.05481642595959));
#20455=CARTESIAN_POINT('Ctrl Pts',(-0.264056468041074,-0.308638795020976,
-1.04359501395068));
#20456=CARTESIAN_POINT('Ctrl Pts',(-0.290495481564827,-0.30527573347708,
-1.036574285215));
#20457=CARTESIAN_POINT('Ctrl Pts',(-0.340838910881557,-0.291048453718569,
-1.02112815447116));
#20458=CARTESIAN_POINT('Ctrl Pts',(-0.364750145543744,-0.28018331644634,
-1.01272583306292));
#20459=CARTESIAN_POINT('Ctrl Pts',(-0.406380688682952,-0.254319232363049,
-0.996771768218699));
#20460=CARTESIAN_POINT('Ctrl Pts',(-0.426157505475872,-0.237895043532788,
-0.988400002689705));
#20461=CARTESIAN_POINT('Ctrl Pts',(-0.460931856495794,-0.199697230012983,
-0.972669835243841));
#20462=CARTESIAN_POINT('Ctrl Pts',(-0.475936279901919,-0.177924977804098,
-0.965323333309091));
#20463=CARTESIAN_POINT('Ctrl Pts',(-0.503136848051454,-0.124911173756694,
-0.951483858396181));
#20464=CARTESIAN_POINT('Ctrl Pts',(-0.513714466572041,-0.0925528133349865,
-0.945684988399766));
#20465=CARTESIAN_POINT('Ctrl Pts',(-0.519393123750572,-0.05953,-0.942555777842682));
#20466=CARTESIAN_POINT('Origin',(-0.244773027351946,-0.05953,-1.07242070340001));
#20467=CARTESIAN_POINT('Origin',(0.,-0.05953,0.));
#20468=CARTESIAN_POINT('',(0.413083465285518,-0.05953,-0.993751811093549));
#20469=CARTESIAN_POINT('Origin',(0.,-0.05953,0.));
#20470=CARTESIAN_POINT('Origin',(0.685838782044607,-0.05953,-0.860014630714833));
#20471=CARTESIAN_POINT('Origin',(0.685838782044607,0.,-0.860014630714833));
#20472=CARTESIAN_POINT('',(0.876916659919095,-0.05953,-0.623857181492959));
#20473=CARTESIAN_POINT('Ctrl Pts',(0.876916659919095,-0.05953,-0.623857181492958));
#20474=CARTESIAN_POINT('Ctrl Pts',(0.873158080166742,-0.0925528133349865,
-0.62914037979579));
#20475=CARTESIAN_POINT('Ctrl Pts',(0.866144010579847,-0.124911173756694,
-0.638954437806245));
#20476=CARTESIAN_POINT('Ctrl Pts',(0.847641868610495,-0.177924977804098,
-0.663225258065736));
#20477=CARTESIAN_POINT('Ctrl Pts',(0.837310877969633,-0.199697230012983,
-0.676354402927683));
#20478=CARTESIAN_POINT('Ctrl Pts',(0.81280533416753,-0.237895043532788,
-0.705614819529209));
#20479=CARTESIAN_POINT('Ctrl Pts',(0.798619410861634,-0.254319232363049,
-0.721738358858166));
#20480=CARTESIAN_POINT('Ctrl Pts',(0.768033796848072,-0.28018331644634,
-0.754175290318038));
#20481=CARTESIAN_POINT('Ctrl Pts',(0.750136149454208,-0.29104845371857,
-0.772120216227122));
#20482=CARTESIAN_POINT('Ctrl Pts',(0.711480111898423,-0.30527573347708,
-0.807879894508811));
#20483=CARTESIAN_POINT('Ctrl Pts',(0.690705563850638,-0.308638795020976,
-0.825676810575913));
#20484=CARTESIAN_POINT('Ctrl Pts',(0.651278921914856,-0.308638795020976,
-0.857118508332695));
#20485=CARTESIAN_POINT('Ctrl Pts',(0.629305439856167,-0.30527573347708,
-0.873412008702649));
#20486=CARTESIAN_POINT('Ctrl Pts',(0.585840553788742,-0.29104845371857,
-0.903141581680914));
#20487=CARTESIAN_POINT('Ctrl Pts',(0.564362943424239,-0.28018331644634,
-0.916597376014514));
#20488=CARTESIAN_POINT('Ctrl Pts',(0.525933334162556,-0.254319232363049,
-0.939198248544427));
#20489=CARTESIAN_POINT('Ctrl Pts',(0.507057380724533,-0.237895043532788,
-0.949440676105255));
#20490=CARTESIAN_POINT('Ctrl Pts',(0.473077587363686,-0.199697230012983,
-0.966820759530997));
#20491=CARTESIAN_POINT('Ctrl Pts',(0.457978755888596,-0.177924977804098,
-0.973971221090534));
#20492=CARTESIAN_POINT('Ctrl Pts',(0.430199341854858,-0.124911173756694,
-0.986608710139579));
#20493=CARTESIAN_POINT('Ctrl Pts',(0.419070565453384,-0.0925528133349865,
-0.991263089003441));
#20494=CARTESIAN_POINT('Ctrl Pts',(0.413083465285518,-0.05953,-0.993751811093549));
#20495=CARTESIAN_POINT('Origin',(0.685838782044607,-0.05953,-0.860014630714833));
#20496=CARTESIAN_POINT('Origin',(0.,-0.208355,0.));
#20497=CARTESIAN_POINT('',(-1.076188,-0.35718,1.31795018948079E-16));
#20498=CARTESIAN_POINT('Origin',(0.,-0.35718,0.));
#20499=CARTESIAN_POINT('',(-1.076188,-0.208355,1.31795018948079E-16));
#20500=CARTESIAN_POINT('',(1.03449977959455,-0.05953,0.296632461748266));
#20501=CARTESIAN_POINT('Origin',(0.,-0.05953,0.));
#20502=CARTESIAN_POINT('',(1.03449977959455,-0.05953,-0.296632461748266));
#20503=CARTESIAN_POINT('Ctrl Pts',(1.03449977959455,-0.05953,0.296632461748267));
#20504=CARTESIAN_POINT('Ctrl Pts',(1.03628691421076,-0.0925528133349865,
0.290399865505497));
#20505=CARTESIAN_POINT('Ctrl Pts',(1.03958665287714,-0.124911173756694,
0.278797079997872));
#20506=CARTESIAN_POINT('Ctrl Pts',(1.0470264474309,-0.177924977804098,0.249198913998601));
#20507=CARTESIAN_POINT('Ctrl Pts',(1.05084995891418,-0.199697230012983,
0.232935932341942));
#20508=CARTESIAN_POINT('Ctrl Pts',(1.05844771715377,-0.237895043532788,
0.195533155353269));
#20509=CARTESIAN_POINT('Ctrl Pts',(1.06220882929878,-0.254319232363049,
0.17438929156337));
#20510=CARTESIAN_POINT('Ctrl Pts',(1.06849922508772,-0.28018331644634,0.130252399648131));
#20511=CARTESIAN_POINT('Ctrl Pts',(1.07137013248666,-0.29104845371857,0.105070977154072));
#20512=CARTESIAN_POINT('Ctrl Pts',(1.07522652957392,-0.30527573347708,0.0525526752791107));
#20513=CARTESIAN_POINT('Ctrl Pts',(1.076188,-0.308638795020976,0.025214283908933));
#20514=CARTESIAN_POINT('Ctrl Pts',(1.076188,-0.308638795020976,-0.025214283908933));
#20515=CARTESIAN_POINT('Ctrl Pts',(1.07522652957392,-0.30527573347708,-0.0525526752791107));
#20516=CARTESIAN_POINT('Ctrl Pts',(1.07137013248666,-0.29104845371857,-0.105070977154072));
#20517=CARTESIAN_POINT('Ctrl Pts',(1.06849922508772,-0.28018331644634,-0.130252399648131));
#20518=CARTESIAN_POINT('Ctrl Pts',(1.06220882929878,-0.254319232363049,
-0.17438929156337));
#20519=CARTESIAN_POINT('Ctrl Pts',(1.05844771715377,-0.237895043532788,
-0.195533155353269));
#20520=CARTESIAN_POINT('Ctrl Pts',(1.05084995891418,-0.199697230012983,
-0.232935932341942));
#20521=CARTESIAN_POINT('Ctrl Pts',(1.0470264474309,-0.177924977804098,-0.249198913998601));
#20522=CARTESIAN_POINT('Ctrl Pts',(1.03958665287714,-0.124911173756694,
-0.278797079997872));
#20523=CARTESIAN_POINT('Ctrl Pts',(1.03628691421076,-0.0925528133349865,
-0.290399865505497));
#20524=CARTESIAN_POINT('Ctrl Pts',(1.03449977959455,-0.05953,-0.296632461748267));
#20525=CARTESIAN_POINT('Origin',(0.,-0.05953,0.));
#20526=CARTESIAN_POINT('Origin',(0.,-0.05953,0.));
#20527=CARTESIAN_POINT('Origin',(1.1,-0.05953,0.));
#20528=CARTESIAN_POINT('Origin',(1.1,0.,0.));
#20529=CARTESIAN_POINT('Origin',(1.1,-0.05953,0.));
#20530=CARTESIAN_POINT('Origin',(0.,-0.35718,0.));
#20531=CARTESIAN_POINT('Origin',(0.,-0.05953,0.));
#20532=CARTESIAN_POINT('',(0.,0.,0.));
#20533=CARTESIAN_POINT('Origin',(1.119765,0.495,0.));
#20534=CARTESIAN_POINT('',(-1.119765,0.495,-1.37131662304724E-16));
#20535=CARTESIAN_POINT('Origin',(0.,0.495,0.));
#20536=CARTESIAN_POINT('',(-1.085235,0.495,-1.32902956907268E-16));
#20537=CARTESIAN_POINT('Origin',(0.,0.495,0.));
#20538=CARTESIAN_POINT('Origin',(0.,0.4575,0.));
#20539=CARTESIAN_POINT('',(-1.119765,0.42,-1.37131662304724E-16));
#20540=CARTESIAN_POINT('Origin',(0.,0.42,0.));
#20541=CARTESIAN_POINT('',(-1.119765,0.4575,-1.37131662304724E-16));
#20542=CARTESIAN_POINT('Origin',(1.085235,0.42,0.));
#20543=CARTESIAN_POINT('',(-1.085235,0.42,-1.32902956907268E-16));
#20544=CARTESIAN_POINT('Origin',(0.,0.42,0.));
#20545=CARTESIAN_POINT('Origin',(0.,0.4575,0.));
#20546=CARTESIAN_POINT('',(-1.085235,0.4575,-1.32902956907268E-16));
#20547=CARTESIAN_POINT('Origin',(1.119765,-0.42,0.));
#20548=CARTESIAN_POINT('',(-1.119765,-0.42,-1.37131662304724E-16));
#20549=CARTESIAN_POINT('Origin',(0.,-0.42,0.));
#20550=CARTESIAN_POINT('',(-1.085235,-0.42,-1.32902956907268E-16));
#20551=CARTESIAN_POINT('Origin',(0.,-0.42,0.));
#20552=CARTESIAN_POINT('Origin',(0.,-0.4575,0.));
#20553=CARTESIAN_POINT('',(-1.119765,-0.495,-1.37131662304724E-16));
#20554=CARTESIAN_POINT('Origin',(0.,-0.495,0.));
#20555=CARTESIAN_POINT('',(-1.119765,-0.4575,-1.37131662304724E-16));
#20556=CARTESIAN_POINT('Origin',(1.085235,-0.495,0.));
#20557=CARTESIAN_POINT('',(-1.085235,-0.495,-1.32902956907268E-16));
#20558=CARTESIAN_POINT('Origin',(0.,-0.495,0.));
#20559=CARTESIAN_POINT('Origin',(0.,-0.4575,0.));
#20560=CARTESIAN_POINT('',(-1.085235,-0.4575,-1.32902956907268E-16));
#20561=CARTESIAN_POINT('',(0.,0.,0.));
#20562=CARTESIAN_POINT('',(0.,0.,0.));
#20563=CARTESIAN_POINT('',(0.,0.,0.));
#20564=CARTESIAN_POINT('',(0.,0.,0.));
#20565=CARTESIAN_POINT('',(0.,0.,0.));
#20566=CARTESIAN_POINT('',(0.,0.,0.));
#20567=CARTESIAN_POINT('Origin',(0.3,0.4,0.));
#20568=CARTESIAN_POINT('',(-0.3,0.4,-3.67394039744206E-17));
#20569=CARTESIAN_POINT('Origin',(0.,0.4,0.));
#20570=CARTESIAN_POINT('Origin',(0.,0.375,0.));
#20571=CARTESIAN_POINT('',(-0.35,0.35,-4.28626379701573E-17));
#20572=CARTESIAN_POINT('Origin',(0.,0.35,0.));
#20573=CARTESIAN_POINT('',(-0.325,0.375,-3.9801020972289E-17));
#20574=CARTESIAN_POINT('Origin',(0.,0.19,0.));
#20575=CARTESIAN_POINT('',(-0.35,0.03,-4.28626379701574E-17));
#20576=CARTESIAN_POINT('Origin',(0.,0.03,0.));
#20577=CARTESIAN_POINT('',(-0.35,0.19,-4.28626379701574E-17));
#20578=CARTESIAN_POINT('Origin',(0.,0.0149999999999999,0.));
#20579=CARTESIAN_POINT('',(-0.32,-3.29597460435593E-17,-3.91886975727153E-17));
#20580=CARTESIAN_POINT('Origin',(0.,0.,0.));
#20581=CARTESIAN_POINT('',(-0.335,0.0149999999999999,-4.10256677714363E-17));
#20582=CARTESIAN_POINT('Origin',(0.22,0.,0.));
#20583=CARTESIAN_POINT('',(-0.22,-6.93889390390723E-18,-2.69422295812418E-17));
#20584=CARTESIAN_POINT('Origin',(0.,0.,0.));
#20585=CARTESIAN_POINT('Origin',(0.,-0.02,0.));
#20586=CARTESIAN_POINT('',(-0.1954,-0.0492,2.39295984553393E-17));
#20587=CARTESIAN_POINT('Origin',(0.,-0.0492,0.));
#20588=CARTESIAN_POINT('',(-0.21,-0.02,-2.57175827820944E-17));
#20589=CARTESIAN_POINT('Origin',(0.,-0.8,0.));
#20590=CARTESIAN_POINT('',(-0.1954,-1.5646,2.39295984553393E-17));
#20591=CARTESIAN_POINT('Origin',(0.,-1.5646,0.));
#20592=CARTESIAN_POINT('',(-0.1954,-0.8,-2.39295984553393E-17));
#20593=CARTESIAN_POINT('Origin',(0.,-1.58,0.));
#20594=CARTESIAN_POINT('',(-0.16,-1.6,-1.95943487863577E-17));
#20595=CARTESIAN_POINT('Origin',(0.,-1.6,0.));
#20596=CARTESIAN_POINT('',(-0.18,-1.58,-2.20436423846524E-17));
#20597=CARTESIAN_POINT('Origin',(0.,-1.6,0.));
#20598=CARTESIAN_POINT('Origin',(0.0866025403784439,-0.4,-0.15));
#20599=CARTESIAN_POINT('',(0.173205080756888,-0.4,0.));
#20600=CARTESIAN_POINT('',(0.0866025403784439,-0.4,-0.15));
#20601=CARTESIAN_POINT('',(0.173205080756888,-0.4,0.));
#20602=CARTESIAN_POINT('',(0.0866025403784439,-0.64,-0.15));
#20603=CARTESIAN_POINT('',(0.0866025403784439,-0.4,-0.15));
#20604=CARTESIAN_POINT('',(0.173205080756888,-0.64,0.));
#20605=CARTESIAN_POINT('',(0.173205080756888,-0.64,0.));
#20606=CARTESIAN_POINT('',(0.173205080756888,-0.4,0.));
#20607=CARTESIAN_POINT('Origin',(-0.0866025403784438,-0.4,-0.15));
#20608=CARTESIAN_POINT('',(-0.0866025403784438,-0.4,-0.15));
#20609=CARTESIAN_POINT('',(0.0866025403784439,-0.4,-0.15));
#20610=CARTESIAN_POINT('',(-0.0866025403784438,-0.64,-0.15));
#20611=CARTESIAN_POINT('',(-0.0866025403784438,-0.4,-0.15));
#20612=CARTESIAN_POINT('',(0.0866025403784439,-0.64,-0.15));
#20613=CARTESIAN_POINT('Origin',(-0.173205080756888,-0.4,-2.77555756156289E-17));
#20614=CARTESIAN_POINT('',(-0.173205080756888,-0.4,-2.12115047744981E-17));
#20615=CARTESIAN_POINT('',(-0.0866025403784438,-0.4,-0.15));
#20616=CARTESIAN_POINT('',(-0.173205080756888,-0.64,-2.77555756156289E-17));
#20617=CARTESIAN_POINT('',(-0.173205080756888,-0.4,-2.12115047744981E-17));
#20618=CARTESIAN_POINT('',(-0.0866025403784438,-0.64,-0.15));
#20619=CARTESIAN_POINT('Origin',(-0.0866025403784439,-0.4,0.15));
#20620=CARTESIAN_POINT('',(-0.0866025403784439,-0.4,0.15));
#20621=CARTESIAN_POINT('',(-0.173205080756888,-0.4,-2.12115047744981E-17));
#20622=CARTESIAN_POINT('',(-0.0866025403784439,-0.64,0.15));
#20623=CARTESIAN_POINT('',(-0.0866025403784439,-0.4,0.15));
#20624=CARTESIAN_POINT('',(-0.173205080756888,-0.64,-2.12115047744981E-17));
#20625=CARTESIAN_POINT('Origin',(0.0866025403784439,-0.4,0.15));
#20626=CARTESIAN_POINT('',(0.0866025403784439,-0.4,0.15));
#20627=CARTESIAN_POINT('',(-0.0866025403784439,-0.4,0.15));
#20628=CARTESIAN_POINT('',(0.0866025403784439,-0.64,0.15));
#20629=CARTESIAN_POINT('',(0.0866025403784439,-0.4,0.15));
#20630=CARTESIAN_POINT('',(-0.0866025403784439,-0.64,0.15));
#20631=CARTESIAN_POINT('Origin',(0.173205080756888,-0.4,0.));
#20632=CARTESIAN_POINT('',(0.0866025403784439,-0.4,0.15));
#20633=CARTESIAN_POINT('',(0.0866025403784439,-0.64,0.15));
#20634=CARTESIAN_POINT('Origin',(0.,-0.4,-2.77555756156289E-17));
#20635=CARTESIAN_POINT('Origin',(0.,-0.64,-2.77555756156289E-17));
#20636=CARTESIAN_POINT('',(0.,0.,0.));
#20637=CARTESIAN_POINT('',(0.,0.,0.));
#20638=CARTESIAN_POINT('Origin',(3.8079689783217,-2.1920310216783,2.3));
#20639=CARTESIAN_POINT('',(3.5979689783217,-2.1920310216783,2.4));
#20640=CARTESIAN_POINT('Origin',(3.8079689783217,-2.1920310216783,2.4));
#20641=CARTESIAN_POINT('',(3.5979689783217,-2.1920310216783,3.2));
#20642=CARTESIAN_POINT('',(3.5979689783217,-2.1920310216783,2.3));
#20643=CARTESIAN_POINT('Origin',(3.8079689783217,-2.1920310216783,3.2));
#20644=CARTESIAN_POINT('Origin',(3.8079689783217,2.1920310216783,2.3));
#20645=CARTESIAN_POINT('',(3.5979689783217,2.1920310216783,2.4));
#20646=CARTESIAN_POINT('Origin',(3.8079689783217,2.1920310216783,2.4));
#20647=CARTESIAN_POINT('',(3.5979689783217,2.1920310216783,3.2));
#20648=CARTESIAN_POINT('',(3.5979689783217,2.1920310216783,2.3));
#20649=CARTESIAN_POINT('Origin',(3.8079689783217,2.1920310216783,3.2));
#20650=CARTESIAN_POINT('Origin',(8.1920310216783,2.1920310216783,2.3));
#20651=CARTESIAN_POINT('',(7.9820310216783,2.1920310216783,2.4));
#20652=CARTESIAN_POINT('Origin',(8.1920310216783,2.1920310216783,2.4));
#20653=CARTESIAN_POINT('',(7.9820310216783,2.1920310216783,3.2));
#20654=CARTESIAN_POINT('',(7.9820310216783,2.1920310216783,2.3));
#20655=CARTESIAN_POINT('Origin',(8.1920310216783,2.1920310216783,3.2));
#20656=CARTESIAN_POINT('Origin',(8.1920310216783,-2.1920310216783,2.3));
#20657=CARTESIAN_POINT('',(7.9820310216783,-2.1920310216783,2.4));
#20658=CARTESIAN_POINT('Origin',(8.1920310216783,-2.1920310216783,2.4));
#20659=CARTESIAN_POINT('',(7.9820310216783,-2.1920310216783,3.2));
#20660=CARTESIAN_POINT('',(7.9820310216783,-2.1920310216783,2.3));
#20661=CARTESIAN_POINT('Origin',(8.1920310216783,-2.1920310216783,3.2));
#20662=CARTESIAN_POINT('Origin',(9.5,7.19,1.1));
#20663=CARTESIAN_POINT('',(9.335,7.2,1.1));
#20664=CARTESIAN_POINT('Origin',(9.5,7.2,1.1));
#20665=CARTESIAN_POINT('',(9.335,8.2,1.1));
#20666=CARTESIAN_POINT('',(9.335,7.19,1.1));
#20667=CARTESIAN_POINT('Origin',(9.5,8.2,1.1));
#20668=CARTESIAN_POINT('Origin',(9.9,8.2,0.8));
#20669=CARTESIAN_POINT('',(9.9,8.2,0.8));
#20670=CARTESIAN_POINT('',(9.1,8.2,0.8));
#20671=CARTESIAN_POINT('',(9.9,8.2,0.8));
#20672=CARTESIAN_POINT('',(9.1,8.2,2.4));
#20673=CARTESIAN_POINT('',(9.1,8.2,0.8));
#20674=CARTESIAN_POINT('',(9.9,8.2,2.4));
#20675=CARTESIAN_POINT('',(7.95,8.2,2.4));
#20676=CARTESIAN_POINT('',(9.9,8.2,0.8));
#20677=CARTESIAN_POINT('Origin',(9.9,7.2,0.8));
#20678=CARTESIAN_POINT('',(9.9,7.2,0.8));
#20679=CARTESIAN_POINT('',(9.9,7.2,0.8));
#20680=CARTESIAN_POINT('',(9.9,7.2,2.4));
#20681=CARTESIAN_POINT('',(9.9,4.975,2.4));
#20682=CARTESIAN_POINT('',(9.9,7.2,0.8));
#20683=CARTESIAN_POINT('Origin',(9.1,7.2,0.8));
#20684=CARTESIAN_POINT('',(9.1,7.2,0.8));
#20685=CARTESIAN_POINT('',(9.1,7.2,0.8));
#20686=CARTESIAN_POINT('',(9.1,7.2,2.4));
#20687=CARTESIAN_POINT('',(7.55,7.2,2.4));
#20688=CARTESIAN_POINT('',(9.1,7.2,0.8));
#20689=CARTESIAN_POINT('Origin',(9.1,8.2,0.8));
#20690=CARTESIAN_POINT('',(9.1,8.2,0.8));
#20691=CARTESIAN_POINT('',(9.1,5.475,2.4));
#20692=CARTESIAN_POINT('Origin',(9.5,7.7,0.8));
#20693=CARTESIAN_POINT('Origin',(7.5,4.1,2.3));
#20694=CARTESIAN_POINT('',(7.225,4.1,2.4));
#20695=CARTESIAN_POINT('Origin',(7.5,4.1,2.4));
#20696=CARTESIAN_POINT('',(7.225,4.1,3.2));
#20697=CARTESIAN_POINT('',(7.225,4.1,2.3));
#20698=CARTESIAN_POINT('Origin',(7.5,4.1,3.2));
#20699=CARTESIAN_POINT('Origin',(4.5,7.9,2.3));
#20700=CARTESIAN_POINT('',(4.225,7.9,2.4));
#20701=CARTESIAN_POINT('Origin',(4.5,7.9,2.4));
#20702=CARTESIAN_POINT('',(4.225,7.9,3.2));
#20703=CARTESIAN_POINT('',(4.225,7.9,2.3));
#20704=CARTESIAN_POINT('Origin',(4.5,7.9,3.2));
#20705=CARTESIAN_POINT('Origin',(4.5,4.1,2.3));
#20706=CARTESIAN_POINT('',(4.225,4.1,2.4));
#20707=CARTESIAN_POINT('Origin',(4.5,4.1,2.4));
#20708=CARTESIAN_POINT('',(4.225,4.1,3.2));
#20709=CARTESIAN_POINT('',(4.225,4.1,2.3));
#20710=CARTESIAN_POINT('Origin',(4.5,4.1,3.2));
#20711=CARTESIAN_POINT('Origin',(7.5,7.9,2.3));
#20712=CARTESIAN_POINT('',(7.225,7.9,2.4));
#20713=CARTESIAN_POINT('Origin',(7.5,7.9,2.4));
#20714=CARTESIAN_POINT('',(7.225,7.9,3.2));
#20715=CARTESIAN_POINT('',(7.225,7.9,2.3));
#20716=CARTESIAN_POINT('Origin',(7.5,7.9,3.2));
#20717=CARTESIAN_POINT('Origin',(0.,0.,2.3));
#20718=CARTESIAN_POINT('',(2.,-1.36249770642009,3.2));
#20719=CARTESIAN_POINT('',(2.,-1.36249770642009,2.4));
#20720=CARTESIAN_POINT('',(2.,-1.36249770642009,2.3));
#20721=CARTESIAN_POINT('',(2.,1.36249770642009,3.2));
#20722=CARTESIAN_POINT('Origin',(0.,0.,3.2));
#20723=CARTESIAN_POINT('',(2.,1.36249770642009,2.4));
#20724=CARTESIAN_POINT('',(2.,1.36249770642009,2.3));
#20725=CARTESIAN_POINT('Origin',(0.,0.,2.4));
#20726=CARTESIAN_POINT('Origin',(6.,2.75,3.2));
#20727=CARTESIAN_POINT('',(2.,-3.5,3.2));
#20728=CARTESIAN_POINT('',(2.,9.,3.2));
#20729=CARTESIAN_POINT('',(10.,-3.5,3.2));
#20730=CARTESIAN_POINT('',(2.,-3.5,3.2));
#20731=CARTESIAN_POINT('',(10.,9.,3.2));
#20732=CARTESIAN_POINT('',(10.,-3.5,3.2));
#20733=CARTESIAN_POINT('',(2.,9.,3.2));
#20734=CARTESIAN_POINT('',(10.,9.,3.2));
#20735=CARTESIAN_POINT('',(2.,9.,3.2));
#20736=CARTESIAN_POINT('Origin',(2.,9.,2.4));
#20737=CARTESIAN_POINT('',(2.,-3.5,2.4));
#20738=CARTESIAN_POINT('',(2.,9.,2.4));
#20739=CARTESIAN_POINT('',(2.,-3.5,2.4));
#20740=CARTESIAN_POINT('Origin',(2.,9.,2.4));
#20741=CARTESIAN_POINT('',(2.,9.,2.4));
#20742=CARTESIAN_POINT('',(2.,9.,2.4));
#20743=CARTESIAN_POINT('',(2.,9.,2.4));
#20744=CARTESIAN_POINT('Origin',(10.,9.,2.4));
#20745=CARTESIAN_POINT('',(10.,9.,2.4));
#20746=CARTESIAN_POINT('',(10.,9.,2.4));
#20747=CARTESIAN_POINT('',(10.,9.,2.4));
#20748=CARTESIAN_POINT('Origin',(10.,-3.5,2.4));
#20749=CARTESIAN_POINT('',(10.,-3.5,2.4));
#20750=CARTESIAN_POINT('',(10.,-3.5,2.4));
#20751=CARTESIAN_POINT('',(10.,-3.5,2.4));
#20752=CARTESIAN_POINT('Origin',(2.,-3.5,2.4));
#20753=CARTESIAN_POINT('',(2.,-3.5,2.4));
#20754=CARTESIAN_POINT('Origin',(6.,2.75,2.4));
#20755=CARTESIAN_POINT('',(0.,0.,0.));
#20756=CARTESIAN_POINT('Origin',(9.8,7.2,0.8));
#20757=CARTESIAN_POINT('',(9.8,7.2,0.8));
#20758=CARTESIAN_POINT('',(9.2,7.2,0.8));
#20759=CARTESIAN_POINT('',(9.8,7.2,0.8));
#20760=CARTESIAN_POINT('',(9.2,7.2,1.4));
#20761=CARTESIAN_POINT('',(9.2,7.2,0.8));
#20762=CARTESIAN_POINT('',(9.8,7.2,1.4));
#20763=CARTESIAN_POINT('',(9.8,7.2,1.4));
#20764=CARTESIAN_POINT('',(9.8,7.2,0.8));
#20765=CARTESIAN_POINT('Origin',(9.8,6.8,0.8));
#20766=CARTESIAN_POINT('',(9.8,6.8,0.8));
#20767=CARTESIAN_POINT('',(9.8,6.8,0.8));
#20768=CARTESIAN_POINT('',(9.8,6.8,1.4));
#20769=CARTESIAN_POINT('',(9.8,6.8,1.4));
#20770=CARTESIAN_POINT('',(9.8,6.8,0.8));
#20771=CARTESIAN_POINT('Origin',(9.2,6.8,0.8));
#20772=CARTESIAN_POINT('',(9.2,6.8,0.8));
#20773=CARTESIAN_POINT('',(9.2,6.8,0.8));
#20774=CARTESIAN_POINT('',(9.2,6.8,1.4));
#20775=CARTESIAN_POINT('',(9.2,6.8,1.4));
#20776=CARTESIAN_POINT('',(9.2,6.8,0.8));
#20777=CARTESIAN_POINT('Origin',(9.2,7.2,0.8));
#20778=CARTESIAN_POINT('',(9.2,7.2,0.8));
#20779=CARTESIAN_POINT('',(9.2,7.2,1.4));
#20780=CARTESIAN_POINT('Origin',(9.5,7.,1.4));
#20781=CARTESIAN_POINT('Origin',(9.5,7.,0.8));
#20782=CARTESIAN_POINT('',(0.,0.,0.));
#20783=CARTESIAN_POINT('Origin',(7.4,0.,5.4));
#20784=CARTESIAN_POINT('',(7.58034806292791,0.25,5.4));
#20785=CARTESIAN_POINT('',(7.6,2.03914977042615E-18,5.65));
#20786=CARTESIAN_POINT('Ctrl Pts',(7.58034806292791,0.25,5.4));
#20787=CARTESIAN_POINT('Ctrl Pts',(7.58034806292791,0.25,5.43144629923968));
#20788=CARTESIAN_POINT('Ctrl Pts',(7.58138367708303,0.243704881963377,5.46495278889766));
#20789=CARTESIAN_POINT('Ctrl Pts',(7.58510750685637,0.218175602614713,5.52653198325384));
#20790=CARTESIAN_POINT('Ctrl Pts',(7.58774011537305,0.198944206314965,5.55460918427831));
#20791=CARTESIAN_POINT('Ctrl Pts',(7.59266861270428,0.154609640177667,5.59894375041561));
#20792=CARTESIAN_POINT('Ctrl Pts',(7.59528712723235,0.126532242805987,5.61817550434358));
#20793=CARTESIAN_POINT('Ctrl Pts',(7.59897861635347,0.0649523762998013,
5.64370504368363));
#20794=CARTESIAN_POINT('Ctrl Pts',(7.6,0.0314456525117888,5.65));
#20795=CARTESIAN_POINT('Ctrl Pts',(7.6,2.77555756156289E-17,5.65));
#20796=CARTESIAN_POINT('Ctrl Pts',(7.6,3.46944695195361E-17,5.65));
#20797=CARTESIAN_POINT('Ctrl Pts',(7.6,-0.0314456525117888,5.65));
#20798=CARTESIAN_POINT('Ctrl Pts',(7.59897861635347,-0.0649523762997998,
5.64370504368363));
#20799=CARTESIAN_POINT('Ctrl Pts',(7.59528712723235,-0.126532242805986,
5.61817550434358));
#20800=CARTESIAN_POINT('Ctrl Pts',(7.59266861270428,-0.154609640177666,
5.59894375041561));
#20801=CARTESIAN_POINT('Ctrl Pts',(7.58774011537305,-0.198944206314964,
5.55460918427831));
#20802=CARTESIAN_POINT('Ctrl Pts',(7.58510750685637,-0.218175602614713,
5.52653198325384));
#20803=CARTESIAN_POINT('Ctrl Pts',(7.58138367708303,-0.243704881963377,
5.46495278889766));
#20804=CARTESIAN_POINT('Ctrl Pts',(7.58034806292791,-0.25,5.43144629923968));
#20805=CARTESIAN_POINT('Ctrl Pts',(7.58034806292791,-0.25,5.36855370076032));
#20806=CARTESIAN_POINT('Ctrl Pts',(7.58138367708303,-0.243704881963377,
5.33504721110235));
#20807=CARTESIAN_POINT('Ctrl Pts',(7.58510750685637,-0.218175602614713,
5.27346801674616));
#20808=CARTESIAN_POINT('Ctrl Pts',(7.58774011537305,-0.198944206314965,
5.24539081572169));
#20809=CARTESIAN_POINT('Ctrl Pts',(7.59266861270428,-0.154609640177667,
5.20105624958439));
#20810=CARTESIAN_POINT('Ctrl Pts',(7.59528712723235,-0.126532242805987,
5.18182449565642));
#20811=CARTESIAN_POINT('Ctrl Pts',(7.59897861635347,-0.0649523762998006,
5.15629495631637));
#20812=CARTESIAN_POINT('Ctrl Pts',(7.6,-0.0314456525117888,5.15));
#20813=CARTESIAN_POINT('Ctrl Pts',(7.6,0.0314456525117887,5.15));
#20814=CARTESIAN_POINT('Ctrl Pts',(7.59897861635347,0.0649523762998006,
5.15629495631637));
#20815=CARTESIAN_POINT('Ctrl Pts',(7.59528712723235,0.126532242805986,5.18182449565642));
#20816=CARTESIAN_POINT('Ctrl Pts',(7.59266861270428,0.154609640177666,5.20105624958439));
#20817=CARTESIAN_POINT('Ctrl Pts',(7.58774011537305,0.198944206314964,5.24539081572169));
#20818=CARTESIAN_POINT('Ctrl Pts',(7.58510750685637,0.218175602614713,5.27346801674616));
#20819=CARTESIAN_POINT('Ctrl Pts',(7.58138367708303,0.243704881963377,5.33504721110235));
#20820=CARTESIAN_POINT('Ctrl Pts',(7.58034806292791,0.25,5.36855370076032));
#20821=CARTESIAN_POINT('Ctrl Pts',(7.58034806292791,0.25,5.4));
#20822=CARTESIAN_POINT('',(9.,-3.06161699786838E-17,5.65));
#20823=CARTESIAN_POINT('',(7.4,-3.06161699786838E-17,5.65));
#20824=CARTESIAN_POINT('',(8.98956518577535,0.25,5.4));
#20825=CARTESIAN_POINT('Ctrl Pts',(8.98956518577535,0.25,5.4));
#20826=CARTESIAN_POINT('Ctrl Pts',(8.98956518577535,0.25,5.36859378633187));
#20827=CARTESIAN_POINT('Ctrl Pts',(8.99011104995181,0.24372047740942,5.33510417960069));
#20828=CARTESIAN_POINT('Ctrl Pts',(8.99208145165098,0.218202539734559,5.27351367328886));
#20829=CARTESIAN_POINT('Ctrl Pts',(8.99347740802958,0.198964922639276,5.245411532046));
#20830=CARTESIAN_POINT('Ctrl Pts',(8.99609686518216,0.154588504271054,5.20103511367778));
#20831=CARTESIAN_POINT('Ctrl Pts',(8.99749070376198,0.126486346986081,5.18179746841036));
#20832=CARTESIAN_POINT('Ctrl Pts',(8.99945625936844,0.0648957875009215,
5.15627950921557));
#20833=CARTESIAN_POINT('Ctrl Pts',(9.,0.0314061622633416,5.15));
#20834=CARTESIAN_POINT('Ctrl Pts',(9.,-0.0314061622633416,5.15));
#20835=CARTESIAN_POINT('Ctrl Pts',(8.99945625936844,-0.064895787500922,
5.15627950921557));
#20836=CARTESIAN_POINT('Ctrl Pts',(8.99749070376198,-0.126486346986081,
5.18179746841036));
#20837=CARTESIAN_POINT('Ctrl Pts',(8.99609686518216,-0.154588504271054,
5.20103511367778));
#20838=CARTESIAN_POINT('Ctrl Pts',(8.99347740802958,-0.198964922639276,
5.245411532046));
#20839=CARTESIAN_POINT('Ctrl Pts',(8.99208145165098,-0.218202539734559,
5.27351367328886));
#20840=CARTESIAN_POINT('Ctrl Pts',(8.99011104995181,-0.24372047740942,5.33510417960069));
#20841=CARTESIAN_POINT('Ctrl Pts',(8.98956518577535,-0.25,5.36859378633187));
#20842=CARTESIAN_POINT('Ctrl Pts',(8.98956518577535,-0.25,5.43140621366814));
#20843=CARTESIAN_POINT('Ctrl Pts',(8.99011104995181,-0.24372047740942,5.46489582039931));
#20844=CARTESIAN_POINT('Ctrl Pts',(8.99208145165098,-0.218202539734559,
5.52648632671114));
#20845=CARTESIAN_POINT('Ctrl Pts',(8.99347740802958,-0.198964922639276,
5.554588467954));
#20846=CARTESIAN_POINT('Ctrl Pts',(8.99609686518216,-0.154588504271054,
5.59896488632222));
#20847=CARTESIAN_POINT('Ctrl Pts',(8.99749070376198,-0.126486346986082,
5.61820253158964));
#20848=CARTESIAN_POINT('Ctrl Pts',(8.99945625936844,-0.0648957875009222,
5.64372049078443));
#20849=CARTESIAN_POINT('Ctrl Pts',(9.,-0.0314061622633417,5.65));
#20850=CARTESIAN_POINT('Ctrl Pts',(9.,-4.16333634234434E-17,5.65));
#20851=CARTESIAN_POINT('Ctrl Pts',(9.,-1.38777878078145E-17,5.65));
#20852=CARTESIAN_POINT('Ctrl Pts',(9.,0.0314061622633417,5.65));
#20853=CARTESIAN_POINT('Ctrl Pts',(8.99945625936844,0.0648957875009221,
5.64372049078443));
#20854=CARTESIAN_POINT('Ctrl Pts',(8.99749070376198,0.126486346986081,5.61820253158964));
#20855=CARTESIAN_POINT('Ctrl Pts',(8.99609686518216,0.154588504271054,5.59896488632222));
#20856=CARTESIAN_POINT('Ctrl Pts',(8.99347740802958,0.198964922639276,5.554588467954));
#20857=CARTESIAN_POINT('Ctrl Pts',(8.99208145165098,0.218202539734559,5.52648632671114));
#20858=CARTESIAN_POINT('Ctrl Pts',(8.99011104995181,0.24372047740942,5.46489582039931));
#20859=CARTESIAN_POINT('Ctrl Pts',(8.98956518577535,0.25,5.43140621366814));
#20860=CARTESIAN_POINT('Ctrl Pts',(8.98956518577535,0.25,5.4));
#20861=CARTESIAN_POINT('Origin',(4.05545635173699,-1.94454364826301,8.5));
#20862=CARTESIAN_POINT('',(3.89045635173699,-1.94454364826301,8.5));
#20863=CARTESIAN_POINT('Origin',(4.05545635173699,-1.94454364826301,8.5));
#20864=CARTESIAN_POINT('',(3.89045635173699,-1.94454364826301,9.2));
#20865=CARTESIAN_POINT('',(3.89045635173699,-1.94454364826301,8.5));
#20866=CARTESIAN_POINT('Origin',(4.05545635173699,-1.94454364826301,9.2));
#20867=CARTESIAN_POINT('Origin',(4.05545635173699,-1.94454364826301,8.5));
#20868=CARTESIAN_POINT('Origin',(4.05545635173699,1.94454364826301,8.5));
#20869=CARTESIAN_POINT('',(3.89045635173699,1.94454364826301,8.5));
#20870=CARTESIAN_POINT('Origin',(4.05545635173699,1.94454364826301,8.5));
#20871=CARTESIAN_POINT('',(3.89045635173699,1.94454364826301,9.2));
#20872=CARTESIAN_POINT('',(3.89045635173699,1.94454364826301,8.5));
#20873=CARTESIAN_POINT('Origin',(4.05545635173699,1.94454364826301,9.2));
#20874=CARTESIAN_POINT('Origin',(4.05545635173699,1.94454364826301,8.5));
#20875=CARTESIAN_POINT('Origin',(7.94454364826301,1.94454364826301,8.5));
#20876=CARTESIAN_POINT('',(7.77954364826301,1.94454364826301,8.5));
#20877=CARTESIAN_POINT('Origin',(7.94454364826301,1.94454364826301,8.5));
#20878=CARTESIAN_POINT('',(7.77954364826301,1.94454364826301,9.2));
#20879=CARTESIAN_POINT('',(7.77954364826301,1.94454364826301,8.5));
#20880=CARTESIAN_POINT('Origin',(7.94454364826301,1.94454364826301,9.2));
#20881=CARTESIAN_POINT('Origin',(7.94454364826301,1.94454364826301,8.5));
#20882=CARTESIAN_POINT('Origin',(7.944543648263,-1.94454364826301,8.5));
#20883=CARTESIAN_POINT('',(7.779543648263,-1.94454364826301,8.5));
#20884=CARTESIAN_POINT('Origin',(7.944543648263,-1.94454364826301,8.5));
#20885=CARTESIAN_POINT('',(7.779543648263,-1.94454364826301,9.2));
#20886=CARTESIAN_POINT('',(7.779543648263,-1.94454364826301,8.5));
#20887=CARTESIAN_POINT('Origin',(7.944543648263,-1.94454364826301,9.2));
#20888=CARTESIAN_POINT('Origin',(7.944543648263,-1.94454364826301,8.5));
#20889=CARTESIAN_POINT('Origin',(3.8079689783217,-2.1920310216783,4.));
#20890=CARTESIAN_POINT('',(4.2662001344149,-2.44825203483977,4.6));
#20891=CARTESIAN_POINT('',(4.2662001344149,-2.44825203483977,4.));
#20892=CARTESIAN_POINT('',(4.2662001344149,-2.44825203483977,4.));
#20893=CARTESIAN_POINT('',(3.55174796516023,-1.7337998655851,4.6));
#20894=CARTESIAN_POINT('Origin',(3.8079689783217,-2.1920310216783,4.6));
#20895=CARTESIAN_POINT('',(3.55174796516023,-1.7337998655851,4.));
#20896=CARTESIAN_POINT('',(3.55174796516023,-1.7337998655851,4.));
#20897=CARTESIAN_POINT('Origin',(3.8079689783217,-2.1920310216783,4.));
#20898=CARTESIAN_POINT('Origin',(3.8079689783217,-2.1920310216783,4.6));
#20899=CARTESIAN_POINT('Origin',(6.,0.,4.6));
#20900=CARTESIAN_POINT('Origin',(3.8079689783217,2.1920310216783,4.));
#20901=CARTESIAN_POINT('',(3.55174796516023,1.7337998655851,4.6));
#20902=CARTESIAN_POINT('',(3.55174796516023,1.7337998655851,4.));
#20903=CARTESIAN_POINT('',(3.55174796516023,1.7337998655851,4.));
#20904=CARTESIAN_POINT('',(4.2662001344149,2.44825203483977,4.6));
#20905=CARTESIAN_POINT('Origin',(3.8079689783217,2.1920310216783,4.6));
#20906=CARTESIAN_POINT('',(4.2662001344149,2.44825203483977,4.));
#20907=CARTESIAN_POINT('',(4.2662001344149,2.44825203483977,4.));
#20908=CARTESIAN_POINT('Origin',(3.8079689783217,2.1920310216783,4.));
#20909=CARTESIAN_POINT('Origin',(3.8079689783217,2.1920310216783,4.6));
#20910=CARTESIAN_POINT('Origin',(6.,0.,4.6));
#20911=CARTESIAN_POINT('Origin',(8.1920310216783,2.1920310216783,4.));
#20912=CARTESIAN_POINT('',(7.7337998655851,2.44825203483977,4.6));
#20913=CARTESIAN_POINT('',(7.7337998655851,2.44825203483977,4.));
#20914=CARTESIAN_POINT('',(7.7337998655851,2.44825203483977,4.));
#20915=CARTESIAN_POINT('',(8.44825203483977,1.7337998655851,4.6));
#20916=CARTESIAN_POINT('Origin',(8.1920310216783,2.1920310216783,4.6));
#20917=CARTESIAN_POINT('',(8.44825203483977,1.7337998655851,4.));
#20918=CARTESIAN_POINT('',(8.44825203483977,1.7337998655851,4.));
#20919=CARTESIAN_POINT('Origin',(8.1920310216783,2.1920310216783,4.));
#20920=CARTESIAN_POINT('Origin',(8.1920310216783,2.1920310216783,4.6));
#20921=CARTESIAN_POINT('Origin',(6.,0.,4.6));
#20922=CARTESIAN_POINT('Origin',(8.1920310216783,-2.1920310216783,4.));
#20923=CARTESIAN_POINT('',(8.44825203483977,-1.7337998655851,4.6));
#20924=CARTESIAN_POINT('',(8.44825203483977,-1.7337998655851,4.));
#20925=CARTESIAN_POINT('',(8.44825203483977,-1.7337998655851,4.));
#20926=CARTESIAN_POINT('',(7.7337998655851,-2.44825203483977,4.6));
#20927=CARTESIAN_POINT('Origin',(8.1920310216783,-2.1920310216783,4.6));
#20928=CARTESIAN_POINT('',(7.7337998655851,-2.44825203483977,4.));
#20929=CARTESIAN_POINT('',(7.7337998655851,-2.44825203483977,4.));
#20930=CARTESIAN_POINT('Origin',(8.1920310216783,-2.1920310216783,4.));
#20931=CARTESIAN_POINT('Origin',(8.1920310216783,-2.1920310216783,4.6));
#20932=CARTESIAN_POINT('Origin',(6.,0.,4.6));
#20933=CARTESIAN_POINT('Origin',(8.1920310216783,2.1920310216783,3.1));
#20934=CARTESIAN_POINT('',(7.9170310216783,2.1920310216783,3.2));
#20935=CARTESIAN_POINT('Origin',(8.1920310216783,2.1920310216783,3.2));
#20936=CARTESIAN_POINT('',(7.9170310216783,2.1920310216783,4.));
#20937=CARTESIAN_POINT('',(7.9170310216783,2.1920310216783,3.1));
#20938=CARTESIAN_POINT('Origin',(8.1920310216783,2.1920310216783,4.));
#20939=CARTESIAN_POINT('Origin',(6.,0.,4.));
#20940=CARTESIAN_POINT('',(2.5,-4.28626379701574E-16,4.));
#20941=CARTESIAN_POINT('Origin',(6.,0.,4.));
#20942=CARTESIAN_POINT('',(3.,-3.67394039744206E-16,4.));
#20943=CARTESIAN_POINT('Origin',(6.,0.,4.));
#20944=CARTESIAN_POINT('Origin',(6.,0.,4.));
#20945=CARTESIAN_POINT('Origin',(6.,0.,4.));
#20946=CARTESIAN_POINT('Origin',(6.,0.,4.));
#20947=CARTESIAN_POINT('Origin',(6.,0.,4.));
#20948=CARTESIAN_POINT('',(3.5329689783217,-2.1920310216783,4.));
#20949=CARTESIAN_POINT('Origin',(3.8079689783217,-2.1920310216783,4.));
#20950=CARTESIAN_POINT('',(7.9170310216783,-2.1920310216783,4.));
#20951=CARTESIAN_POINT('Origin',(8.1920310216783,-2.1920310216783,4.));
#20952=CARTESIAN_POINT('',(3.5329689783217,2.1920310216783,4.));
#20953=CARTESIAN_POINT('Origin',(3.8079689783217,2.1920310216783,4.));
#20954=CARTESIAN_POINT('Origin',(8.1920310216783,-2.1920310216783,3.1));
#20955=CARTESIAN_POINT('',(7.9170310216783,-2.1920310216783,3.2));
#20956=CARTESIAN_POINT('Origin',(8.1920310216783,-2.1920310216783,3.2));
#20957=CARTESIAN_POINT('',(7.9170310216783,-2.1920310216783,3.1));
#20958=CARTESIAN_POINT('Origin',(3.8079689783217,-2.1920310216783,3.1));
#20959=CARTESIAN_POINT('',(3.5329689783217,-2.1920310216783,3.2));
#20960=CARTESIAN_POINT('Origin',(3.8079689783217,-2.1920310216783,3.2));
#20961=CARTESIAN_POINT('',(3.5329689783217,-2.1920310216783,3.1));
#20962=CARTESIAN_POINT('Origin',(3.8079689783217,2.1920310216783,3.1));
#20963=CARTESIAN_POINT('',(3.5329689783217,2.1920310216783,3.2));
#20964=CARTESIAN_POINT('Origin',(3.8079689783217,2.1920310216783,3.2));
#20965=CARTESIAN_POINT('',(3.5329689783217,2.1920310216783,3.1));
#20966=CARTESIAN_POINT('Origin',(6.,0.,3.2));
#20967=CARTESIAN_POINT('',(3.,-3.67394039744206E-16,9.2));
#20968=CARTESIAN_POINT('Origin',(6.,0.,9.2));
#20969=CARTESIAN_POINT('',(3.,-3.67394039744206E-16,3.2));
#20970=CARTESIAN_POINT('Origin',(6.,0.,5.8));
#20971=CARTESIAN_POINT('',(3.65,-2.87791997799628E-16,5.8));
#20972=CARTESIAN_POINT('Origin',(6.,0.,5.8));
#20973=CARTESIAN_POINT('',(3.65,2.87791997799628E-16,9.2));
#20974=CARTESIAN_POINT('',(3.65,-2.87791997799628E-16,5.8));
#20975=CARTESIAN_POINT('Origin',(6.,0.,9.2));
#20976=CARTESIAN_POINT('Origin',(6.,0.,5.8));
#20977=CARTESIAN_POINT('',(4.4,-1.95943487863576E-16,5.8));
#20978=CARTESIAN_POINT('Origin',(6.,0.,5.8));
#20979=CARTESIAN_POINT('Origin',(6.,0.,3.2));
#20980=CARTESIAN_POINT('',(2.5,-4.28626379701574E-16,3.2));
#20981=CARTESIAN_POINT('',(2.5,-4.28626379701574E-16,3.2));
#20982=CARTESIAN_POINT('Origin',(6.,0.,3.2));
#20983=CARTESIAN_POINT('Origin',(6.,0.,3.2));
#20984=CARTESIAN_POINT('',(4.4,-1.95943487863576E-16,3.2));
#20985=CARTESIAN_POINT('',(4.4,-1.95943487863576E-16,3.2));
#20986=CARTESIAN_POINT('Origin',(6.,0.,3.2));
#20987=CARTESIAN_POINT('Origin',(6.,0.,9.2));
#20988=CARTESIAN_POINT('Origin',(6.,0.,3.2));
#20989=CARTESIAN_POINT('',(0.,0.,0.));
#20990=CARTESIAN_POINT('Origin',(6.,0.,7.2));
#20991=CARTESIAN_POINT('',(4.3,-2.0818995585505E-16,7.8));
#20992=CARTESIAN_POINT('Origin',(6.,0.,7.8));
#20993=CARTESIAN_POINT('',(4.3,-2.0818995585505E-16,7.2));
#20994=CARTESIAN_POINT('',(4.3,-2.0818995585505E-16,7.2));
#20995=CARTESIAN_POINT('Origin',(6.,0.,7.2));
#20996=CARTESIAN_POINT('Origin',(6.,0.,7.2));
#20997=CARTESIAN_POINT('',(3.66,-2.86567351000481E-16,7.8));
#20998=CARTESIAN_POINT('Origin',(6.,0.,7.8));
#20999=CARTESIAN_POINT('',(3.66,-2.86567351000481E-16,7.2));
#21000=CARTESIAN_POINT('',(3.66,-2.86567351000481E-16,7.2));
#21001=CARTESIAN_POINT('Origin',(6.,0.,7.2));
#21002=CARTESIAN_POINT('Origin',(6.,0.,7.8));
#21003=CARTESIAN_POINT('Origin',(6.,0.,7.2));
#21004=CARTESIAN_POINT('',(0.,0.,0.));
#21005=CARTESIAN_POINT('Origin',(4.05545635173699,-1.94454364826301,9.1));
#21006=CARTESIAN_POINT('',(3.83045635173699,-1.94454364826301,9.2));
#21007=CARTESIAN_POINT('Origin',(4.05545635173699,-1.94454364826301,9.2));
#21008=CARTESIAN_POINT('',(3.83045635173699,-1.94454364826301,9.6));
#21009=CARTESIAN_POINT('',(3.83045635173699,-1.94454364826301,9.1));
#21010=CARTESIAN_POINT('Origin',(4.05545635173699,-1.94454364826301,9.6));
#21011=CARTESIAN_POINT('Origin',(4.05545635173699,1.94454364826301,9.1));
#21012=CARTESIAN_POINT('',(3.83045635173699,1.94454364826301,9.2));
#21013=CARTESIAN_POINT('Origin',(4.05545635173699,1.94454364826301,9.2));
#21014=CARTESIAN_POINT('',(3.83045635173699,1.94454364826301,9.6));
#21015=CARTESIAN_POINT('',(3.83045635173699,1.94454364826301,9.1));
#21016=CARTESIAN_POINT('Origin',(4.05545635173699,1.94454364826301,9.6));
#21017=CARTESIAN_POINT('Origin',(7.94454364826301,1.94454364826301,9.1));
#21018=CARTESIAN_POINT('',(7.71954364826301,1.94454364826301,9.2));
#21019=CARTESIAN_POINT('Origin',(7.94454364826301,1.94454364826301,9.2));
#21020=CARTESIAN_POINT('',(7.71954364826301,1.94454364826301,9.6));
#21021=CARTESIAN_POINT('',(7.71954364826301,1.94454364826301,9.1));
#21022=CARTESIAN_POINT('Origin',(7.94454364826301,1.94454364826301,9.6));
#21023=CARTESIAN_POINT('Origin',(7.944543648263,-1.94454364826301,9.1));
#21024=CARTESIAN_POINT('',(7.719543648263,-1.94454364826301,9.2));
#21025=CARTESIAN_POINT('Origin',(7.944543648263,-1.94454364826301,9.2));
#21026=CARTESIAN_POINT('',(7.719543648263,-1.94454364826301,9.6));
#21027=CARTESIAN_POINT('',(7.719543648263,-1.94454364826301,9.1));
#21028=CARTESIAN_POINT('Origin',(7.944543648263,-1.94454364826301,9.6));
#21029=CARTESIAN_POINT('Origin',(6.,0.,9.2));
#21030=CARTESIAN_POINT('',(4.3,-2.0818995585505E-16,9.6));
#21031=CARTESIAN_POINT('Origin',(6.,0.,9.6));
#21032=CARTESIAN_POINT('',(4.3,-2.0818995585505E-16,9.2));
#21033=CARTESIAN_POINT('',(4.3,-2.0818995585505E-16,9.2));
#21034=CARTESIAN_POINT('Origin',(6.,0.,9.2));
#21035=CARTESIAN_POINT('Origin',(6.,0.,9.2));
#21036=CARTESIAN_POINT('',(3.,-3.67394039744206E-16,9.6));
#21037=CARTESIAN_POINT('Origin',(6.,0.,9.6));
#21038=CARTESIAN_POINT('',(3.,-3.67394039744206E-16,9.2));
#21039=CARTESIAN_POINT('',(3.,-3.67394039744206E-16,9.2));
#21040=CARTESIAN_POINT('Origin',(6.,0.,9.2));
#21041=CARTESIAN_POINT('Origin',(6.,0.,9.6));
#21042=CARTESIAN_POINT('Origin',(6.,0.,9.2));
#21043=CARTESIAN_POINT('',(0.,0.,0.));
#21044=CARTESIAN_POINT('',(0.,0.,0.));
#21045=CARTESIAN_POINT('Origin',(1.5,-1.9,1.7));
#21046=CARTESIAN_POINT('',(1.56403124237433,-1.7,1.7));
#21047=CARTESIAN_POINT('',(1.43596875762567,-1.7,1.7));
#21048=CARTESIAN_POINT('',(0.75,-1.7,1.7));
#21049=CARTESIAN_POINT('Origin',(1.5,-1.9,1.7));
#21050=CARTESIAN_POINT('Origin',(1.5,-1.9,1.7));
#21051=CARTESIAN_POINT('',(1.56403124237433,-1.7,1.75));
#21052=CARTESIAN_POINT('',(1.56403124237433,-1.7,1.7));
#21053=CARTESIAN_POINT('',(1.29,-1.9,1.75));
#21054=CARTESIAN_POINT('Origin',(1.5,-1.9,1.75));
#21055=CARTESIAN_POINT('',(1.29,-1.9,2.4));
#21056=CARTESIAN_POINT('',(1.29,-1.9,1.7));
#21057=CARTESIAN_POINT('Origin',(1.5,-1.9,2.4));
#21058=CARTESIAN_POINT('',(1.43596875762567,-1.7,1.75));
#21059=CARTESIAN_POINT('Origin',(1.5,-1.9,1.75));
#21060=CARTESIAN_POINT('',(1.43596875762567,-1.7,1.7));
#21061=CARTESIAN_POINT('Origin',(-1.5,1.9,1.7));
#21062=CARTESIAN_POINT('',(-1.56403124237433,1.7,1.7));
#21063=CARTESIAN_POINT('',(-1.43596875762567,1.7,1.7));
#21064=CARTESIAN_POINT('',(-0.75,1.7,1.7));
#21065=CARTESIAN_POINT('Origin',(-1.5,1.9,1.7));
#21066=CARTESIAN_POINT('Origin',(-1.5,1.9,1.7));
#21067=CARTESIAN_POINT('',(-1.56403124237433,1.7,1.75));
#21068=CARTESIAN_POINT('',(-1.56403124237433,1.7,1.7));
#21069=CARTESIAN_POINT('',(-1.71,1.9,1.75));
#21070=CARTESIAN_POINT('Origin',(-1.5,1.9,1.75));
#21071=CARTESIAN_POINT('',(-1.71,1.9,2.4));
#21072=CARTESIAN_POINT('',(-1.71,1.9,1.7));
#21073=CARTESIAN_POINT('Origin',(-1.5,1.9,2.4));
#21074=CARTESIAN_POINT('',(-1.43596875762567,1.7,1.75));
#21075=CARTESIAN_POINT('Origin',(-1.5,1.9,1.75));
#21076=CARTESIAN_POINT('',(-1.43596875762567,1.7,1.7));
#21077=CARTESIAN_POINT('Origin',(-1.5,-1.9,1.7));
#21078=CARTESIAN_POINT('',(-1.43596875762567,-1.7,1.7));
#21079=CARTESIAN_POINT('',(-1.56403124237433,-1.7,1.7));
#21080=CARTESIAN_POINT('',(-0.75,-1.7,1.7));
#21081=CARTESIAN_POINT('Origin',(-1.5,-1.9,1.7));
#21082=CARTESIAN_POINT('Origin',(-1.5,-1.9,1.7));
#21083=CARTESIAN_POINT('',(-1.43596875762567,-1.7,1.75));
#21084=CARTESIAN_POINT('',(-1.43596875762567,-1.7,1.7));
#21085=CARTESIAN_POINT('',(-1.71,-1.9,1.75));
#21086=CARTESIAN_POINT('Origin',(-1.5,-1.9,1.75));
#21087=CARTESIAN_POINT('',(-1.71,-1.9,2.4));
#21088=CARTESIAN_POINT('',(-1.71,-1.9,1.7));
#21089=CARTESIAN_POINT('Origin',(-1.5,-1.9,2.4));
#21090=CARTESIAN_POINT('',(-1.56403124237433,-1.7,1.75));
#21091=CARTESIAN_POINT('Origin',(-1.5,-1.9,1.75));
#21092=CARTESIAN_POINT('',(-1.56403124237433,-1.7,1.7));
#21093=CARTESIAN_POINT('Origin',(1.5,1.9,1.7));
#21094=CARTESIAN_POINT('',(1.43596875762567,1.7,1.7));
#21095=CARTESIAN_POINT('',(1.56403124237433,1.7,1.7));
#21096=CARTESIAN_POINT('',(0.75,1.7,1.7));
#21097=CARTESIAN_POINT('Origin',(1.5,1.9,1.7));
#21098=CARTESIAN_POINT('Origin',(1.5,1.9,1.7));
#21099=CARTESIAN_POINT('',(1.43596875762567,1.7,1.75));
#21100=CARTESIAN_POINT('',(1.43596875762567,1.7,1.7));
#21101=CARTESIAN_POINT('',(1.29,1.9,1.75));
#21102=CARTESIAN_POINT('Origin',(1.5,1.9,1.75));
#21103=CARTESIAN_POINT('',(1.29,1.9,2.4));
#21104=CARTESIAN_POINT('',(1.29,1.9,1.7));
#21105=CARTESIAN_POINT('Origin',(1.5,1.9,2.4));
#21106=CARTESIAN_POINT('',(1.56403124237433,1.7,1.75));
#21107=CARTESIAN_POINT('Origin',(1.5,1.9,1.75));
#21108=CARTESIAN_POINT('',(1.56403124237433,1.7,1.7));
#21109=CARTESIAN_POINT('Origin',(0.,-1.7,1.75));
#21110=CARTESIAN_POINT('',(0.,-1.7,1.75));
#21111=CARTESIAN_POINT('',(-1.97,-1.7,1.75));
#21112=CARTESIAN_POINT('',(0.,-1.7,1.75));
#21113=CARTESIAN_POINT('',(-1.97,-1.7,0.43));
#21114=CARTESIAN_POINT('',(-1.97,-1.7,1.75));
#21115=CARTESIAN_POINT('',(1.97,-1.7,0.43));
#21116=CARTESIAN_POINT('',(0.,-1.7,0.43));
#21117=CARTESIAN_POINT('',(1.97,-1.7,1.75));
#21118=CARTESIAN_POINT('',(1.97,-1.7,1.75));
#21119=CARTESIAN_POINT('',(0.,-1.7,1.75));
#21120=CARTESIAN_POINT('Origin',(0.,1.7,0.43));
#21121=CARTESIAN_POINT('',(0.,1.7,1.75));
#21122=CARTESIAN_POINT('',(1.97,1.7,1.75));
#21123=CARTESIAN_POINT('',(0.,1.7,1.75));
#21124=CARTESIAN_POINT('',(1.97,1.7,0.43));
#21125=CARTESIAN_POINT('',(1.97,1.7,0.43));
#21126=CARTESIAN_POINT('',(-1.97,1.7,0.43));
#21127=CARTESIAN_POINT('',(0.,1.7,0.43));
#21128=CARTESIAN_POINT('',(-1.97,1.7,1.75));
#21129=CARTESIAN_POINT('',(-1.97,1.7,0.43));
#21130=CARTESIAN_POINT('',(0.,1.7,1.75));
#21131=CARTESIAN_POINT('Origin',(-1.97,0.,1.415));
#21132=CARTESIAN_POINT('',(-1.97,-2.35,1.75));
#21133=CARTESIAN_POINT('',(-1.97,-2.35,1.75));
#21134=CARTESIAN_POINT('',(-1.97,-2.35,2.4));
#21135=CARTESIAN_POINT('',(-1.97,-2.35,2.4));
#21136=CARTESIAN_POINT('',(-1.97,2.35,2.4));
#21137=CARTESIAN_POINT('',(-1.97,2.35,2.4));
#21138=CARTESIAN_POINT('',(-1.97,2.35,1.75));
#21139=CARTESIAN_POINT('',(-1.97,2.35,1.75));
#21140=CARTESIAN_POINT('',(-1.97,1.7,1.75));
#21141=CARTESIAN_POINT('',(-1.97,0.78,0.43));
#21142=CARTESIAN_POINT('',(-1.97,0.78,0.43));
#21143=CARTESIAN_POINT('',(-1.97,0.78,1.55));
#21144=CARTESIAN_POINT('',(-1.97,0.78,1.55));
#21145=CARTESIAN_POINT('',(-1.97,-0.78,1.55));
#21146=CARTESIAN_POINT('',(-1.97,-0.78,1.55));
#21147=CARTESIAN_POINT('',(-1.97,-0.78,0.43));
#21148=CARTESIAN_POINT('',(-1.97,-0.78,0.43));
#21149=CARTESIAN_POINT('',(-1.97,-1.7,0.43));
#21150=CARTESIAN_POINT('Origin',(0.,-2.35,1.75));
#21151=CARTESIAN_POINT('',(1.97,-2.35,1.75));
#21152=CARTESIAN_POINT('',(1.97,-2.35,1.75));
#21153=CARTESIAN_POINT('',(0.,-2.35,1.75));
#21154=CARTESIAN_POINT('Origin',(0.,-2.35,2.4));
#21155=CARTESIAN_POINT('',(1.97,-2.35,2.4));
#21156=CARTESIAN_POINT('',(1.97,-2.35,2.4));
#21157=CARTESIAN_POINT('',(0.,-2.35,2.4));
#21158=CARTESIAN_POINT('Origin',(0.,2.35,2.4));
#21159=CARTESIAN_POINT('',(1.97,2.35,2.4));
#21160=CARTESIAN_POINT('',(1.97,2.35,2.4));
#21161=CARTESIAN_POINT('',(0.,2.35,2.4));
#21162=CARTESIAN_POINT('Origin',(0.,2.35,1.75));
#21163=CARTESIAN_POINT('',(1.97,2.35,1.75));
#21164=CARTESIAN_POINT('',(1.97,2.35,1.75));
#21165=CARTESIAN_POINT('',(0.,2.35,1.75));
#21166=CARTESIAN_POINT('Origin',(0.,1.7,1.75));
#21167=CARTESIAN_POINT('',(1.97,1.7,1.75));
#21168=CARTESIAN_POINT('Origin',(0.,0.78,0.43));
#21169=CARTESIAN_POINT('',(1.97,0.78,0.43));
#21170=CARTESIAN_POINT('',(1.97,0.78,0.43));
#21171=CARTESIAN_POINT('',(0.,0.78,0.43));
#21172=CARTESIAN_POINT('Origin',(0.,0.78,1.55));
#21173=CARTESIAN_POINT('',(1.97,0.78,1.55));
#21174=CARTESIAN_POINT('',(1.97,0.78,1.55));
#21175=CARTESIAN_POINT('',(0.,0.78,1.55));
#21176=CARTESIAN_POINT('Origin',(0.,-0.78,1.55));
#21177=CARTESIAN_POINT('',(1.97,-0.78,1.55));
#21178=CARTESIAN_POINT('',(1.97,-0.78,1.55));
#21179=CARTESIAN_POINT('',(0.,-0.78,1.55));
#21180=CARTESIAN_POINT('Origin',(0.,-0.78,0.43));
#21181=CARTESIAN_POINT('',(1.97,-0.78,0.43));
#21182=CARTESIAN_POINT('',(1.97,-0.78,0.43));
#21183=CARTESIAN_POINT('',(0.,-0.78,0.43));
#21184=CARTESIAN_POINT('Origin',(0.,-1.7,0.43));
#21185=CARTESIAN_POINT('',(1.97,-1.7,0.43));
#21186=CARTESIAN_POINT('Origin',(1.97,0.,1.415));
#21187=CARTESIAN_POINT('',(0.,0.,0.));
#21188=CARTESIAN_POINT('Origin',(1.97,1.7,2.3));
#21189=CARTESIAN_POINT('',(1.97,1.7,2.3));
#21190=CARTESIAN_POINT('',(1.97,-1.7,2.3));
#21191=CARTESIAN_POINT('',(1.97,1.7,2.3));
#21192=CARTESIAN_POINT('',(3.07,-1.7,2.3));
#21193=CARTESIAN_POINT('',(1.97,-1.7,2.3));
#21194=CARTESIAN_POINT('',(3.07,1.7,2.3));
#21195=CARTESIAN_POINT('',(3.07,1.7,2.3));
#21196=CARTESIAN_POINT('',(1.97,1.7,2.3));
#21197=CARTESIAN_POINT('Origin',(1.97,1.7,0.46));
#21198=CARTESIAN_POINT('',(1.97,1.7,0.46));
#21199=CARTESIAN_POINT('',(1.97,1.7,0.46));
#21200=CARTESIAN_POINT('',(3.07,1.7,0.46));
#21201=CARTESIAN_POINT('',(3.07,1.7,0.46));
#21202=CARTESIAN_POINT('',(1.97,1.7,0.46));
#21203=CARTESIAN_POINT('Origin',(1.97,0.78,0.46));
#21204=CARTESIAN_POINT('',(1.97,0.78,0.46));
#21205=CARTESIAN_POINT('',(1.97,0.78,0.46));
#21206=CARTESIAN_POINT('',(3.07,0.78,0.46));
#21207=CARTESIAN_POINT('',(3.07,0.78,0.46));
#21208=CARTESIAN_POINT('',(1.97,0.78,0.46));
#21209=CARTESIAN_POINT('Origin',(1.97,0.78,1.55));
#21210=CARTESIAN_POINT('',(1.97,0.78,1.55));
#21211=CARTESIAN_POINT('',(1.97,0.78,1.55));
#21212=CARTESIAN_POINT('',(3.07,0.78,1.55));
#21213=CARTESIAN_POINT('',(3.07,0.78,1.55));
#21214=CARTESIAN_POINT('',(1.97,0.78,1.55));
#21215=CARTESIAN_POINT('Origin',(1.97,-0.78,1.55));
#21216=CARTESIAN_POINT('',(1.97,-0.78,1.55));
#21217=CARTESIAN_POINT('',(1.97,-0.78,1.55));
#21218=CARTESIAN_POINT('',(3.07,-0.78,1.55));
#21219=CARTESIAN_POINT('',(3.07,-0.78,1.55));
#21220=CARTESIAN_POINT('',(1.97,-0.78,1.55));
#21221=CARTESIAN_POINT('Origin',(1.97,-0.78,0.46));
#21222=CARTESIAN_POINT('',(1.97,-0.78,0.46));
#21223=CARTESIAN_POINT('',(1.97,-0.78,0.46));
#21224=CARTESIAN_POINT('',(3.07,-0.78,0.46));
#21225=CARTESIAN_POINT('',(3.07,-0.78,0.46));
#21226=CARTESIAN_POINT('',(1.97,-0.78,0.46));
#21227=CARTESIAN_POINT('Origin',(1.97,-1.7,0.46));
#21228=CARTESIAN_POINT('',(1.97,-1.7,0.46));
#21229=CARTESIAN_POINT('',(1.97,-1.7,0.46));
#21230=CARTESIAN_POINT('',(3.07,-1.7,0.46));
#21231=CARTESIAN_POINT('',(3.07,-1.7,0.46));
#21232=CARTESIAN_POINT('',(1.97,-1.7,0.46));
#21233=CARTESIAN_POINT('Origin',(1.97,-1.7,2.3));
#21234=CARTESIAN_POINT('',(1.97,-1.7,2.3));
#21235=CARTESIAN_POINT('',(3.07,-1.7,2.3));
#21236=CARTESIAN_POINT('Origin',(3.07,0.,1.38));
#21237=CARTESIAN_POINT('Origin',(1.97,0.,1.38));
#21238=CARTESIAN_POINT('',(0.,0.,0.));
#21239=CARTESIAN_POINT('Origin',(-1.97,-0.78,0.46));
#21240=CARTESIAN_POINT('',(-1.97,-1.7,0.46));
#21241=CARTESIAN_POINT('',(-1.97,-0.78,0.46));
#21242=CARTESIAN_POINT('',(-1.97,-1.7,0.46));
#21243=CARTESIAN_POINT('',(-3.07,-1.7,0.46));
#21244=CARTESIAN_POINT('',(-1.97,-1.7,0.46));
#21245=CARTESIAN_POINT('',(-3.07,-0.78,0.46));
#21246=CARTESIAN_POINT('',(-3.07,-1.7,0.46));
#21247=CARTESIAN_POINT('',(-1.97,-0.78,0.46));
#21248=CARTESIAN_POINT('Origin',(-1.97,-0.78,1.55));
#21249=CARTESIAN_POINT('',(-1.97,-0.78,1.55));
#21250=CARTESIAN_POINT('',(-1.97,-0.78,0.46));
#21251=CARTESIAN_POINT('',(-3.07,-0.78,1.55));
#21252=CARTESIAN_POINT('',(-3.07,-0.78,0.46));
#21253=CARTESIAN_POINT('',(-1.97,-0.78,1.55));
#21254=CARTESIAN_POINT('Origin',(-1.97,0.78,1.55));
#21255=CARTESIAN_POINT('',(-1.97,0.78,1.55));
#21256=CARTESIAN_POINT('',(-1.97,-0.78,1.55));
#21257=CARTESIAN_POINT('',(-3.07,0.78,1.55));
#21258=CARTESIAN_POINT('',(-3.07,-0.78,1.55));
#21259=CARTESIAN_POINT('',(-1.97,0.78,1.55));
#21260=CARTESIAN_POINT('Origin',(-1.97,0.78,0.46));
#21261=CARTESIAN_POINT('',(-1.97,0.78,0.46));
#21262=CARTESIAN_POINT('',(-1.97,0.78,1.55));
#21263=CARTESIAN_POINT('',(-3.07,0.78,0.46));
#21264=CARTESIAN_POINT('',(-3.07,0.78,1.55));
#21265=CARTESIAN_POINT('',(-1.97,0.78,0.46));
#21266=CARTESIAN_POINT('Origin',(-1.97,1.7,0.46));
#21267=CARTESIAN_POINT('',(-1.97,1.7,0.46));
#21268=CARTESIAN_POINT('',(-1.97,0.78,0.46));
#21269=CARTESIAN_POINT('',(-3.07,1.7,0.46));
#21270=CARTESIAN_POINT('',(-3.07,0.78,0.46));
#21271=CARTESIAN_POINT('',(-1.97,1.7,0.46));
#21272=CARTESIAN_POINT('Origin',(-1.97,1.7,2.3));
#21273=CARTESIAN_POINT('',(-1.97,1.7,2.3));
#21274=CARTESIAN_POINT('',(-1.97,1.7,0.46));
#21275=CARTESIAN_POINT('',(-3.07,1.7,2.3));
#21276=CARTESIAN_POINT('',(-3.07,1.7,0.46));
#21277=CARTESIAN_POINT('',(-1.97,1.7,2.3));
#21278=CARTESIAN_POINT('Origin',(-1.97,-1.7,2.3));
#21279=CARTESIAN_POINT('',(-1.97,-1.7,2.3));
#21280=CARTESIAN_POINT('',(-1.97,1.7,2.3));
#21281=CARTESIAN_POINT('',(-3.07,-1.7,2.3));
#21282=CARTESIAN_POINT('',(-3.07,1.7,2.3));
#21283=CARTESIAN_POINT('',(-1.97,-1.7,2.3));
#21284=CARTESIAN_POINT('Origin',(-1.97,-1.7,0.46));
#21285=CARTESIAN_POINT('',(-1.97,-1.7,2.3));
#21286=CARTESIAN_POINT('',(-3.07,-1.7,2.3));
#21287=CARTESIAN_POINT('Origin',(-1.97,0.,1.38));
#21288=CARTESIAN_POINT('Origin',(-3.07,0.,1.38));
#21289=CARTESIAN_POINT('',(0.,0.,0.));
#21290=CARTESIAN_POINT('',(0.,0.,0.));
#21291=CARTESIAN_POINT('',(0.,0.,0.));
#21292=CARTESIAN_POINT('',(0.,0.,0.));
#21293=CARTESIAN_POINT('Origin',(0.0577350269189626,0.,-0.1));
#21294=CARTESIAN_POINT('',(0.0577350269189626,0.,-0.1));
#21295=CARTESIAN_POINT('',(0.115470053837925,0.,0.));
#21296=CARTESIAN_POINT('',(0.0934187836487032,0.,-0.0381939203391614));
#21297=CARTESIAN_POINT('',(0.0577350269189626,-0.2,-0.1));
#21298=CARTESIAN_POINT('',(0.0577350269189626,0.,-0.1));
#21299=CARTESIAN_POINT('',(0.115470053837925,-0.2,0.));
#21300=CARTESIAN_POINT('',(0.115470053837925,-0.2,0.));
#21301=CARTESIAN_POINT('',(0.115470053837925,0.,0.));
#21302=CARTESIAN_POINT('Origin',(-0.0577350269189626,0.,-0.1));
#21303=CARTESIAN_POINT('',(-0.0577350269189626,0.,-0.1));
#21304=CARTESIAN_POINT('',(0.0561324865405187,0.,-0.1));
#21305=CARTESIAN_POINT('',(-0.0577350269189626,-0.2,-0.1));
#21306=CARTESIAN_POINT('',(-0.0577350269189626,0.,-0.1));
#21307=CARTESIAN_POINT('',(0.0577350269189626,-0.2,-0.1));
#21308=CARTESIAN_POINT('Origin',(-0.115470053837925,0.,-1.38777878078145E-17));
#21309=CARTESIAN_POINT('',(-0.115470053837925,0.,-1.41410031829988E-17));
#21310=CARTESIAN_POINT('',(-0.0797862971081845,0.,-0.0618060796608387));
#21311=CARTESIAN_POINT('',(-0.115470053837925,-0.2,-1.38777878078145E-17));
#21312=CARTESIAN_POINT('',(-0.115470053837925,0.,-1.41410031829988E-17));
#21313=CARTESIAN_POINT('',(-0.0577350269189626,-0.2,-0.1));
#21314=CARTESIAN_POINT('Origin',(-0.0577350269189626,0.,0.1));
#21315=CARTESIAN_POINT('',(-0.0577350269189626,0.,0.1));
#21316=CARTESIAN_POINT('',(-0.0509187836487033,0.,0.111806079660839));
#21317=CARTESIAN_POINT('',(-0.0577350269189626,-0.2,0.1));
#21318=CARTESIAN_POINT('',(-0.0577350269189626,0.,0.1));
#21319=CARTESIAN_POINT('',(-0.115470053837925,-0.2,-1.41410031829988E-17));
#21320=CARTESIAN_POINT('Origin',(0.0577350269189626,0.,0.1));
#21321=CARTESIAN_POINT('',(0.0577350269189626,0.,0.1));
#21322=CARTESIAN_POINT('',(0.113867513459481,0.,0.1));
#21323=CARTESIAN_POINT('',(0.0577350269189626,-0.2,0.1));
#21324=CARTESIAN_POINT('',(0.0577350269189626,0.,0.1));
#21325=CARTESIAN_POINT('',(-0.0577350269189626,-0.2,0.1));
#21326=CARTESIAN_POINT('Origin',(0.115470053837925,0.,0.));
#21327=CARTESIAN_POINT('',(0.122286297108185,0.,-0.0118060796608386));
#21328=CARTESIAN_POINT('',(0.0577350269189626,-0.2,0.1));
#21329=CARTESIAN_POINT('Origin',(0.,-0.2,0.));
#21330=CARTESIAN_POINT('Origin',(0.17,0.,0.));
#21331=CARTESIAN_POINT('',(-0.17,-8.67361737988404E-18,-2.0818995585505E-17));
#21332=CARTESIAN_POINT('Origin',(0.,0.,0.));
#21333=CARTESIAN_POINT('Origin',(0.,-0.015,0.));
#21334=CARTESIAN_POINT('',(-0.1954,-0.0254,-2.39295984553393E-17));
#21335=CARTESIAN_POINT('Origin',(0.,-0.0254,0.));
#21336=CARTESIAN_POINT('',(-0.185,-0.015,-2.2655965784226E-17));
#21337=CARTESIAN_POINT('Origin',(0.,-0.2775,0.));
#21338=CARTESIAN_POINT('',(-0.1954,-0.5296,2.39295984553393E-17));
#21339=CARTESIAN_POINT('Origin',(0.,-0.5296,0.));
#21340=CARTESIAN_POINT('',(-0.1954,-0.2775,-2.39295984553393E-17));
#21341=CARTESIAN_POINT('Origin',(0.,-0.5625,0.));
#21342=CARTESIAN_POINT('',(-0.125,-0.6,-1.53080849893419E-17));
#21343=CARTESIAN_POINT('Origin',(0.,-0.6,0.));
#21344=CARTESIAN_POINT('',(-0.1625,-0.5625,-1.99005104861445E-17));
#21345=CARTESIAN_POINT('Origin',(0.,-0.6,0.));
#21346=CARTESIAN_POINT('',(0.,0.,0.));
#21347=CARTESIAN_POINT('Origin',(0.115470053837925,-0.5,-0.2));
#21348=CARTESIAN_POINT('',(0.23094010767585,-0.5,0.));
#21349=CARTESIAN_POINT('',(0.115470053837925,-0.5,-0.2));
#21350=CARTESIAN_POINT('',(0.23094010767585,-0.5,0.));
#21351=CARTESIAN_POINT('',(0.115470053837925,-0.8,-0.2));
#21352=CARTESIAN_POINT('',(0.115470053837925,-0.5,-0.2));
#21353=CARTESIAN_POINT('',(0.23094010767585,-0.8,0.));
#21354=CARTESIAN_POINT('',(0.23094010767585,-0.8,0.));
#21355=CARTESIAN_POINT('',(0.23094010767585,-0.5,0.));
#21356=CARTESIAN_POINT('Origin',(-0.115470053837925,-0.5,-0.2));
#21357=CARTESIAN_POINT('',(-0.115470053837925,-0.5,-0.2));
#21358=CARTESIAN_POINT('',(0.115470053837925,-0.5,-0.2));
#21359=CARTESIAN_POINT('',(-0.115470053837925,-0.8,-0.2));
#21360=CARTESIAN_POINT('',(-0.115470053837925,-0.5,-0.2));
#21361=CARTESIAN_POINT('',(0.115470053837925,-0.8,-0.2));
#21362=CARTESIAN_POINT('Origin',(-0.23094010767585,-0.5,-2.77555756156289E-17));
#21363=CARTESIAN_POINT('',(-0.23094010767585,-0.5,-2.82820063659975E-17));
#21364=CARTESIAN_POINT('',(-0.115470053837925,-0.5,-0.2));
#21365=CARTESIAN_POINT('',(-0.23094010767585,-0.8,-2.77555756156289E-17));
#21366=CARTESIAN_POINT('',(-0.23094010767585,-0.5,-2.82820063659975E-17));
#21367=CARTESIAN_POINT('',(-0.115470053837925,-0.8,-0.2));
#21368=CARTESIAN_POINT('Origin',(-0.115470053837925,-0.5,0.2));
#21369=CARTESIAN_POINT('',(-0.115470053837925,-0.5,0.2));
#21370=CARTESIAN_POINT('',(-0.23094010767585,-0.5,-2.82820063659975E-17));
#21371=CARTESIAN_POINT('',(-0.115470053837925,-0.8,0.2));
#21372=CARTESIAN_POINT('',(-0.115470053837925,-0.5,0.2));
#21373=CARTESIAN_POINT('',(-0.23094010767585,-0.8,-2.82820063659975E-17));
#21374=CARTESIAN_POINT('Origin',(0.115470053837925,-0.5,0.2));
#21375=CARTESIAN_POINT('',(0.115470053837925,-0.5,0.2));
#21376=CARTESIAN_POINT('',(-0.115470053837925,-0.5,0.2));
#21377=CARTESIAN_POINT('',(0.115470053837925,-0.8,0.2));
#21378=CARTESIAN_POINT('',(0.115470053837925,-0.5,0.2));
#21379=CARTESIAN_POINT('',(-0.115470053837925,-0.8,0.2));
#21380=CARTESIAN_POINT('Origin',(0.23094010767585,-0.5,0.));
#21381=CARTESIAN_POINT('',(0.115470053837925,-0.5,0.2));
#21382=CARTESIAN_POINT('',(0.115470053837925,-0.8,0.2));
#21383=CARTESIAN_POINT('Origin',(0.,-0.5,0.));
#21384=CARTESIAN_POINT('Origin',(0.,-0.8,0.));
#21385=CARTESIAN_POINT('Origin',(0.,-1.4,0.));
#21386=CARTESIAN_POINT('',(-0.24505,-1.4,3.00099698131059E-17));
#21387=CARTESIAN_POINT('Origin',(0.,-1.4,0.));
#21388=CARTESIAN_POINT('Origin',(0.375,0.5,0.));
#21389=CARTESIAN_POINT('',(-0.375,0.5,-4.59242549680257E-17));
#21390=CARTESIAN_POINT('Origin',(0.,0.5,0.));
#21391=CARTESIAN_POINT('Origin',(0.,0.475,0.));
#21392=CARTESIAN_POINT('',(-0.425,0.45,-5.20474889637625E-17));
#21393=CARTESIAN_POINT('Origin',(0.,0.45,0.));
#21394=CARTESIAN_POINT('',(-0.4,0.475,-4.89858719658941E-17));
#21395=CARTESIAN_POINT('Origin',(0.,0.24,0.));
#21396=CARTESIAN_POINT('',(-0.425,0.0299999999999998,-5.20474889637625E-17));
#21397=CARTESIAN_POINT('Origin',(0.,0.0299999999999998,0.));
#21398=CARTESIAN_POINT('',(-0.425,0.24,-5.20474889637625E-17));
#21399=CARTESIAN_POINT('Origin',(0.,0.0150000000000001,0.));
#21400=CARTESIAN_POINT('',(-0.395,4.85722573273506E-17,-4.83735485663204E-17));
#21401=CARTESIAN_POINT('Origin',(0.,0.,0.));
#21402=CARTESIAN_POINT('',(-0.41,0.0150000000000001,-5.02105187650415E-17));
#21403=CARTESIAN_POINT('Origin',(0.27,0.,0.));
#21404=CARTESIAN_POINT('',(-0.27,0.,-3.30654635769785E-17));
#21405=CARTESIAN_POINT('Origin',(0.,0.,0.));
#21406=CARTESIAN_POINT('Origin',(0.,-0.02,0.));
#21407=CARTESIAN_POINT('',(-0.24505,-0.0498999999999999,3.00099698131059E-17));
#21408=CARTESIAN_POINT('Origin',(0.,-0.0498999999999999,0.));
#21409=CARTESIAN_POINT('',(-0.26,-0.02,-3.18408167778312E-17));
#21410=CARTESIAN_POINT('Origin',(0.,-0.995,0.));
#21411=CARTESIAN_POINT('',(-0.24505,-0.995,-3.00099698131059E-17));
#21412=CARTESIAN_POINT('',(0.,0.,0.));
#21413=CARTESIAN_POINT('',(0.,0.,0.));
#21414=CARTESIAN_POINT('Origin',(0.,0.,0.));
#21415=CARTESIAN_POINT('',(-1.63531,-0.410863395882378,-2.00267715711366E-16));
#21416=CARTESIAN_POINT('',(-2.00267715711366E-16,-0.410863395882378,1.63531));
#21417=CARTESIAN_POINT('Origin',(0.,-0.410863395882378,0.));
#21418=CARTESIAN_POINT('Origin',(0.,-0.410863395882378,0.));
#21419=CARTESIAN_POINT('',(-2.00267715711366E-16,0.410863395882378,1.63531));
#21420=CARTESIAN_POINT('Origin',(-2.05128338857182E-16,0.,1.675));
#21421=CARTESIAN_POINT('',(-1.63531,0.410863395882378,2.00267715711366E-16));
#21422=CARTESIAN_POINT('Origin',(0.,0.410863395882378,0.));
#21423=CARTESIAN_POINT('Origin',(0.,0.410863395882378,0.));
#21424=CARTESIAN_POINT('Origin',(0.,0.,0.));
#21425=CARTESIAN_POINT('',(-1.63531,0.7,-2.00267715711366E-16));
#21426=CARTESIAN_POINT('',(-1.63531,0.,-2.00267715711366E-16));
#21427=CARTESIAN_POINT('Origin',(0.,0.7,0.));
#21428=CARTESIAN_POINT('Origin',(0.,0.,0.));
#21429=CARTESIAN_POINT('',(-1.,-0.6,-1.22464679914735E-16));
#21430=CARTESIAN_POINT('Origin',(0.,-0.6,0.));
#21431=CARTESIAN_POINT('',(-1.,0.6,-1.22464679914735E-16));
#21432=CARTESIAN_POINT('',(-1.,0.,-1.22464679914735E-16));
#21433=CARTESIAN_POINT('Origin',(0.,0.6,0.));
#21434=CARTESIAN_POINT('Origin',(0.,0.65,0.));
#21435=CARTESIAN_POINT('',(-1.1,0.7,-1.34711147906209E-16));
#21436=CARTESIAN_POINT('',(-1.05,0.65,-1.28587913910472E-16));
#21437=CARTESIAN_POINT('Origin',(0.,0.7,0.));
#21438=CARTESIAN_POINT('Origin',(1.63531,0.7,0.));
#21439=CARTESIAN_POINT('Origin',(0.,0.,0.));
#21440=CARTESIAN_POINT('',(-1.63531,-0.7,-2.00267715711366E-16));
#21441=CARTESIAN_POINT('Origin',(0.,-0.7,0.));
#21442=CARTESIAN_POINT('',(-1.63531,0.,-2.00267715711366E-16));
#21443=CARTESIAN_POINT('Origin',(1.1,-0.7,0.));
#21444=CARTESIAN_POINT('',(-1.1,-0.7,-1.34711147906209E-16));
#21445=CARTESIAN_POINT('Origin',(0.,-0.7,0.));
#21446=CARTESIAN_POINT('Origin',(0.,-0.65,0.));
#21447=CARTESIAN_POINT('',(-1.05,-0.65,-1.28587913910472E-16));
#21448=CARTESIAN_POINT('',(0.,0.,0.));
#21449=CARTESIAN_POINT('Origin',(0.,0.,0.));
#21450=CARTESIAN_POINT('',(-1.71469,0.410863395882378,-2.09988962002998E-16));
#21451=CARTESIAN_POINT('',(-2.09988962002998E-16,0.410863395882378,1.71469));
#21452=CARTESIAN_POINT('Origin',(0.,0.410863395882378,0.));
#21453=CARTESIAN_POINT('Origin',(0.,0.410863395882378,0.));
#21454=CARTESIAN_POINT('',(-2.09988962002998E-16,-0.410863395882378,1.71469));
#21455=CARTESIAN_POINT('Origin',(-2.05128338857182E-16,0.,1.675));
#21456=CARTESIAN_POINT('',(-1.71469,-0.410863395882378,2.09988962002998E-16));
#21457=CARTESIAN_POINT('Origin',(0.,-0.410863395882378,0.));
#21458=CARTESIAN_POINT('Origin',(0.,-0.410863395882378,0.));
#21459=CARTESIAN_POINT('Origin',(0.,0.,0.));
#21460=CARTESIAN_POINT('',(-1.71469,-0.7,-2.09988962002998E-16));
#21461=CARTESIAN_POINT('Origin',(0.,-0.7,0.));
#21462=CARTESIAN_POINT('',(-1.71469,0.,-2.09988962002998E-16));
#21463=CARTESIAN_POINT('Origin',(2.25,0.7,0.));
#21464=CARTESIAN_POINT('',(-2.25,0.7,-2.75545529808154E-16));
#21465=CARTESIAN_POINT('Origin',(0.,0.7,0.));
#21466=CARTESIAN_POINT('',(-1.71469,0.7,-2.09988962002998E-16));
#21467=CARTESIAN_POINT('Origin',(0.,0.7,0.));
#21468=CARTESIAN_POINT('Origin',(0.,0.65,0.));
#21469=CARTESIAN_POINT('',(-2.35,0.6,-2.87791997799628E-16));
#21470=CARTESIAN_POINT('Origin',(0.,0.6,0.));
#21471=CARTESIAN_POINT('',(-2.3,0.65,-2.81668763803891E-16));
#21472=CARTESIAN_POINT('Origin',(0.,0.,0.));
#21473=CARTESIAN_POINT('',(-2.35,-0.6,-2.87791997799628E-16));
#21474=CARTESIAN_POINT('Origin',(0.,-0.6,0.));
#21475=CARTESIAN_POINT('',(-2.35,0.,-2.87791997799628E-16));
#21476=CARTESIAN_POINT('Origin',(0.,-0.65,0.));
#21477=CARTESIAN_POINT('',(-2.25,-0.7,-2.75545529808154E-16));
#21478=CARTESIAN_POINT('Origin',(0.,-0.7,0.));
#21479=CARTESIAN_POINT('',(-2.3,-0.65,-2.81668763803891E-16));
#21480=CARTESIAN_POINT('Origin',(1.71469,-0.7,0.));
#21481=CARTESIAN_POINT('Origin',(0.,0.,0.));
#21482=CARTESIAN_POINT('',(-1.71469,0.,-2.09988962002998E-16));
#21483=CARTESIAN_POINT('',(0.,0.,0.));
#21484=CARTESIAN_POINT('Origin',(1.675,0.,0.));
#21485=CARTESIAN_POINT('',(1.675,-2.97627328869245E-33,0.3969));
#21486=CARTESIAN_POINT('',(1.675,-2.97627328869245E-33,-0.3969));
#21487=CARTESIAN_POINT('Origin',(1.675,0.,0.));
#21488=CARTESIAN_POINT('Origin',(1.18440385848747,0.,-1.18440385848747));
#21489=CARTESIAN_POINT('',(1.46505453994041,3.1867025333467E-33,-0.903753177034526));
#21490=CARTESIAN_POINT('',(0.903753177034527,-9.13924911073161E-33,-1.46505453994041));
#21491=CARTESIAN_POINT('Origin',(1.18440385848747,0.,-1.18440385848747));
#21492=CARTESIAN_POINT('Origin',(1.02564169428591E-16,0.,-1.675));
#21493=CARTESIAN_POINT('',(0.3969,-2.97627328869246E-33,-1.675));
#21494=CARTESIAN_POINT('',(-0.3969,-2.97627328869245E-33,-1.675));
#21495=CARTESIAN_POINT('Origin',(1.02564169428591E-16,0.,-1.675));
#21496=CARTESIAN_POINT('Origin',(-1.18440385848747,0.,-1.18440385848747));
#21497=CARTESIAN_POINT('',(-0.903753177034526,3.1867025333467E-33,-1.46505453994041));
#21498=CARTESIAN_POINT('',(-1.46505453994041,-9.13924911073161E-33,-0.903753177034527));
#21499=CARTESIAN_POINT('Origin',(-1.18440385848747,0.,-1.18440385848747));
#21500=CARTESIAN_POINT('Origin',(-1.675,0.,-2.05128338857182E-16));
#21501=CARTESIAN_POINT('',(-1.675,-2.97627328869246E-33,-0.3969));
#21502=CARTESIAN_POINT('',(-1.675,-2.97627328869245E-33,0.3969));
#21503=CARTESIAN_POINT('Origin',(-1.675,0.,-2.05128338857182E-16));
#21504=CARTESIAN_POINT('Origin',(-1.18440385848747,0.,1.18440385848747));
#21505=CARTESIAN_POINT('',(-1.46505453994041,6.26819044436628E-33,0.903753177034526));
#21506=CARTESIAN_POINT('',(-0.903753177034527,-1.22207370217512E-32,1.46505453994041));
#21507=CARTESIAN_POINT('Origin',(-1.18440385848747,0.,1.18440385848747));
#21508=CARTESIAN_POINT('Origin',(-3.07692508285772E-16,0.,1.675));
#21509=CARTESIAN_POINT('',(-0.3969,-2.97627328869246E-33,1.675));
#21510=CARTESIAN_POINT('',(0.396899999999999,-2.97627328869245E-33,1.675));
#21511=CARTESIAN_POINT('Origin',(-3.07692508285772E-16,0.,1.675));
#21512=CARTESIAN_POINT('Origin',(1.18440385848747,0.,1.18440385848747));
#21513=CARTESIAN_POINT('',(0.903753177034526,9.34967835538585E-33,1.46505453994041));
#21514=CARTESIAN_POINT('',(1.46505453994041,-1.53022249327708E-32,0.903753177034527));
#21515=CARTESIAN_POINT('Origin',(1.18440385848747,0.,1.18440385848747));
#21516=CARTESIAN_POINT('',(0.,0.,0.));
#21517=CARTESIAN_POINT('Origin',(1.18440385848747,0.,1.18440385848747));
#21518=CARTESIAN_POINT('',(0.846804978391753,-0.07938,1.40825612658882));
#21519=CARTESIAN_POINT('',(1.40825612658882,-0.07938,0.846804978391754));
#21520=CARTESIAN_POINT('Ctrl Pts',(0.846804978391752,-0.0793800000000001,
1.40825612658882));
#21521=CARTESIAN_POINT('Ctrl Pts',(0.854205272175554,-0.123401821157026,
1.40380622184538));
#21522=CARTESIAN_POINT('Ctrl Pts',(0.867957148219441,-0.166543350814306,
1.39550172959303));
#21523=CARTESIAN_POINT('Ctrl Pts',(0.902193646979982,-0.237231147975234,
1.3735491215176));
#21524=CARTESIAN_POINT('Ctrl Pts',(0.920778333482564,-0.266264900654909,
1.36127834356734));
#21525=CARTESIAN_POINT('Ctrl Pts',(0.962485392528369,-0.317195968905306,
1.33211611256184));
#21526=CARTESIAN_POINT('Ctrl Pts',(0.985600426557816,-0.33909093068465,
1.31521005565926));
#21527=CARTESIAN_POINT('Ctrl Pts',(1.03253285680459,-0.373586846396559,
1.27866649102984));
#21528=CARTESIAN_POINT('Ctrl Pts',(1.05871835910697,-0.388086240756494,
1.25722555095714));
#21529=CARTESIAN_POINT('Ctrl Pts',(1.11153475808518,-0.407068917407805,
1.2107812086231));
#21530=CARTESIAN_POINT('Ctrl Pts',(1.13814686046673,-0.411552957311693,
1.18575674747573));
#21531=CARTESIAN_POINT('Ctrl Pts',(1.18575674747573,-0.411552957311693,
1.13814686046673));
#21532=CARTESIAN_POINT('Ctrl Pts',(1.2107812086231,-0.407068917407805,1.11153475808518));
#21533=CARTESIAN_POINT('Ctrl Pts',(1.25722555095713,-0.388086240756494,
1.05871835910697));
#21534=CARTESIAN_POINT('Ctrl Pts',(1.27866649102984,-0.373586846396559,
1.03253285680459));
#21535=CARTESIAN_POINT('Ctrl Pts',(1.31521005565926,-0.33909093068465,0.985600426557816));
#21536=CARTESIAN_POINT('Ctrl Pts',(1.33211611256184,-0.317195968905306,
0.962485392528369));
#21537=CARTESIAN_POINT('Ctrl Pts',(1.36127834356734,-0.266264900654909,
0.920778333482565));
#21538=CARTESIAN_POINT('Ctrl Pts',(1.3735491215176,-0.237231147975234,0.902193646979983));
#21539=CARTESIAN_POINT('Ctrl Pts',(1.39550172959303,-0.166543350814306,
0.867957148219442));
#21540=CARTESIAN_POINT('Ctrl Pts',(1.40380622184538,-0.123401821157026,
0.854205272175555));
#21541=CARTESIAN_POINT('Ctrl Pts',(1.40825612658882,-0.0793800000000001,
0.846804978391753));
#21542=CARTESIAN_POINT('',(0.886256117232623,-0.07938,1.45861320581289));
#21543=CARTESIAN_POINT('Origin',(1.18440385848747,-0.07938,1.18440385848747));
#21544=CARTESIAN_POINT('',(1.45861320581289,-0.07938,0.886256117232624));
#21545=CARTESIAN_POINT('Ctrl Pts',(1.45861320581289,-0.0793800000000001,
0.886256117232623));
#21546=CARTESIAN_POINT('Ctrl Pts',(1.45630208793976,-0.101649918886749,
0.890059788636852));
#21547=CARTESIAN_POINT('Ctrl Pts',(1.45296717977858,-0.123823518623746,
0.895520212222107));
#21548=CARTESIAN_POINT('Ctrl Pts',(1.43904931717599,-0.192480977588836,
0.917859913453975));
#21549=CARTESIAN_POINT('Ctrl Pts',(1.4243271592157,-0.236152929235938,0.940896403863072));
#21550=CARTESIAN_POINT('Ctrl Pts',(1.39055359345152,-0.303141259068212,
0.990027513266106));
#21551=CARTESIAN_POINT('Ctrl Pts',(1.36743459453896,-0.335108247315849,
1.02199477007745));
#21552=CARTESIAN_POINT('Ctrl Pts',(1.32643091652006,-0.373243761060364,
1.07446535104584));
#21553=CARTESIAN_POINT('Ctrl Pts',(1.30441816675528,-0.387888272594439,
1.10126842659597));
#21554=CARTESIAN_POINT('Ctrl Pts',(1.25681160160691,-0.407041111792943,
1.15530234155453));
#21555=CARTESIAN_POINT('Ctrl Pts',(1.23119764287622,-0.411552957311693,
1.18251418313119));
#21556=CARTESIAN_POINT('Ctrl Pts',(1.18251418313119,-0.411552957311693,
1.23119764287622));
#21557=CARTESIAN_POINT('Ctrl Pts',(1.15530234155453,-0.407041111792943,
1.25681160160691));
#21558=CARTESIAN_POINT('Ctrl Pts',(1.10126842659597,-0.387888272594439,
1.30441816675528));
#21559=CARTESIAN_POINT('Ctrl Pts',(1.07446535104584,-0.373243761060364,
1.32643091652006));
#21560=CARTESIAN_POINT('Ctrl Pts',(1.02199477007745,-0.335108247315848,
1.36743459453896));
#21561=CARTESIAN_POINT('Ctrl Pts',(0.990027513266105,-0.303141259068211,
1.39055359345152));
#21562=CARTESIAN_POINT('Ctrl Pts',(0.940896403863071,-0.236152929235937,
1.42432715921571));
#21563=CARTESIAN_POINT('Ctrl Pts',(0.917859913453974,-0.192480977588835,
1.43904931717599));
#21564=CARTESIAN_POINT('Ctrl Pts',(0.895520212222106,-0.123823518623745,
1.45296717977858));
#21565=CARTESIAN_POINT('Ctrl Pts',(0.890059788636851,-0.101649918886749,
1.45630208793976));
#21566=CARTESIAN_POINT('Ctrl Pts',(0.886256117232622,-0.0793800000000001,
1.45861320581289));
#21567=CARTESIAN_POINT('Origin',(1.18440385848747,-0.07938,1.18440385848747));
#21568=CARTESIAN_POINT('Origin',(0.,-0.27783,0.));
#21569=CARTESIAN_POINT('',(0.404717578595295,-0.07938,1.65807299932179));
#21570=CARTESIAN_POINT('Origin',(0.,-0.07938,0.));
#21571=CARTESIAN_POINT('',(-0.404717578595296,-0.07938,1.65807299932179));
#21572=CARTESIAN_POINT('Ctrl Pts',(0.404717578595296,-0.0793800000000001,
1.65807299932179));
#21573=CARTESIAN_POINT('Ctrl Pts',(0.400393769631747,-0.101649918886749,
1.65912839404491));
#21574=CARTESIAN_POINT('Ctrl Pts',(0.394174530911058,-0.123823518623745,
1.66063136041479));
#21575=CARTESIAN_POINT('Ctrl Pts',(0.368536561654407,-0.192480977588835,
1.66658649961961));
#21576=CARTESIAN_POINT('Ctrl Pts',(0.341837165343982,-0.236152929235937,
1.67246562047521));
#21577=CARTESIAN_POINT('Ctrl Pts',(0.283214707341173,-0.303141259068211,
1.68332504372461));
#21578=CARTESIAN_POINT('Ctrl Pts',(0.244262842368623,-0.335108247315849,
1.68958170688653));
#21579=CARTESIAN_POINT('Ctrl Pts',(0.178166559972324,-0.373243761060364,
1.69769003172132));
#21580=CARTESIAN_POINT('Ctrl Pts',(0.143648558862931,-0.387888272594439,
1.70107730356824));
#21581=CARTESIAN_POINT('Ctrl Pts',(0.0717778861362652,-0.407041111792943,
1.70562212620408));
#21582=CARTESIAN_POINT('Ctrl Pts',(0.0344244045173309,-0.411552957311693,
1.706752));
#21583=CARTESIAN_POINT('Ctrl Pts',(-0.0344244045173315,-0.411552957311693,
1.706752));
#21584=CARTESIAN_POINT('Ctrl Pts',(-0.0717778861362658,-0.407041111792943,
1.70562212620408));
#21585=CARTESIAN_POINT('Ctrl Pts',(-0.143648558862932,-0.387888272594439,
1.70107730356824));
#21586=CARTESIAN_POINT('Ctrl Pts',(-0.178166559972325,-0.373243761060364,
1.69769003172132));
#21587=CARTESIAN_POINT('Ctrl Pts',(-0.244262842368624,-0.335108247315849,
1.68958170688653));
#21588=CARTESIAN_POINT('Ctrl Pts',(-0.283214707341173,-0.303141259068212,
1.68332504372461));
#21589=CARTESIAN_POINT('Ctrl Pts',(-0.341837165343982,-0.236152929235937,
1.67246562047521));
#21590=CARTESIAN_POINT('Ctrl Pts',(-0.368536561654408,-0.192480977588835,
1.66658649961961));
#21591=CARTESIAN_POINT('Ctrl Pts',(-0.394174530911059,-0.123823518623745,
1.66063136041479));
#21592=CARTESIAN_POINT('Ctrl Pts',(-0.400393769631748,-0.101649918886749,
1.65912839404491));
#21593=CARTESIAN_POINT('Ctrl Pts',(-0.404717578595297,-0.0793800000000001,
1.65807299932179));
#21594=CARTESIAN_POINT('',(-0.886256117232624,-0.07938,1.45861320581289));
#21595=CARTESIAN_POINT('Origin',(0.,-0.07938,0.));
#21596=CARTESIAN_POINT('',(-1.45861320581289,-0.07938,0.886256117232623));
#21597=CARTESIAN_POINT('Ctrl Pts',(-0.886256117232623,-0.0793800000000001,
1.45861320581289));
#21598=CARTESIAN_POINT('Ctrl Pts',(-0.890059788636852,-0.101649918886749,
1.45630208793976));
#21599=CARTESIAN_POINT('Ctrl Pts',(-0.895520212222106,-0.123823518623745,
1.45296717977858));
#21600=CARTESIAN_POINT('Ctrl Pts',(-0.917859913453974,-0.192480977588835,
1.43904931717599));
#21601=CARTESIAN_POINT('Ctrl Pts',(-0.940896403863071,-0.236152929235937,
1.4243271592157));
#21602=CARTESIAN_POINT('Ctrl Pts',(-0.990027513266105,-0.303141259068211,
1.39055359345152));
#21603=CARTESIAN_POINT('Ctrl Pts',(-1.02199477007745,-0.335108247315848,
1.36743459453896));
#21604=CARTESIAN_POINT('Ctrl Pts',(-1.07446535104584,-0.373243761060364,
1.32643091652006));
#21605=CARTESIAN_POINT('Ctrl Pts',(-1.10126842659597,-0.387888272594439,
1.30441816675528));
#21606=CARTESIAN_POINT('Ctrl Pts',(-1.15530234155453,-0.407041111792943,
1.25681160160691));
#21607=CARTESIAN_POINT('Ctrl Pts',(-1.18251418313119,-0.411552957311693,
1.23119764287622));
#21608=CARTESIAN_POINT('Ctrl Pts',(-1.23119764287622,-0.411552957311693,
1.18251418313119));
#21609=CARTESIAN_POINT('Ctrl Pts',(-1.25681160160691,-0.407041111792943,
1.15530234155453));
#21610=CARTESIAN_POINT('Ctrl Pts',(-1.30441816675528,-0.387888272594439,
1.10126842659597));
#21611=CARTESIAN_POINT('Ctrl Pts',(-1.32643091652006,-0.373243761060365,
1.07446535104584));
#21612=CARTESIAN_POINT('Ctrl Pts',(-1.36743459453896,-0.335108247315849,
1.02199477007745));
#21613=CARTESIAN_POINT('Ctrl Pts',(-1.39055359345152,-0.303141259068212,
0.990027513266106));
#21614=CARTESIAN_POINT('Ctrl Pts',(-1.4243271592157,-0.236152929235938,
0.940896403863071));
#21615=CARTESIAN_POINT('Ctrl Pts',(-1.43904931717599,-0.192480977588836,
0.917859913453974));
#21616=CARTESIAN_POINT('Ctrl Pts',(-1.45296717977858,-0.123823518623746,
0.895520212222106));
#21617=CARTESIAN_POINT('Ctrl Pts',(-1.45630208793976,-0.101649918886749,
0.890059788636852));
#21618=CARTESIAN_POINT('Ctrl Pts',(-1.45861320581289,-0.0793800000000001,
0.886256117232623));
#21619=CARTESIAN_POINT('',(-1.65807299932179,-0.07938,0.404717578595295));
#21620=CARTESIAN_POINT('Origin',(0.,-0.07938,0.));
#21621=CARTESIAN_POINT('',(-1.706752,-0.411552957311693,2.08591827245526E-16));
#21622=CARTESIAN_POINT('Ctrl Pts',(-1.65807299932179,-0.0793800000000001,
0.404717578595296));
#21623=CARTESIAN_POINT('Ctrl Pts',(-1.65912839404491,-0.101649918886749,
0.400393769631747));
#21624=CARTESIAN_POINT('Ctrl Pts',(-1.66063136041479,-0.123823518623745,
0.394174530911058));
#21625=CARTESIAN_POINT('Ctrl Pts',(-1.66658649961961,-0.192480977588835,
0.368536561654407));
#21626=CARTESIAN_POINT('Ctrl Pts',(-1.67246562047521,-0.236152929235937,
0.341837165343982));
#21627=CARTESIAN_POINT('Ctrl Pts',(-1.68332504372461,-0.303141259068211,
0.283214707341173));
#21628=CARTESIAN_POINT('Ctrl Pts',(-1.68958170688653,-0.335108247315848,
0.244262842368623));
#21629=CARTESIAN_POINT('Ctrl Pts',(-1.69769003172132,-0.373243761060364,
0.178166559972324));
#21630=CARTESIAN_POINT('Ctrl Pts',(-1.70107730356824,-0.387888272594439,
0.143648558862931));
#21631=CARTESIAN_POINT('Ctrl Pts',(-1.70562212620408,-0.407041111792943,
0.0717778861362656));
#21632=CARTESIAN_POINT('Ctrl Pts',(-1.706752,-0.411552957311693,0.0344244045173313));
#21633=CARTESIAN_POINT('Ctrl Pts',(-1.706752,-0.411552957311693,2.08166817117217E-16));
#21634=CARTESIAN_POINT('',(-1.706752,-0.47628,2.09016837373834E-16));
#21635=CARTESIAN_POINT('',(-1.706752,-0.27783,2.09016837373834E-16));
#21636=CARTESIAN_POINT('Origin',(0.,-0.47628,0.));
#21637=CARTESIAN_POINT('',(-1.65807299932179,-0.07938,-0.404717578595296));
#21638=CARTESIAN_POINT('Ctrl Pts',(-1.706752,-0.411552957311693,2.0122792321331E-16));
#21639=CARTESIAN_POINT('Ctrl Pts',(-1.706752,-0.411552957311693,-0.0344244045173309));
#21640=CARTESIAN_POINT('Ctrl Pts',(-1.70562212620408,-0.407041111792943,
-0.0717778861362652));
#21641=CARTESIAN_POINT('Ctrl Pts',(-1.70107730356824,-0.387888272594439,
-0.143648558862931));
#21642=CARTESIAN_POINT('Ctrl Pts',(-1.69769003172132,-0.373243761060365,
-0.178166559972324));
#21643=CARTESIAN_POINT('Ctrl Pts',(-1.68958170688653,-0.335108247315849,
-0.244262842368623));
#21644=CARTESIAN_POINT('Ctrl Pts',(-1.68332504372461,-0.303141259068212,
-0.283214707341173));
#21645=CARTESIAN_POINT('Ctrl Pts',(-1.67246562047521,-0.236152929235938,
-0.341837165343982));
#21646=CARTESIAN_POINT('Ctrl Pts',(-1.66658649961961,-0.192480977588836,
-0.368536561654407));
#21647=CARTESIAN_POINT('Ctrl Pts',(-1.66063136041479,-0.123823518623745,
-0.394174530911059));
#21648=CARTESIAN_POINT('Ctrl Pts',(-1.65912839404491,-0.101649918886749,
-0.400393769631748));
#21649=CARTESIAN_POINT('Ctrl Pts',(-1.65807299932179,-0.0793800000000001,
-0.404717578595296));
#21650=CARTESIAN_POINT('',(-1.45861320581289,-0.07938,-0.886256117232623));
#21651=CARTESIAN_POINT('Origin',(0.,-0.07938,0.));
#21652=CARTESIAN_POINT('',(-0.886256117232623,-0.07938,-1.45861320581289));
#21653=CARTESIAN_POINT('Ctrl Pts',(-1.45861320581289,-0.0793800000000001,
-0.886256117232623));
#21654=CARTESIAN_POINT('Ctrl Pts',(-1.45630208793976,-0.101649918886749,
-0.890059788636852));
#21655=CARTESIAN_POINT('Ctrl Pts',(-1.45296717977858,-0.123823518623745,
-0.895520212222106));
#21656=CARTESIAN_POINT('Ctrl Pts',(-1.43904931717599,-0.192480977588835,
-0.917859913453974));
#21657=CARTESIAN_POINT('Ctrl Pts',(-1.4243271592157,-0.236152929235937,
-0.940896403863072));
#21658=CARTESIAN_POINT('Ctrl Pts',(-1.39055359345152,-0.303141259068212,
-0.990027513266106));
#21659=CARTESIAN_POINT('Ctrl Pts',(-1.36743459453896,-0.335108247315849,
-1.02199477007745));
#21660=CARTESIAN_POINT('Ctrl Pts',(-1.32643091652006,-0.373243761060364,
-1.07446535104584));
#21661=CARTESIAN_POINT('Ctrl Pts',(-1.30441816675528,-0.387888272594439,
-1.10126842659597));
#21662=CARTESIAN_POINT('Ctrl Pts',(-1.25681160160691,-0.407041111792943,
-1.15530234155453));
#21663=CARTESIAN_POINT('Ctrl Pts',(-1.23119764287622,-0.411552957311693,
-1.18251418313119));
#21664=CARTESIAN_POINT('Ctrl Pts',(-1.18251418313119,-0.411552957311693,
-1.23119764287622));
#21665=CARTESIAN_POINT('Ctrl Pts',(-1.15530234155453,-0.407041111792943,
-1.25681160160691));
#21666=CARTESIAN_POINT('Ctrl Pts',(-1.10126842659597,-0.387888272594439,
-1.30441816675528));
#21667=CARTESIAN_POINT('Ctrl Pts',(-1.07446535104584,-0.373243761060364,
-1.32643091652006));
#21668=CARTESIAN_POINT('Ctrl Pts',(-1.02199477007745,-0.335108247315848,
-1.36743459453896));
#21669=CARTESIAN_POINT('Ctrl Pts',(-0.990027513266105,-0.303141259068211,
-1.39055359345152));
#21670=CARTESIAN_POINT('Ctrl Pts',(-0.940896403863071,-0.236152929235936,
-1.42432715921571));
#21671=CARTESIAN_POINT('Ctrl Pts',(-0.917859913453974,-0.192480977588835,
-1.43904931717599));
#21672=CARTESIAN_POINT('Ctrl Pts',(-0.895520212222106,-0.123823518623745,
-1.45296717977858));
#21673=CARTESIAN_POINT('Ctrl Pts',(-0.890059788636851,-0.101649918886749,
-1.45630208793976));
#21674=CARTESIAN_POINT('Ctrl Pts',(-0.886256117232623,-0.0793800000000001,
-1.45861320581289));
#21675=CARTESIAN_POINT('',(-0.404717578595295,-0.07938,-1.65807299932179));
#21676=CARTESIAN_POINT('Origin',(0.,-0.07938,0.));
#21677=CARTESIAN_POINT('',(0.404717578595296,-0.07938,-1.65807299932179));
#21678=CARTESIAN_POINT('Ctrl Pts',(-0.404717578595296,-0.0793800000000001,
-1.65807299932179));
#21679=CARTESIAN_POINT('Ctrl Pts',(-0.400393769631747,-0.101649918886749,
-1.65912839404491));
#21680=CARTESIAN_POINT('Ctrl Pts',(-0.394174530911058,-0.123823518623746,
-1.66063136041479));
#21681=CARTESIAN_POINT('Ctrl Pts',(-0.368536561654407,-0.192480977588836,
-1.66658649961961));
#21682=CARTESIAN_POINT('Ctrl Pts',(-0.341837165343982,-0.236152929235938,
-1.67246562047521));
#21683=CARTESIAN_POINT('Ctrl Pts',(-0.283214707341173,-0.303141259068212,
-1.68332504372461));
#21684=CARTESIAN_POINT('Ctrl Pts',(-0.244262842368623,-0.335108247315849,
-1.68958170688653));
#21685=CARTESIAN_POINT('Ctrl Pts',(-0.178166559972324,-0.373243761060364,
-1.69769003172132));
#21686=CARTESIAN_POINT('Ctrl Pts',(-0.143648558862931,-0.387888272594439,
-1.70107730356824));
#21687=CARTESIAN_POINT('Ctrl Pts',(-0.0717778861362653,-0.407041111792943,
-1.70562212620408));
#21688=CARTESIAN_POINT('Ctrl Pts',(-0.034424404517331,-0.411552957311693,
-1.706752));
#21689=CARTESIAN_POINT('Ctrl Pts',(0.0344244045173312,-0.411552957311693,
-1.706752));
#21690=CARTESIAN_POINT('Ctrl Pts',(0.0717778861362655,-0.407041111792943,
-1.70562212620408));
#21691=CARTESIAN_POINT('Ctrl Pts',(0.143648558862931,-0.387888272594439,
-1.70107730356824));
#21692=CARTESIAN_POINT('Ctrl Pts',(0.178166559972324,-0.373243761060364,
-1.69769003172132));
#21693=CARTESIAN_POINT('Ctrl Pts',(0.244262842368623,-0.335108247315849,
-1.68958170688653));
#21694=CARTESIAN_POINT('Ctrl Pts',(0.283214707341173,-0.303141259068212,
-1.68332504372461));
#21695=CARTESIAN_POINT('Ctrl Pts',(0.341837165343982,-0.236152929235937,
-1.67246562047521));
#21696=CARTESIAN_POINT('Ctrl Pts',(0.368536561654407,-0.192480977588835,
-1.66658649961961));
#21697=CARTESIAN_POINT('Ctrl Pts',(0.394174530911059,-0.123823518623745,
-1.66063136041479));
#21698=CARTESIAN_POINT('Ctrl Pts',(0.400393769631748,-0.101649918886749,
-1.65912839404491));
#21699=CARTESIAN_POINT('Ctrl Pts',(0.404717578595296,-0.0793800000000001,
-1.65807299932179));
#21700=CARTESIAN_POINT('',(0.886256117232623,-0.07938,-1.45861320581289));
#21701=CARTESIAN_POINT('Origin',(0.,-0.07938,0.));
#21702=CARTESIAN_POINT('',(1.45861320581289,-0.07938,-0.886256117232623));
#21703=CARTESIAN_POINT('Ctrl Pts',(0.886256117232623,-0.0793800000000001,
-1.45861320581289));
#21704=CARTESIAN_POINT('Ctrl Pts',(0.890059788636852,-0.101649918886749,
-1.45630208793976));
#21705=CARTESIAN_POINT('Ctrl Pts',(0.895520212222106,-0.123823518623745,
-1.45296717977858));
#21706=CARTESIAN_POINT('Ctrl Pts',(0.917859913453974,-0.192480977588835,
-1.43904931717599));
#21707=CARTESIAN_POINT('Ctrl Pts',(0.940896403863072,-0.236152929235937,
-1.4243271592157));
#21708=CARTESIAN_POINT('Ctrl Pts',(0.990027513266106,-0.303141259068211,
-1.39055359345152));
#21709=CARTESIAN_POINT('Ctrl Pts',(1.02199477007745,-0.335108247315849,
-1.36743459453896));
#21710=CARTESIAN_POINT('Ctrl Pts',(1.07446535104584,-0.373243761060364,
-1.32643091652006));
#21711=CARTESIAN_POINT('Ctrl Pts',(1.10126842659597,-0.387888272594439,
-1.30441816675528));
#21712=CARTESIAN_POINT('Ctrl Pts',(1.15530234155453,-0.407041111792943,
-1.25681160160691));
#21713=CARTESIAN_POINT('Ctrl Pts',(1.18251418313119,-0.411552957311693,
-1.23119764287622));
#21714=CARTESIAN_POINT('Ctrl Pts',(1.23119764287622,-0.411552957311693,
-1.18251418313119));
#21715=CARTESIAN_POINT('Ctrl Pts',(1.25681160160691,-0.407041111792943,
-1.15530234155453));
#21716=CARTESIAN_POINT('Ctrl Pts',(1.30441816675528,-0.387888272594439,
-1.10126842659597));
#21717=CARTESIAN_POINT('Ctrl Pts',(1.32643091652006,-0.373243761060364,
-1.07446535104584));
#21718=CARTESIAN_POINT('Ctrl Pts',(1.36743459453896,-0.335108247315849,
-1.02199477007745));
#21719=CARTESIAN_POINT('Ctrl Pts',(1.39055359345152,-0.303141259068212,
-0.990027513266105));
#21720=CARTESIAN_POINT('Ctrl Pts',(1.4243271592157,-0.236152929235937,-0.940896403863071));
#21721=CARTESIAN_POINT('Ctrl Pts',(1.43904931717599,-0.192480977588835,
-0.917859913453974));
#21722=CARTESIAN_POINT('Ctrl Pts',(1.45296717977858,-0.123823518623745,
-0.895520212222106));
#21723=CARTESIAN_POINT('Ctrl Pts',(1.45630208793976,-0.101649918886749,
-0.890059788636852));
#21724=CARTESIAN_POINT('Ctrl Pts',(1.45861320581289,-0.0793800000000001,
-0.886256117232623));
#21725=CARTESIAN_POINT('',(1.65807299932179,-0.07938,-0.404717578595296));
#21726=CARTESIAN_POINT('Origin',(0.,-0.07938,0.));
#21727=CARTESIAN_POINT('',(1.65807299932179,-0.07938,0.404717578595296));
#21728=CARTESIAN_POINT('Ctrl Pts',(1.65807299932179,-0.0793800000000001,
-0.404717578595296));
#21729=CARTESIAN_POINT('Ctrl Pts',(1.65912839404491,-0.101649918886749,
-0.400393769631747));
#21730=CARTESIAN_POINT('Ctrl Pts',(1.66063136041479,-0.123823518623745,
-0.394174530911058));
#21731=CARTESIAN_POINT('Ctrl Pts',(1.66658649961961,-0.192480977588835,
-0.368536561654407));
#21732=CARTESIAN_POINT('Ctrl Pts',(1.67246562047521,-0.236152929235937,
-0.341837165343982));
#21733=CARTESIAN_POINT('Ctrl Pts',(1.68332504372461,-0.303141259068212,
-0.283214707341173));
#21734=CARTESIAN_POINT('Ctrl Pts',(1.68958170688653,-0.335108247315849,
-0.244262842368623));
#21735=CARTESIAN_POINT('Ctrl Pts',(1.69769003172132,-0.373243761060364,
-0.178166559972324));
#21736=CARTESIAN_POINT('Ctrl Pts',(1.70107730356824,-0.387888272594439,
-0.143648558862931));
#21737=CARTESIAN_POINT('Ctrl Pts',(1.70562212620408,-0.407041111792943,
-0.0717778861362655));
#21738=CARTESIAN_POINT('Ctrl Pts',(1.706752,-0.411552957311693,-0.0344244045173312));
#21739=CARTESIAN_POINT('Ctrl Pts',(1.706752,-0.411552957311693,0.0344244045173312));
#21740=CARTESIAN_POINT('Ctrl Pts',(1.70562212620408,-0.407041111792943,
0.0717778861362655));
#21741=CARTESIAN_POINT('Ctrl Pts',(1.70107730356824,-0.387888272594439,
0.143648558862931));
#21742=CARTESIAN_POINT('Ctrl Pts',(1.69769003172132,-0.373243761060364,
0.178166559972324));
#21743=CARTESIAN_POINT('Ctrl Pts',(1.68958170688653,-0.335108247315849,
0.244262842368623));
#21744=CARTESIAN_POINT('Ctrl Pts',(1.68332504372461,-0.303141259068212,
0.283214707341173));
#21745=CARTESIAN_POINT('Ctrl Pts',(1.67246562047521,-0.236152929235937,
0.341837165343982));
#21746=CARTESIAN_POINT('Ctrl Pts',(1.66658649961961,-0.192480977588835,
0.368536561654407));
#21747=CARTESIAN_POINT('Ctrl Pts',(1.66063136041479,-0.123823518623745,
0.394174530911058));
#21748=CARTESIAN_POINT('Ctrl Pts',(1.65912839404491,-0.101649918886749,
0.400393769631747));
#21749=CARTESIAN_POINT('Ctrl Pts',(1.65807299932179,-0.0793800000000001,
0.404717578595296));
#21750=CARTESIAN_POINT('Origin',(0.,-0.07938,0.));
#21751=CARTESIAN_POINT('Origin',(0.,-0.07938,0.));
#21752=CARTESIAN_POINT('',(0.397005914195118,-0.07938,1.59456899932179));
#21753=CARTESIAN_POINT('Origin',(0.,-0.07938,0.));
#21754=CARTESIAN_POINT('Origin',(-3.33066907387547E-16,-0.07938,1.675));
#21755=CARTESIAN_POINT('Origin',(-3.33066907387547E-16,0.,1.675));
#21756=CARTESIAN_POINT('',(-0.397005914195118,-0.07938,1.59456899932179));
#21757=CARTESIAN_POINT('Ctrl Pts',(-0.397005914195119,-0.0793800000000001,
1.59456899932179));
#21758=CARTESIAN_POINT('Ctrl Pts',(-0.3886265584581,-0.123401821157026,
1.59665523941937));
#21759=CARTESIAN_POINT('Ctrl Pts',(-0.373030350867485,-0.166543350814306,
1.60050712143809));
#21760=CARTESIAN_POINT('Ctrl Pts',(-0.333298652394954,-0.237231147975234,
1.60919314384089));
#21761=CARTESIAN_POINT('Ctrl Pts',(-0.311480544243687,-0.266264900654909,
1.61365775139403));
#21762=CARTESIAN_POINT('Ctrl Pts',(-0.261368388670537,-0.317195968905306,
1.62252828437015));
#21763=CARTESIAN_POINT('Ctrl Pts',(-0.233069203882014,-0.33909093068465,
1.62691869420078));
#21764=CARTESIAN_POINT('Ctrl Pts',(-0.174042761838764,-0.373586846396559,
1.63426473152765));
#21765=CARTESIAN_POINT('Ctrl Pts',(-0.14036578147155,-0.388086240756494,
1.63761964365402));
#21766=CARTESIAN_POINT('Ctrl Pts',(-0.0701778381840615,-0.407068917407805,
1.64212536811722));
#21767=CARTESIAN_POINT('Ctrl Pts',(-0.0336652739555918,-0.411552957311693,
1.643248));
#21768=CARTESIAN_POINT('Ctrl Pts',(0.0336652739555913,-0.411552957311693,
1.643248));
#21769=CARTESIAN_POINT('Ctrl Pts',(0.070177838184061,-0.407068917407805,
1.64212536811722));
#21770=CARTESIAN_POINT('Ctrl Pts',(0.140365781471549,-0.388086240756494,
1.63761964365402));
#21771=CARTESIAN_POINT('Ctrl Pts',(0.174042761838763,-0.373586846396559,
1.63426473152765));
#21772=CARTESIAN_POINT('Ctrl Pts',(0.233069203882014,-0.33909093068465,
1.62691869420078));
#21773=CARTESIAN_POINT('Ctrl Pts',(0.261368388670536,-0.317195968905306,
1.62252828437015));
#21774=CARTESIAN_POINT('Ctrl Pts',(0.311480544243686,-0.266264900654908,
1.61365775139403));
#21775=CARTESIAN_POINT('Ctrl Pts',(0.333298652394954,-0.237231147975234,
1.60919314384089));
#21776=CARTESIAN_POINT('Ctrl Pts',(0.373030350867484,-0.166543350814306,
1.60050712143809));
#21777=CARTESIAN_POINT('Ctrl Pts',(0.388626558458099,-0.123401821157026,
1.59665523941937));
#21778=CARTESIAN_POINT('Ctrl Pts',(0.397005914195118,-0.07938,1.59456899932179));
#21779=CARTESIAN_POINT('Origin',(-3.33066907387547E-16,-0.07938,1.675));
#21780=CARTESIAN_POINT('Origin',(0.,-0.07938,0.));
#21781=CARTESIAN_POINT('',(-0.846804978391754,-0.07938,1.40825612658882));
#21782=CARTESIAN_POINT('Origin',(0.,-0.07938,0.));
#21783=CARTESIAN_POINT('Origin',(-1.18440385848747,-0.07938,1.18440385848747));
#21784=CARTESIAN_POINT('Origin',(-1.18440385848747,0.,1.18440385848747));
#21785=CARTESIAN_POINT('',(-1.40825612658882,-0.07938,0.846804978391753));
#21786=CARTESIAN_POINT('Ctrl Pts',(-1.40825612658882,-0.0793800000000001,
0.846804978391753));
#21787=CARTESIAN_POINT('Ctrl Pts',(-1.40380622184538,-0.123401821157026,
0.854205272175555));
#21788=CARTESIAN_POINT('Ctrl Pts',(-1.39550172959303,-0.166543350814306,
0.867957148219442));
#21789=CARTESIAN_POINT('Ctrl Pts',(-1.3735491215176,-0.237231147975235,
0.902193646979983));
#21790=CARTESIAN_POINT('Ctrl Pts',(-1.36127834356734,-0.266264900654909,
0.920778333482565));
#21791=CARTESIAN_POINT('Ctrl Pts',(-1.33211611256184,-0.317195968905306,
0.962485392528369));
#21792=CARTESIAN_POINT('Ctrl Pts',(-1.31521005565926,-0.339090930684651,
0.985600426557816));
#21793=CARTESIAN_POINT('Ctrl Pts',(-1.27866649102984,-0.373586846396559,
1.03253285680459));
#21794=CARTESIAN_POINT('Ctrl Pts',(-1.25722555095714,-0.388086240756494,
1.05871835910697));
#21795=CARTESIAN_POINT('Ctrl Pts',(-1.2107812086231,-0.407068917407805,
1.11153475808518));
#21796=CARTESIAN_POINT('Ctrl Pts',(-1.18575674747573,-0.411552957311693,
1.13814686046673));
#21797=CARTESIAN_POINT('Ctrl Pts',(-1.13814686046673,-0.411552957311693,
1.18575674747573));
#21798=CARTESIAN_POINT('Ctrl Pts',(-1.11153475808518,-0.407068917407805,
1.2107812086231));
#21799=CARTESIAN_POINT('Ctrl Pts',(-1.05871835910697,-0.388086240756494,
1.25722555095714));
#21800=CARTESIAN_POINT('Ctrl Pts',(-1.03253285680459,-0.373586846396559,
1.27866649102984));
#21801=CARTESIAN_POINT('Ctrl Pts',(-0.985600426557816,-0.33909093068465,
1.31521005565926));
#21802=CARTESIAN_POINT('Ctrl Pts',(-0.962485392528369,-0.317195968905306,
1.33211611256184));
#21803=CARTESIAN_POINT('Ctrl Pts',(-0.920778333482565,-0.266264900654908,
1.36127834356734));
#21804=CARTESIAN_POINT('Ctrl Pts',(-0.902193646979983,-0.237231147975234,
1.3735491215176));
#21805=CARTESIAN_POINT('Ctrl Pts',(-0.867957148219442,-0.166543350814306,
1.39550172959303));
#21806=CARTESIAN_POINT('Ctrl Pts',(-0.854205272175555,-0.123401821157026,
1.40380622184538));
#21807=CARTESIAN_POINT('Ctrl Pts',(-0.846804978391753,-0.0793800000000001,
1.40825612658882));
#21808=CARTESIAN_POINT('Origin',(-1.18440385848747,-0.07938,1.18440385848747));
#21809=CARTESIAN_POINT('Origin',(0.,-0.07938,0.));
#21810=CARTESIAN_POINT('',(-1.59456899932179,-0.07938,0.397005914195118));
#21811=CARTESIAN_POINT('Origin',(0.,-0.07938,0.));
#21812=CARTESIAN_POINT('Origin',(-1.675,-0.07938,-2.22044604925031E-16));
#21813=CARTESIAN_POINT('Origin',(-1.675,0.,-2.22044604925031E-16));
#21814=CARTESIAN_POINT('',(-1.59456899932179,-0.07938,-0.397005914195118));
#21815=CARTESIAN_POINT('',(-1.643248,-0.411552957311693,3.47540551556327E-18));
#21816=CARTESIAN_POINT('Ctrl Pts',(-1.59456899932179,-0.0793800000000001,
-0.397005914195119));
#21817=CARTESIAN_POINT('Ctrl Pts',(-1.59665523941937,-0.123401821157026,
-0.388626558458099));
#21818=CARTESIAN_POINT('Ctrl Pts',(-1.60050712143809,-0.166543350814306,
-0.373030350867485));
#21819=CARTESIAN_POINT('Ctrl Pts',(-1.60919314384089,-0.237231147975234,
-0.333298652394954));
#21820=CARTESIAN_POINT('Ctrl Pts',(-1.61365775139403,-0.266264900654909,
-0.311480544243686));
#21821=CARTESIAN_POINT('Ctrl Pts',(-1.62252828437015,-0.317195968905306,
-0.261368388670537));
#21822=CARTESIAN_POINT('Ctrl Pts',(-1.62691869420078,-0.33909093068465,
-0.233069203882014));
#21823=CARTESIAN_POINT('Ctrl Pts',(-1.63426473152765,-0.373586846396559,
-0.174042761838764));
#21824=CARTESIAN_POINT('Ctrl Pts',(-1.63761964365402,-0.388086240756494,
-0.140365781471549));
#21825=CARTESIAN_POINT('Ctrl Pts',(-1.64212536811722,-0.407068917407805,
-0.0701778381840614));
#21826=CARTESIAN_POINT('Ctrl Pts',(-1.643248,-0.411552957311693,-0.0336652739555917));
#21827=CARTESIAN_POINT('Ctrl Pts',(-1.643248,-0.411552957311693,-2.0122792321331E-16));
#21828=CARTESIAN_POINT('Origin',(-1.675,-0.07938,-2.22044604925031E-16));
#21829=CARTESIAN_POINT('Ctrl Pts',(-1.643248,-0.411552957311693,-1.94289029309402E-16));
#21830=CARTESIAN_POINT('Ctrl Pts',(-1.643248,-0.411552957311693,0.0336652739555913));
#21831=CARTESIAN_POINT('Ctrl Pts',(-1.64212536811722,-0.407068917407805,
0.0701778381840609));
#21832=CARTESIAN_POINT('Ctrl Pts',(-1.63761964365402,-0.388086240756494,
0.140365781471549));
#21833=CARTESIAN_POINT('Ctrl Pts',(-1.63426473152765,-0.373586846396559,
0.174042761838763));
#21834=CARTESIAN_POINT('Ctrl Pts',(-1.62691869420078,-0.33909093068465,
0.233069203882014));
#21835=CARTESIAN_POINT('Ctrl Pts',(-1.62252828437015,-0.317195968905306,
0.261368388670536));
#21836=CARTESIAN_POINT('Ctrl Pts',(-1.61365775139403,-0.266264900654909,
0.311480544243686));
#21837=CARTESIAN_POINT('Ctrl Pts',(-1.60919314384089,-0.237231147975235,
0.333298652394954));
#21838=CARTESIAN_POINT('Ctrl Pts',(-1.60050712143809,-0.166543350814306,
0.373030350867484));
#21839=CARTESIAN_POINT('Ctrl Pts',(-1.59665523941937,-0.123401821157026,
0.388626558458099));
#21840=CARTESIAN_POINT('Ctrl Pts',(-1.59456899932179,-0.0793800000000001,
0.397005914195118));
#21841=CARTESIAN_POINT('Origin',(0.,-0.07938,0.));
#21842=CARTESIAN_POINT('',(-1.40825612658882,-0.07938,-0.846804978391753));
#21843=CARTESIAN_POINT('Origin',(0.,-0.07938,0.));
#21844=CARTESIAN_POINT('Origin',(-1.18440385848747,-0.07938,-1.18440385848747));
#21845=CARTESIAN_POINT('Origin',(-1.18440385848747,0.,-1.18440385848747));
#21846=CARTESIAN_POINT('',(-0.846804978391753,-0.07938,-1.40825612658882));
#21847=CARTESIAN_POINT('Ctrl Pts',(-0.846804978391753,-0.0793800000000001,
-1.40825612658882));
#21848=CARTESIAN_POINT('Ctrl Pts',(-0.854205272175555,-0.123401821157026,
-1.40380622184538));
#21849=CARTESIAN_POINT('Ctrl Pts',(-0.867957148219442,-0.166543350814306,
-1.39550172959303));
#21850=CARTESIAN_POINT('Ctrl Pts',(-0.902193646979982,-0.237231147975234,
-1.3735491215176));
#21851=CARTESIAN_POINT('Ctrl Pts',(-0.920778333482564,-0.266264900654908,
-1.36127834356734));
#21852=CARTESIAN_POINT('Ctrl Pts',(-0.962485392528368,-0.317195968905306,
-1.33211611256184));
#21853=CARTESIAN_POINT('Ctrl Pts',(-0.985600426557816,-0.33909093068465,
-1.31521005565926));
#21854=CARTESIAN_POINT('Ctrl Pts',(-1.03253285680459,-0.373586846396559,
-1.27866649102984));
#21855=CARTESIAN_POINT('Ctrl Pts',(-1.05871835910697,-0.388086240756494,
-1.25722555095714));
#21856=CARTESIAN_POINT('Ctrl Pts',(-1.11153475808518,-0.407068917407805,
-1.2107812086231));
#21857=CARTESIAN_POINT('Ctrl Pts',(-1.13814686046673,-0.411552957311693,
-1.18575674747573));
#21858=CARTESIAN_POINT('Ctrl Pts',(-1.18575674747573,-0.411552957311693,
-1.13814686046673));
#21859=CARTESIAN_POINT('Ctrl Pts',(-1.2107812086231,-0.407068917407805,
-1.11153475808518));
#21860=CARTESIAN_POINT('Ctrl Pts',(-1.25722555095714,-0.388086240756494,
-1.05871835910697));
#21861=CARTESIAN_POINT('Ctrl Pts',(-1.27866649102984,-0.373586846396559,
-1.03253285680459));
#21862=CARTESIAN_POINT('Ctrl Pts',(-1.31521005565926,-0.33909093068465,
-0.985600426557816));
#21863=CARTESIAN_POINT('Ctrl Pts',(-1.33211611256184,-0.317195968905306,
-0.962485392528369));
#21864=CARTESIAN_POINT('Ctrl Pts',(-1.36127834356734,-0.266264900654909,
-0.920778333482565));
#21865=CARTESIAN_POINT('Ctrl Pts',(-1.3735491215176,-0.237231147975234,
-0.902193646979983));
#21866=CARTESIAN_POINT('Ctrl Pts',(-1.39550172959303,-0.166543350814306,
-0.867957148219442));
#21867=CARTESIAN_POINT('Ctrl Pts',(-1.40380622184538,-0.123401821157026,
-0.854205272175555));
#21868=CARTESIAN_POINT('Ctrl Pts',(-1.40825612658882,-0.07938,-0.846804978391753));
#21869=CARTESIAN_POINT('Origin',(-1.18440385848747,-0.07938,-1.18440385848747));
#21870=CARTESIAN_POINT('Origin',(0.,-0.07938,0.));
#21871=CARTESIAN_POINT('',(-0.397005914195118,-0.07938,-1.59456899932179));
#21872=CARTESIAN_POINT('Origin',(0.,-0.07938,0.));
#21873=CARTESIAN_POINT('Origin',(1.11022302462516E-16,-0.07938,-1.675));
#21874=CARTESIAN_POINT('Origin',(1.11022302462516E-16,0.,-1.675));
#21875=CARTESIAN_POINT('',(0.397005914195118,-0.07938,-1.59456899932179));
#21876=CARTESIAN_POINT('Ctrl Pts',(0.397005914195119,-0.0793800000000001,
-1.59456899932179));
#21877=CARTESIAN_POINT('Ctrl Pts',(0.388626558458099,-0.123401821157026,
-1.59665523941937));
#21878=CARTESIAN_POINT('Ctrl Pts',(0.373030350867485,-0.166543350814306,
-1.60050712143809));
#21879=CARTESIAN_POINT('Ctrl Pts',(0.333298652394954,-0.237231147975234,
-1.60919314384089));
#21880=CARTESIAN_POINT('Ctrl Pts',(0.311480544243686,-0.266264900654909,
-1.61365775139403));
#21881=CARTESIAN_POINT('Ctrl Pts',(0.261368388670537,-0.317195968905306,
-1.62252828437015));
#21882=CARTESIAN_POINT('Ctrl Pts',(0.233069203882014,-0.33909093068465,
-1.62691869420078));
#21883=CARTESIAN_POINT('Ctrl Pts',(0.174042761838763,-0.373586846396559,
-1.63426473152765));
#21884=CARTESIAN_POINT('Ctrl Pts',(0.140365781471549,-0.388086240756494,
-1.63761964365402));
#21885=CARTESIAN_POINT('Ctrl Pts',(0.0701778381840612,-0.407068917407805,
-1.64212536811722));
#21886=CARTESIAN_POINT('Ctrl Pts',(0.0336652739555916,-0.411552957311693,
-1.643248));
#21887=CARTESIAN_POINT('Ctrl Pts',(-0.0336652739555915,-0.411552957311693,
-1.643248));
#21888=CARTESIAN_POINT('Ctrl Pts',(-0.0701778381840612,-0.407068917407805,
-1.64212536811722));
#21889=CARTESIAN_POINT('Ctrl Pts',(-0.140365781471549,-0.388086240756494,
-1.63761964365402));
#21890=CARTESIAN_POINT('Ctrl Pts',(-0.174042761838764,-0.373586846396559,
-1.63426473152765));
#21891=CARTESIAN_POINT('Ctrl Pts',(-0.233069203882014,-0.33909093068465,
-1.62691869420078));
#21892=CARTESIAN_POINT('Ctrl Pts',(-0.261368388670536,-0.317195968905306,
-1.62252828437015));
#21893=CARTESIAN_POINT('Ctrl Pts',(-0.311480544243686,-0.266264900654908,
-1.61365775139403));
#21894=CARTESIAN_POINT('Ctrl Pts',(-0.333298652394954,-0.237231147975234,
-1.60919314384089));
#21895=CARTESIAN_POINT('Ctrl Pts',(-0.373030350867485,-0.166543350814306,
-1.60050712143809));
#21896=CARTESIAN_POINT('Ctrl Pts',(-0.388626558458099,-0.123401821157026,
-1.59665523941937));
#21897=CARTESIAN_POINT('Ctrl Pts',(-0.397005914195118,-0.07938,-1.59456899932179));
#21898=CARTESIAN_POINT('Origin',(1.11022302462516E-16,-0.07938,-1.675));
#21899=CARTESIAN_POINT('Origin',(0.,-0.07938,0.));
#21900=CARTESIAN_POINT('',(0.846804978391753,-0.07938,-1.40825612658882));
#21901=CARTESIAN_POINT('Origin',(0.,-0.07938,0.));
#21902=CARTESIAN_POINT('Origin',(1.18440385848747,-0.07938,-1.18440385848747));
#21903=CARTESIAN_POINT('Origin',(1.18440385848747,0.,-1.18440385848747));
#21904=CARTESIAN_POINT('',(1.40825612658882,-0.07938,-0.846804978391753));
#21905=CARTESIAN_POINT('Ctrl Pts',(1.40825612658882,-0.0793800000000001,
-0.846804978391753));
#21906=CARTESIAN_POINT('Ctrl Pts',(1.40380622184538,-0.123401821157026,
-0.854205272175555));
#21907=CARTESIAN_POINT('Ctrl Pts',(1.39550172959303,-0.166543350814306,
-0.867957148219442));
#21908=CARTESIAN_POINT('Ctrl Pts',(1.3735491215176,-0.237231147975234,-0.902193646979983));
#21909=CARTESIAN_POINT('Ctrl Pts',(1.36127834356734,-0.266264900654908,
-0.920778333482565));
#21910=CARTESIAN_POINT('Ctrl Pts',(1.33211611256184,-0.317195968905306,
-0.962485392528369));
#21911=CARTESIAN_POINT('Ctrl Pts',(1.31521005565926,-0.33909093068465,-0.985600426557816));
#21912=CARTESIAN_POINT('Ctrl Pts',(1.27866649102984,-0.373586846396559,
-1.03253285680459));
#21913=CARTESIAN_POINT('Ctrl Pts',(1.25722555095714,-0.388086240756494,
-1.05871835910697));
#21914=CARTESIAN_POINT('Ctrl Pts',(1.2107812086231,-0.407068917407805,-1.11153475808518));
#21915=CARTESIAN_POINT('Ctrl Pts',(1.18575674747573,-0.411552957311693,
-1.13814686046673));
#21916=CARTESIAN_POINT('Ctrl Pts',(1.13814686046673,-0.411552957311693,
-1.18575674747573));
#21917=CARTESIAN_POINT('Ctrl Pts',(1.11153475808518,-0.407068917407805,
-1.2107812086231));
#21918=CARTESIAN_POINT('Ctrl Pts',(1.05871835910697,-0.388086240756494,
-1.25722555095714));
#21919=CARTESIAN_POINT('Ctrl Pts',(1.03253285680459,-0.373586846396559,
-1.27866649102984));
#21920=CARTESIAN_POINT('Ctrl Pts',(0.985600426557816,-0.33909093068465,
-1.31521005565926));
#21921=CARTESIAN_POINT('Ctrl Pts',(0.962485392528369,-0.317195968905306,
-1.33211611256184));
#21922=CARTESIAN_POINT('Ctrl Pts',(0.920778333482565,-0.266264900654909,
-1.36127834356734));
#21923=CARTESIAN_POINT('Ctrl Pts',(0.902193646979983,-0.237231147975234,
-1.3735491215176));
#21924=CARTESIAN_POINT('Ctrl Pts',(0.867957148219442,-0.166543350814306,
-1.39550172959303));
#21925=CARTESIAN_POINT('Ctrl Pts',(0.854205272175555,-0.123401821157026,
-1.40380622184538));
#21926=CARTESIAN_POINT('Ctrl Pts',(0.846804978391753,-0.0793800000000001,
-1.40825612658882));
#21927=CARTESIAN_POINT('Origin',(1.18440385848747,-0.07938,-1.18440385848747));
#21928=CARTESIAN_POINT('Origin',(0.,-0.27783,0.));
#21929=CARTESIAN_POINT('',(-1.643248,-0.47628,2.01239840340529E-16));
#21930=CARTESIAN_POINT('Origin',(0.,-0.47628,0.));
#21931=CARTESIAN_POINT('',(-1.643248,-0.27783,2.01239840340529E-16));
#21932=CARTESIAN_POINT('',(1.59456899932179,-0.07938,0.397005914195118));
#21933=CARTESIAN_POINT('Origin',(0.,-0.07938,0.));
#21934=CARTESIAN_POINT('',(1.59456899932179,-0.07938,-0.397005914195118));
#21935=CARTESIAN_POINT('Ctrl Pts',(1.59456899932179,-0.0793800000000001,
0.397005914195118));
#21936=CARTESIAN_POINT('Ctrl Pts',(1.59665523941937,-0.123401821157026,
0.388626558458099));
#21937=CARTESIAN_POINT('Ctrl Pts',(1.60050712143809,-0.166543350814306,
0.373030350867485));
#21938=CARTESIAN_POINT('Ctrl Pts',(1.60919314384089,-0.237231147975234,
0.333298652394954));
#21939=CARTESIAN_POINT('Ctrl Pts',(1.61365775139403,-0.266264900654909,
0.311480544243686));
#21940=CARTESIAN_POINT('Ctrl Pts',(1.62252828437015,-0.317195968905306,
0.261368388670537));
#21941=CARTESIAN_POINT('Ctrl Pts',(1.62691869420078,-0.33909093068465,0.233069203882014));
#21942=CARTESIAN_POINT('Ctrl Pts',(1.63426473152765,-0.373586846396559,
0.174042761838764));
#21943=CARTESIAN_POINT('Ctrl Pts',(1.63761964365402,-0.388086240756494,
0.140365781471549));
#21944=CARTESIAN_POINT('Ctrl Pts',(1.64212536811722,-0.407068917407805,
0.0701778381840612));
#21945=CARTESIAN_POINT('Ctrl Pts',(1.643248,-0.411552957311693,0.0336652739555916));
#21946=CARTESIAN_POINT('Ctrl Pts',(1.643248,-0.411552957311693,-0.0336652739555916));
#21947=CARTESIAN_POINT('Ctrl Pts',(1.64212536811722,-0.407068917407805,
-0.0701778381840612));
#21948=CARTESIAN_POINT('Ctrl Pts',(1.63761964365402,-0.388086240756494,
-0.140365781471549));
#21949=CARTESIAN_POINT('Ctrl Pts',(1.63426473152765,-0.373586846396559,
-0.174042761838764));
#21950=CARTESIAN_POINT('Ctrl Pts',(1.62691869420078,-0.33909093068465,-0.233069203882014));
#21951=CARTESIAN_POINT('Ctrl Pts',(1.62252828437015,-0.317195968905306,
-0.261368388670537));
#21952=CARTESIAN_POINT('Ctrl Pts',(1.61365775139403,-0.266264900654909,
-0.311480544243686));
#21953=CARTESIAN_POINT('Ctrl Pts',(1.60919314384089,-0.237231147975234,
-0.333298652394954));
#21954=CARTESIAN_POINT('Ctrl Pts',(1.60050712143809,-0.166543350814306,
-0.373030350867485));
#21955=CARTESIAN_POINT('Ctrl Pts',(1.59665523941937,-0.123401821157026,
-0.388626558458099));
#21956=CARTESIAN_POINT('Ctrl Pts',(1.59456899932179,-0.07938,-0.397005914195118));
#21957=CARTESIAN_POINT('Origin',(0.,-0.07938,0.));
#21958=CARTESIAN_POINT('Origin',(0.,-0.07938,0.));
#21959=CARTESIAN_POINT('Origin',(1.675,-0.07938,0.));
#21960=CARTESIAN_POINT('Origin',(1.675,0.,0.));
#21961=CARTESIAN_POINT('Origin',(1.675,-0.07938,0.));
#21962=CARTESIAN_POINT('Origin',(0.,-0.47628,0.));
#21963=CARTESIAN_POINT('Origin',(0.,-0.07938,0.));
#21964=CARTESIAN_POINT('',(0.,0.,0.));
#21965=CARTESIAN_POINT('Origin',(1.70469,0.695,0.));
#21966=CARTESIAN_POINT('',(-1.70469,0.695,-2.0876431520385E-16));
#21967=CARTESIAN_POINT('Origin',(0.,0.695,0.));
#21968=CARTESIAN_POINT('',(-1.65031,0.695,-2.02104685910087E-16));
#21969=CARTESIAN_POINT('Origin',(0.,0.695,0.));
#21970=CARTESIAN_POINT('Origin',(0.,0.6575,0.));
#21971=CARTESIAN_POINT('',(-1.70469,0.62,-2.0876431520385E-16));
#21972=CARTESIAN_POINT('Origin',(0.,0.62,0.));
#21973=CARTESIAN_POINT('',(-1.70469,0.6575,-2.0876431520385E-16));
#21974=CARTESIAN_POINT('Origin',(1.65031,0.62,0.));
#21975=CARTESIAN_POINT('',(-1.65031,0.62,-2.02104685910087E-16));
#21976=CARTESIAN_POINT('Origin',(0.,0.62,0.));
#21977=CARTESIAN_POINT('Origin',(0.,0.6575,0.));
#21978=CARTESIAN_POINT('',(-1.65031,0.6575,-2.02104685910087E-16));
#21979=CARTESIAN_POINT('Origin',(1.70469,-0.62,0.));
#21980=CARTESIAN_POINT('',(-1.70469,-0.62,-2.0876431520385E-16));
#21981=CARTESIAN_POINT('Origin',(0.,-0.62,0.));
#21982=CARTESIAN_POINT('',(-1.65031,-0.62,-2.02104685910087E-16));
#21983=CARTESIAN_POINT('Origin',(0.,-0.62,0.));
#21984=CARTESIAN_POINT('Origin',(0.,-0.6575,0.));
#21985=CARTESIAN_POINT('',(-1.70469,-0.695,-2.0876431520385E-16));
#21986=CARTESIAN_POINT('Origin',(0.,-0.695,0.));
#21987=CARTESIAN_POINT('',(-1.70469,-0.6575,-2.0876431520385E-16));
#21988=CARTESIAN_POINT('Origin',(1.65031,-0.695,0.));
#21989=CARTESIAN_POINT('',(-1.65031,-0.695,-2.02104685910087E-16));
#21990=CARTESIAN_POINT('Origin',(0.,-0.695,0.));
#21991=CARTESIAN_POINT('Origin',(0.,-0.6575,0.));
#21992=CARTESIAN_POINT('',(-1.65031,-0.6575,-2.02104685910087E-16));
#21993=CARTESIAN_POINT('',(0.,0.,0.));
#21994=CARTESIAN_POINT('',(0.,0.,0.));
#21995=CARTESIAN_POINT('',(0.,0.,0.));
#21996=CARTESIAN_POINT('',(0.,0.,0.));
#21997=CARTESIAN_POINT('',(0.,0.,0.));
#21998=CARTESIAN_POINT('',(0.,0.,0.));
#21999=CARTESIAN_POINT('',(0.,0.,0.));
#22000=CARTESIAN_POINT('Origin',(0.,0.,14.1));
#22001=CARTESIAN_POINT('',(-0.165,-2.02066721859313E-17,14.1));
#22002=CARTESIAN_POINT('Origin',(0.,0.,14.1));
#22003=CARTESIAN_POINT('',(-0.165,2.02066721859313E-17,15.));
#22004=CARTESIAN_POINT('',(-0.165,-2.02066721859313E-17,14.1));
#22005=CARTESIAN_POINT('Origin',(0.,0.,15.));
#22006=CARTESIAN_POINT('Origin',(0.,0.,14.1));
#22007=CARTESIAN_POINT('Origin',(-0.2,0.7,11.8));
#22008=CARTESIAN_POINT('',(-0.2,0.565685424949238,13.2));
#22009=CARTESIAN_POINT('',(-0.2,0.565685424949238,11.8));
#22010=CARTESIAN_POINT('',(-0.2,0.565685424949238,5.));
#22011=CARTESIAN_POINT('',(-0.2,0.35,13.2));
#22012=CARTESIAN_POINT('',(-0.2,0.35,13.2));
#22013=CARTESIAN_POINT('',(-0.2,0.35,11.8));
#22014=CARTESIAN_POINT('',(-0.2,0.35,11.8));
#22015=CARTESIAN_POINT('',(-0.2,0.35,11.8));
#22016=CARTESIAN_POINT('Origin',(0.,0.525,11.8));
#22017=CARTESIAN_POINT('',(0.2,0.565685424949238,11.8));
#22018=CARTESIAN_POINT('Origin',(0.,0.,11.8));
#22019=CARTESIAN_POINT('',(0.2,0.35,11.8));
#22020=CARTESIAN_POINT('',(0.2,0.35,11.8));
#22021=CARTESIAN_POINT('',(0.2,0.7,11.8));
#22022=CARTESIAN_POINT('Origin',(-0.2,0.35,11.8));
#22023=CARTESIAN_POINT('',(0.2,0.35,13.2));
#22024=CARTESIAN_POINT('',(0.2,0.35,13.2));
#22025=CARTESIAN_POINT('',(0.2,0.35,11.8));
#22026=CARTESIAN_POINT('Origin',(0.2,0.35,11.8));
#22027=CARTESIAN_POINT('',(0.2,0.565685424949238,13.2));
#22028=CARTESIAN_POINT('',(0.2,0.565685424949238,5.));
#22029=CARTESIAN_POINT('',(0.2,0.7,13.2));
#22030=CARTESIAN_POINT('Origin',(0.,0.525,13.2));
#22031=CARTESIAN_POINT('Origin',(0.,0.,13.2));
#22032=CARTESIAN_POINT('Origin',(0.,0.,11.));
#22033=CARTESIAN_POINT('',(-0.8,-9.79717439317883E-17,11.));
#22034=CARTESIAN_POINT('Origin',(0.,0.,11.));
#22035=CARTESIAN_POINT('',(-0.6,-7.34788079488412E-17,11.));
#22036=CARTESIAN_POINT('Origin',(0.,0.,11.));
#22037=CARTESIAN_POINT('Origin',(0.,0.,9.));
#22038=CARTESIAN_POINT('',(-0.8,-9.79717439317883E-17,9.));
#22039=CARTESIAN_POINT('Origin',(0.,0.,9.));
#22040=CARTESIAN_POINT('',(-0.6,7.34788079488412E-17,9.));
#22041=CARTESIAN_POINT('Origin',(0.,0.,9.));
#22042=CARTESIAN_POINT('Origin',(0.,0.,9.));
#22043=CARTESIAN_POINT('',(-0.8,-9.79717439317883E-17,9.));
#22044=CARTESIAN_POINT('Origin',(0.,0.,5.));
#22045=CARTESIAN_POINT('',(-0.6,-7.34788079488412E-17,5.));
#22046=CARTESIAN_POINT('',(-0.6,-7.34788079488412E-17,5.));
#22047=CARTESIAN_POINT('Origin',(0.,0.,5.));
#22048=CARTESIAN_POINT('Origin',(0.,0.,5.));
#22049=CARTESIAN_POINT('',(-0.6,-7.34788079488412E-17,15.));
#22050=CARTESIAN_POINT('Origin',(0.,0.,15.));
#22051=CARTESIAN_POINT('',(-0.6,-7.34788079488412E-17,5.));
#22052=CARTESIAN_POINT('Origin',(0.,0.,15.));
#22053=CARTESIAN_POINT('Origin',(0.,0.,5.));
#22054=CARTESIAN_POINT('',(0.,0.,0.));
#22055=CARTESIAN_POINT('Origin',(0.,0.,7.));
#22056=CARTESIAN_POINT('',(-0.605,-7.40911313484149E-17,8.));
#22057=CARTESIAN_POINT('Origin',(0.,0.,8.));
#22058=CARTESIAN_POINT('',(-0.605,-7.40911313484149E-17,7.));
#22059=CARTESIAN_POINT('',(-0.605,-7.40911313484149E-17,7.));
#22060=CARTESIAN_POINT('Origin',(0.,0.,7.));
#22061=CARTESIAN_POINT('Origin',(0.,0.,7.));
#22062=CARTESIAN_POINT('',(-0.8,-9.79717439317883E-17,8.));
#22063=CARTESIAN_POINT('Origin',(0.,0.,8.));
#22064=CARTESIAN_POINT('',(-0.8,-9.79717439317883E-17,7.));
#22065=CARTESIAN_POINT('',(-0.8,-9.79717439317883E-17,7.));
#22066=CARTESIAN_POINT('Origin',(0.,0.,7.));
#22067=CARTESIAN_POINT('Origin',(0.,0.,8.));
#22068=CARTESIAN_POINT('Origin',(0.,0.,7.));
#22069=CARTESIAN_POINT('',(0.,0.,0.));
#22070=CARTESIAN_POINT('Origin',(0.,0.,14.2));
#22071=CARTESIAN_POINT('',(-0.605,-7.40911313484149E-17,15.));
#22072=CARTESIAN_POINT('Origin',(0.,0.,15.));
#22073=CARTESIAN_POINT('',(-0.605,-7.40911313484149E-17,14.2));
#22074=CARTESIAN_POINT('',(-0.605,-7.40911313484149E-17,14.2));
#22075=CARTESIAN_POINT('Origin',(0.,0.,14.2));
#22076=CARTESIAN_POINT('Origin',(0.,0.,14.2));
#22077=CARTESIAN_POINT('',(-0.8,-9.79717439317883E-17,15.));
#22078=CARTESIAN_POINT('Origin',(0.,0.,15.));
#22079=CARTESIAN_POINT('',(-0.8,-9.79717439317883E-17,14.2));
#22080=CARTESIAN_POINT('',(-0.8,-9.79717439317883E-17,14.2));
#22081=CARTESIAN_POINT('Origin',(0.,0.,14.2));
#22082=CARTESIAN_POINT('Origin',(0.,0.,15.));
#22083=CARTESIAN_POINT('Origin',(0.,0.,14.2));
#22084=CARTESIAN_POINT('',(0.,0.,0.));
#22085=CARTESIAN_POINT('Origin',(0.,0.,5.8));
#22086=CARTESIAN_POINT('',(-0.605,-7.40911313484149E-17,6.));
#22087=CARTESIAN_POINT('Origin',(0.,0.,6.));
#22088=CARTESIAN_POINT('',(-0.605,-7.40911313484149E-17,5.8));
#22089=CARTESIAN_POINT('',(-0.605,-7.40911313484149E-17,5.8));
#22090=CARTESIAN_POINT('Origin',(0.,0.,5.8));
#22091=CARTESIAN_POINT('Origin',(0.,0.,5.8));
#22092=CARTESIAN_POINT('',(-0.8,-9.79717439317883E-17,6.));
#22093=CARTESIAN_POINT('Origin',(0.,0.,6.));
#22094=CARTESIAN_POINT('',(-0.8,-9.79717439317883E-17,5.8));
#22095=CARTESIAN_POINT('',(-0.8,-9.79717439317883E-17,5.8));
#22096=CARTESIAN_POINT('Origin',(0.,0.,5.8));
#22097=CARTESIAN_POINT('Origin',(0.,0.,6.));
#22098=CARTESIAN_POINT('Origin',(0.,0.,5.8));
#22099=CARTESIAN_POINT('',(0.,0.,0.));
#22100=CARTESIAN_POINT('Origin',(0.59,0.,5.4));
#22101=CARTESIAN_POINT('',(0.59,0.133884278389959,5.30356349239007));
#22102=CARTESIAN_POINT('',(0.59,0.133884278389959,5.49643650760993));
#22103=CARTESIAN_POINT('',(0.59,0.133884278389959,5.));
#22104=CARTESIAN_POINT('Origin',(0.59,0.,5.4));
#22105=CARTESIAN_POINT('Origin',(1.19,0.,5.4));
#22106=CARTESIAN_POINT('',(1.19,-0.154596248337402,5.45766281297336));
#22107=CARTESIAN_POINT('',(1.19,-0.154596248337402,5.34233718702664));
#22108=CARTESIAN_POINT('',(1.19,-0.154596248337402,5.));
#22109=CARTESIAN_POINT('',(1.19,-2.02066721859313E-17,5.565));
#22110=CARTESIAN_POINT('Origin',(1.19,0.,5.4));
#22111=CARTESIAN_POINT('',(1.19,0.154596248337402,5.45766281297336));
#22112=CARTESIAN_POINT('Origin',(1.19,0.,5.4));
#22113=CARTESIAN_POINT('',(1.19,0.154596248337402,5.34233718702664));
#22114=CARTESIAN_POINT('',(1.19,0.154596248337402,5.));
#22115=CARTESIAN_POINT('Origin',(1.19,0.,5.4));
#22116=CARTESIAN_POINT('Origin',(0.59,0.,5.4));
#22117=CARTESIAN_POINT('',(0.59,-0.133884278389959,5.30356349239007));
#22118=CARTESIAN_POINT('Ctrl Pts',(0.59,-0.133884278389959,5.30356349239007));
#22119=CARTESIAN_POINT('Ctrl Pts',(0.591198403406107,-0.128603165341393,
5.29623164237676));
#22120=CARTESIAN_POINT('Ctrl Pts',(0.59244064128815,-0.122792448979943,
5.28944721118838));
#22121=CARTESIAN_POINT('Ctrl Pts',(0.596510641114135,-0.10208383195986,
5.2687385941683));
#22122=CARTESIAN_POINT('Ctrl Pts',(0.599544094983168,-0.0836002135946608,
5.2560565239921));
#22123=CARTESIAN_POINT('Ctrl Pts',(0.603817074382984,-0.0429774150042653,
5.23918438436621));
#22124=CARTESIAN_POINT('Ctrl Pts',(0.605,-0.0208299403327843,5.235));
#22125=CARTESIAN_POINT('Ctrl Pts',(0.605,0.0208299403327842,5.235));
#22126=CARTESIAN_POINT('Ctrl Pts',(0.603817074382984,0.0429774150042653,
5.23918438436621));
#22127=CARTESIAN_POINT('Ctrl Pts',(0.599544094983168,0.0836002135946608,
5.2560565239921));
#22128=CARTESIAN_POINT('Ctrl Pts',(0.596510641114135,0.10208383195986,5.2687385941683));
#22129=CARTESIAN_POINT('Ctrl Pts',(0.59244064128815,0.122792448979943,5.28944721118838));
#22130=CARTESIAN_POINT('Ctrl Pts',(0.591198403406107,0.128603165341393,
5.29623164237676));
#22131=CARTESIAN_POINT('Ctrl Pts',(0.59,0.133884278389959,5.30356349239007));
#22132=CARTESIAN_POINT('',(0.59,-0.133884278389959,5.49643650760993));
#22133=CARTESIAN_POINT('Origin',(0.59,0.,5.4));
#22134=CARTESIAN_POINT('',(0.605,2.8060580378524E-17,5.565));
#22135=CARTESIAN_POINT('Ctrl Pts',(0.605,7.63278329429795E-17,5.565));
#22136=CARTESIAN_POINT('Ctrl Pts',(0.605,-0.0208299403327841,5.565));
#22137=CARTESIAN_POINT('Ctrl Pts',(0.603817074382984,-0.0429774150042653,
5.5608156156338));
#22138=CARTESIAN_POINT('Ctrl Pts',(0.599544094983168,-0.0836002135946608,
5.5439434760079));
#22139=CARTESIAN_POINT('Ctrl Pts',(0.596510641114135,-0.10208383195986,
5.5312614058317));
#22140=CARTESIAN_POINT('Ctrl Pts',(0.59244064128815,-0.122792448979943,
5.51055278881162));
#22141=CARTESIAN_POINT('Ctrl Pts',(0.591198403406107,-0.128603165341393,
5.50376835762324));
#22142=CARTESIAN_POINT('Ctrl Pts',(0.59,-0.133884278389959,5.49643650760993));
#22143=CARTESIAN_POINT('',(0.59,-2.02066721859313E-17,5.565));
#22144=CARTESIAN_POINT('Ctrl Pts',(1.19,-0.154596248337401,5.34233718702664));
#22145=CARTESIAN_POINT('Ctrl Pts',(1.18909117046716,-0.161591936497431,
5.36109289956149));
#22146=CARTESIAN_POINT('Ctrl Pts',(1.18860212013945,-0.165,5.38111762795045));
#22147=CARTESIAN_POINT('Ctrl Pts',(1.18860212013945,-0.165,5.41888237204955));
#22148=CARTESIAN_POINT('Ctrl Pts',(1.18909117046716,-0.161591936497431,
5.43890710043851));
#22149=CARTESIAN_POINT('Ctrl Pts',(1.19,-0.154596248337402,5.45766281297336));
#22150=CARTESIAN_POINT('Ctrl Pts',(1.19,0.154596248337402,5.45766281297336));
#22151=CARTESIAN_POINT('Ctrl Pts',(1.18909117046841,0.161591936487821,5.43890710046428));
#22152=CARTESIAN_POINT('Ctrl Pts',(1.18860212013945,0.165,5.41888237204667));
#22153=CARTESIAN_POINT('Ctrl Pts',(1.18860212013945,0.165,5.4));
#22154=CARTESIAN_POINT('Ctrl Pts',(1.18860212013945,0.165,5.38111762795045));
#22155=CARTESIAN_POINT('Ctrl Pts',(1.18909117046716,0.161591936497431,5.36109289956149));
#22156=CARTESIAN_POINT('Ctrl Pts',(1.19,0.154596248337401,5.34233718702664));
#22157=CARTESIAN_POINT('Ctrl Pts',(0.59,0.133884278389959,5.49643650760993));
#22158=CARTESIAN_POINT('Ctrl Pts',(0.591198403406107,0.128603165341393,
5.50376835762324));
#22159=CARTESIAN_POINT('Ctrl Pts',(0.59244064128815,0.122792448979943,5.51055278881162));
#22160=CARTESIAN_POINT('Ctrl Pts',(0.596510641114135,0.10208383195986,5.5312614058317));
#22161=CARTESIAN_POINT('Ctrl Pts',(0.599544094983168,0.0836002135946608,
5.5439434760079));
#22162=CARTESIAN_POINT('Ctrl Pts',(0.603817074382984,0.0429774150042653,
5.5608156156338));
#22163=CARTESIAN_POINT('Ctrl Pts',(0.605,0.0208299403327841,5.565));
#22164=CARTESIAN_POINT('Ctrl Pts',(0.605,-7.63278329429795E-17,5.565));
#22165=CARTESIAN_POINT('Origin',(0.59,0.,5.4));
#22166=CARTESIAN_POINT('',(0.59,-0.133884278389959,5.));
#22167=CARTESIAN_POINT('Origin',(0.,0.,5.));
#22168=CARTESIAN_POINT('',(-0.605,-7.40911313484149E-17,5.8));
#22169=CARTESIAN_POINT('Origin',(0.,0.,5.8));
#22170=CARTESIAN_POINT('',(-0.605,-7.40911313484149E-17,5.));
#22171=CARTESIAN_POINT('',(-0.605,-7.40911313484149E-17,5.));
#22172=CARTESIAN_POINT('Origin',(0.,0.,5.));
#22173=CARTESIAN_POINT('Origin',(0.,0.,5.));
#22174=CARTESIAN_POINT('',(-1.2,-1.46957615897682E-16,5.8));
#22175=CARTESIAN_POINT('Origin',(0.,0.,5.8));
#22176=CARTESIAN_POINT('',(-1.2,-1.46957615897682E-16,5.));
#22177=CARTESIAN_POINT('',(-1.2,-1.46957615897682E-16,5.));
#22178=CARTESIAN_POINT('Origin',(0.,0.,5.));
#22179=CARTESIAN_POINT('Origin',(0.,0.,5.8));
#22180=CARTESIAN_POINT('Origin',(0.,0.,5.));
#22181=CARTESIAN_POINT('',(0.,0.,0.));
#22182=CARTESIAN_POINT('Origin',(-0.2,0.35,11.8));
#22183=CARTESIAN_POINT('',(0.2,0.35,11.8));
#22184=CARTESIAN_POINT('',(-0.2,0.35,11.8));
#22185=CARTESIAN_POINT('',(0.2,0.35,11.8));
#22186=CARTESIAN_POINT('',(0.2,0.35,13.2));
#22187=CARTESIAN_POINT('',(0.2,0.35,11.8));
#22188=CARTESIAN_POINT('',(-0.2,0.35,13.2));
#22189=CARTESIAN_POINT('',(0.2,0.35,13.2));
#22190=CARTESIAN_POINT('',(-0.2,0.35,11.8));
#22191=CARTESIAN_POINT('Origin',(-0.2,0.75,11.8));
#22192=CARTESIAN_POINT('',(-0.2,0.75,11.8));
#22193=CARTESIAN_POINT('',(-0.2,0.35,11.8));
#22194=CARTESIAN_POINT('',(-0.2,0.75,13.2));
#22195=CARTESIAN_POINT('',(-0.2,0.35,13.2));
#22196=CARTESIAN_POINT('',(-0.2,0.75,11.8));
#22197=CARTESIAN_POINT('Origin',(0.2,0.75,11.8));
#22198=CARTESIAN_POINT('',(0.2,0.75,11.8));
#22199=CARTESIAN_POINT('',(-0.2,0.75,11.8));
#22200=CARTESIAN_POINT('',(0.2,0.75,13.2));
#22201=CARTESIAN_POINT('',(-0.2,0.75,13.2));
#22202=CARTESIAN_POINT('',(0.2,0.75,11.8));
#22203=CARTESIAN_POINT('Origin',(0.2,0.35,11.8));
#22204=CARTESIAN_POINT('',(0.2,0.75,11.8));
#22205=CARTESIAN_POINT('',(0.2,0.75,13.2));
#22206=CARTESIAN_POINT('Origin',(0.,0.55,13.2));
#22207=CARTESIAN_POINT('Origin',(0.,0.55,11.8));
#22208=CARTESIAN_POINT('',(0.,0.,0.));
#22209=CARTESIAN_POINT('Origin',(0.,0.,15.));
#22210=CARTESIAN_POINT('',(-0.225,-2.75545529808154E-17,15.2));
#22211=CARTESIAN_POINT('Origin',(0.,0.,15.2));
#22212=CARTESIAN_POINT('',(-0.225,-2.75545529808154E-17,15.));
#22213=CARTESIAN_POINT('',(-0.225,-2.75545529808154E-17,15.));
#22214=CARTESIAN_POINT('Origin',(0.,0.,15.));
#22215=CARTESIAN_POINT('Origin',(0.,0.,15.));
#22216=CARTESIAN_POINT('',(-0.9,-1.10218211923262E-16,15.2));
#22217=CARTESIAN_POINT('Origin',(0.,0.,15.2));
#22218=CARTESIAN_POINT('',(-0.9,-1.10218211923262E-16,15.));
#22219=CARTESIAN_POINT('',(-0.9,-1.10218211923262E-16,15.));
#22220=CARTESIAN_POINT('Origin',(0.,0.,15.));
#22221=CARTESIAN_POINT('Origin',(0.,0.,15.2));
#22222=CARTESIAN_POINT('Origin',(0.,0.,15.));
#22223=CARTESIAN_POINT('',(0.,0.,0.));
#22224=CARTESIAN_POINT('Origin',(0.2,0.,0.));
#22225=CARTESIAN_POINT('',(0.2,2.2,-0.78));
#22226=CARTESIAN_POINT('',(0.2,2.2,-0.565685424949238));
#22227=CARTESIAN_POINT('',(0.2,2.2,0.));
#22228=CARTESIAN_POINT('',(0.2,-1.,-0.78));
#22229=CARTESIAN_POINT('',(0.2,0.,-0.78));
#22230=CARTESIAN_POINT('',(0.2,-1.,-0.565685424949238));
#22231=CARTESIAN_POINT('',(0.2,-1.,0.));
#22232=CARTESIAN_POINT('',(0.2,0.,-0.565685424949238));
#22233=CARTESIAN_POINT('Origin',(0.2,0.,-0.78));
#22234=CARTESIAN_POINT('',(-0.2,2.2,-0.78));
#22235=CARTESIAN_POINT('',(0.1,2.2,-0.78));
#22236=CARTESIAN_POINT('',(-0.2,-1.,-0.78));
#22237=CARTESIAN_POINT('',(-0.2,0.,-0.78));
#22238=CARTESIAN_POINT('',(0.1,-1.,-0.78));
#22239=CARTESIAN_POINT('Origin',(-0.2,0.,-0.78));
#22240=CARTESIAN_POINT('',(-0.2,2.2,-0.565685424949238));
#22241=CARTESIAN_POINT('',(-0.2,2.2,-0.39));
#22242=CARTESIAN_POINT('',(-0.2,-1.,-0.565685424949238));
#22243=CARTESIAN_POINT('',(-0.2,0.,-0.565685424949238));
#22244=CARTESIAN_POINT('',(-0.2,-1.,-0.39));
#22245=CARTESIAN_POINT('Origin',(0.,-1.,0.));
#22246=CARTESIAN_POINT('',(1.60662857109684,-1.,0.693717979106306));
#22247=CARTESIAN_POINT('',(1.5055822144029,-1.,0.892032620296856));
#22248=CARTESIAN_POINT('Origin',(0.,-1.,0.));
#22249=CARTESIAN_POINT('',(1.81978687191668,-1.,1.23627494547115));
#22250=CARTESIAN_POINT('Ctrl Pts',(1.5055822144029,-1.,0.892032620296856));
#22251=CARTESIAN_POINT('Ctrl Pts',(1.50980486806688,-1.,0.894452006964544));
#22252=CARTESIAN_POINT('Ctrl Pts',(1.51805569590094,-1.,0.899185047483511));
#22253=CARTESIAN_POINT('Ctrl Pts',(1.52984849887993,-1.,0.905967409625651));
#22254=CARTESIAN_POINT('Ctrl Pts',(1.54440491149498,-1.,0.914375919026456));
#22255=CARTESIAN_POINT('Ctrl Pts',(1.56065988578893,-1.,0.923832188944341));
#22256=CARTESIAN_POINT('Ctrl Pts',(1.57499388382243,-1.,0.932246680108685));
#22257=CARTESIAN_POINT('Ctrl Pts',(1.58744937487176,-1.,0.939646377893399));
#22258=CARTESIAN_POINT('Ctrl Pts',(1.59810042043673,-1.,0.946078063315257));
#22259=CARTESIAN_POINT('Ctrl Pts',(1.60706069896936,-1.,0.951613284356035));
#22260=CARTESIAN_POINT('Ctrl Pts',(1.61449324337085,-1.,0.956354422920671));
#22261=CARTESIAN_POINT('Ctrl Pts',(1.62061638140221,-1.,0.960438326101729));
#22262=CARTESIAN_POINT('Ctrl Pts',(1.62571930670187,-1.,0.964046107040536));
#22263=CARTESIAN_POINT('Ctrl Pts',(1.63013849959461,-1.,0.967387853230345));
#22264=CARTESIAN_POINT('Ctrl Pts',(1.63420665729798,-1.,0.970669715997509));
#22265=CARTESIAN_POINT('Ctrl Pts',(1.63820952658144,-1.,0.974066058287419));
#22266=CARTESIAN_POINT('Ctrl Pts',(1.64233990826687,-1.,0.977689794119417));
#22267=CARTESIAN_POINT('Ctrl Pts',(1.64665139190656,-1.,0.981562530939489));
#22268=CARTESIAN_POINT('Ctrl Pts',(1.65110016612638,-1.,0.985642622920821));
#22269=CARTESIAN_POINT('Ctrl Pts',(1.65559044289699,-1.,0.989855627854165));
#22270=CARTESIAN_POINT('Ctrl Pts',(1.66001553809947,-1.,0.994121836661306));
#22271=CARTESIAN_POINT('Ctrl Pts',(1.66430758030376,-1.,0.998389654952758));
#22272=CARTESIAN_POINT('Ctrl Pts',(1.66846059277303,-1.,1.00265091003727));
#22273=CARTESIAN_POINT('Ctrl Pts',(1.67250335383293,-1.,1.00692206696414));
#22274=CARTESIAN_POINT('Ctrl Pts',(1.67648246776464,-1.,1.01123236493511));
#22275=CARTESIAN_POINT('Ctrl Pts',(1.68044289894798,-1.,1.01561026162773));
#22276=CARTESIAN_POINT('Ctrl Pts',(1.68440578021706,-1.,1.02006795074201));
#22277=CARTESIAN_POINT('Ctrl Pts',(1.68836910178447,-1.,1.02460180535255));
#22278=CARTESIAN_POINT('Ctrl Pts',(1.69231840863458,-1.,1.02919977579147));
#22279=CARTESIAN_POINT('Ctrl Pts',(1.69623414782771,-1.,1.03384646003588));
#22280=CARTESIAN_POINT('Ctrl Pts',(1.70010052930962,-1.,1.03852922490789));
#22281=CARTESIAN_POINT('Ctrl Pts',(1.70391338707982,-1.,1.04324363334554));
#22282=CARTESIAN_POINT('Ctrl Pts',(1.70767646263649,-1.,1.04799085404995));
#22283=CARTESIAN_POINT('Ctrl Pts',(1.71139783543989,-1.,1.05277517202855));
#22284=CARTESIAN_POINT('Ctrl Pts',(1.7150865442702,-1.,1.05760163192479));
#22285=CARTESIAN_POINT('Ctrl Pts',(1.71874858456904,-1.,1.06247324680647));
#22286=CARTESIAN_POINT('Ctrl Pts',(1.72238500928453,-1.,1.06738966975462));
#22287=CARTESIAN_POINT('Ctrl Pts',(1.72599406198488,-1.,1.07234866990252));
#22288=CARTESIAN_POINT('Ctrl Pts',(1.72957248977424,-1.,1.0773470373727));
#22289=CARTESIAN_POINT('Ctrl Pts',(1.73311705663407,-1.,1.08238162784749));
#22290=CARTESIAN_POINT('Ctrl Pts',(1.73662628326091,-1.,1.08745056285427));
#22291=CARTESIAN_POINT('Ctrl Pts',(1.74010053962247,-1.,1.09255329056493));
#22292=CARTESIAN_POINT('Ctrl Pts',(1.74354119236208,-1.,1.09768999241226));
#22293=CARTESIAN_POINT('Ctrl Pts',(1.74695004214923,-1.,1.10286118991143));
#22294=CARTESIAN_POINT('Ctrl Pts',(1.7503286607592,-1.,1.10806728183007));
#22295=CARTESIAN_POINT('Ctrl Pts',(1.7536777209463,-1.,1.11330807582551));
#22296=CARTESIAN_POINT('Ctrl Pts',(1.75699720772105,-1.,1.11858293216763));
#22297=CARTESIAN_POINT('Ctrl Pts',(1.76028671825096,-1.,1.12389096855086));
#22298=CARTESIAN_POINT('Ctrl Pts',(1.7635457196617,-1.,1.12923123555075));
#22299=CARTESIAN_POINT('Ctrl Pts',(1.76677384551862,-1.,1.1346029180462));
#22300=CARTESIAN_POINT('Ctrl Pts',(1.76997111386769,-1.,1.14000548336975));
#22301=CARTESIAN_POINT('Ctrl Pts',(1.77313777896194,-1.,1.1454385822692));
#22302=CARTESIAN_POINT('Ctrl Pts',(1.7762742255701,-1.,1.15090197841515));
#22303=CARTESIAN_POINT('Ctrl Pts',(1.77938085564275,-1.,1.15639547194698));
#22304=CARTESIAN_POINT('Ctrl Pts',(1.78245795881009,-1.,1.16191881298499));
#22305=CARTESIAN_POINT('Ctrl Pts',(1.78550566040443,-1.,1.16747166312303));
#22306=CARTESIAN_POINT('Ctrl Pts',(1.78852398877616,-1.,1.17305363177328));
#22307=CARTESIAN_POINT('Ctrl Pts',(1.79151291552689,-1.,1.17866429440809));
#22308=CARTESIAN_POINT('Ctrl Pts',(1.79447240321515,-1.,1.18430321697432));
#22309=CARTESIAN_POINT('Ctrl Pts',(1.79740245923478,-1.,1.18996997934445));
#22310=CARTESIAN_POINT('Ctrl Pts',(1.80030314369879,-1.,1.19566418930242));
#22311=CARTESIAN_POINT('Ctrl Pts',(1.80317454838603,-1.,1.20138548938974));
#22312=CARTESIAN_POINT('Ctrl Pts',(1.80601678480707,-1.,1.20713356605475));
#22313=CARTESIAN_POINT('Ctrl Pts',(1.80882996917129,-1.,1.21290815708314));
#22314=CARTESIAN_POINT('Ctrl Pts',(1.81161420806656,-1.,1.21870906103557));
#22315=CARTESIAN_POINT('Ctrl Pts',(1.81436959210434,-1.,1.2245361330495));
#22316=CARTESIAN_POINT('Ctrl Pts',(1.8165508718364,-1.,1.2292186489137));
#22317=CARTESIAN_POINT('Ctrl Pts',(1.81817389921279,-1.,1.2327422452705));
#22318=CARTESIAN_POINT('Ctrl Pts',(1.81925017193666,-1.,1.23509651170476));
#22319=CARTESIAN_POINT('Ctrl Pts',(1.81978687191668,-1.,1.23627494547115));
#22320=CARTESIAN_POINT('',(1.73811241238545,-1.,1.34869019493419));
#22321=CARTESIAN_POINT('',(1.81978687191668,-1.,1.23627494547115));
#22322=CARTESIAN_POINT('',(1.31362392696032,-1.,1.15624053661742));
#22323=CARTESIAN_POINT('Ctrl Pts',(1.73811241238545,-1.,1.34869019493419));
#22324=CARTESIAN_POINT('Ctrl Pts',(1.73682580585691,-1.,1.34854391898045));
#22325=CARTESIAN_POINT('Ctrl Pts',(1.73425417885907,-1.,1.34824783112887));
#22326=CARTESIAN_POINT('Ctrl Pts',(1.7304014965394,-1.,1.34779309152035));
#22327=CARTESIAN_POINT('Ctrl Pts',(1.72527410680674,-1.,1.34716554819527));
#22328=CARTESIAN_POINT('Ctrl Pts',(1.7188807715049,-1.,1.34634568653227));
#22329=CARTESIAN_POINT('Ctrl Pts',(1.71250340686822,-1.,1.34549029589416));
#22330=CARTESIAN_POINT('Ctrl Pts',(1.70614212266738,-1.,1.34459924533831));
#22331=CARTESIAN_POINT('Ctrl Pts',(1.69979707754427,-1.,1.34367237124483));
#22332=CARTESIAN_POINT('Ctrl Pts',(1.6934684849687,-1.,1.34270948206319));
#22333=CARTESIAN_POINT('Ctrl Pts',(1.68715660868764,-1.,1.341710374848));
#22334=CARTESIAN_POINT('Ctrl Pts',(1.68086176030362,-1.,1.34067485185203));
#22335=CARTESIAN_POINT('Ctrl Pts',(1.67458429426086,-1.,1.3396027347034));
#22336=CARTESIAN_POINT('Ctrl Pts',(1.66832460783989,-1.,1.33849388654388));
#22337=CARTESIAN_POINT('Ctrl Pts',(1.66208312541983,-1.,1.33734820885262));
#22338=CARTESIAN_POINT('Ctrl Pts',(1.65586025952593,-1.,1.33616559745172));
#22339=CARTESIAN_POINT('Ctrl Pts',(1.6496563728683,-1.,1.33494590467993));
#22340=CARTESIAN_POINT('Ctrl Pts',(1.6434717485603,-1.,1.33368890676572));
#22341=CARTESIAN_POINT('Ctrl Pts',(1.63730653475089,-1.,1.33239425103724));
#22342=CARTESIAN_POINT('Ctrl Pts',(1.63116079730923,-1.,1.33106149345645));
#22343=CARTESIAN_POINT('Ctrl Pts',(1.62503464209797,-1.,1.3296901950568));
#22344=CARTESIAN_POINT('Ctrl Pts',(1.61892832270724,-1.,1.32828000610449));
#22345=CARTESIAN_POINT('Ctrl Pts',(1.6128423401575,-1.,1.32683074483356));
#22346=CARTESIAN_POINT('Ctrl Pts',(1.60677758290954,-1.,1.32534250785782));
#22347=CARTESIAN_POINT('Ctrl Pts',(1.60073511858687,-1.,1.32381550858256));
#22348=CARTESIAN_POINT('Ctrl Pts',(1.59471591079403,-1.,1.32224985747682));
#22349=CARTESIAN_POINT('Ctrl Pts',(1.58872057258245,-1.,1.32064537110892));
#22350=CARTESIAN_POINT('Ctrl Pts',(1.58274907898834,-1.,1.31900135021432));
#22351=CARTESIAN_POINT('Ctrl Pts',(1.5768005650559,-1.,1.31731642317187));
#22352=CARTESIAN_POINT('Ctrl Pts',(1.57087397835723,-1.,1.31558903860016));
#22353=CARTESIAN_POINT('Ctrl Pts',(1.56496872402353,-1.,1.31381795281002));
#22354=CARTESIAN_POINT('Ctrl Pts',(1.55908521254821,-1.,1.31200264341696));
#22355=CARTESIAN_POINT('Ctrl Pts',(1.55322568759481,-1.,1.31014393684222));
#22356=CARTESIAN_POINT('Ctrl Pts',(1.54739413957185,-1.,1.30824393907473));
#22357=CARTESIAN_POINT('Ctrl Pts',(1.54159462645432,-1.,1.30630475189556));
#22358=CARTESIAN_POINT('Ctrl Pts',(1.53582981268977,-1.,1.30432735639489));
#22359=CARTESIAN_POINT('Ctrl Pts',(1.53009970283891,-1.,1.30231064395568));
#22360=CARTESIAN_POINT('Ctrl Pts',(1.52439957861062,-1.,1.30024984366328));
#22361=CARTESIAN_POINT('Ctrl Pts',(1.51872184912724,-1.,1.29813791800747));
#22362=CARTESIAN_POINT('Ctrl Pts',(1.51305994241402,-1.,1.29596850710509));
#22363=CARTESIAN_POINT('Ctrl Pts',(1.50741159078365,-1.,1.29373841372842));
#22364=CARTESIAN_POINT('Ctrl Pts',(1.50178230149776,-1.,1.29145022885181));
#22365=CARTESIAN_POINT('Ctrl Pts',(1.49618896881754,-1.,1.28911506584254));
#22366=CARTESIAN_POINT('Ctrl Pts',(1.4906522831278,-1.,1.2867467611644));
#22367=CARTESIAN_POINT('Ctrl Pts',(1.4851881711891,-1.,1.28435533880201));
#22368=CARTESIAN_POINT('Ctrl Pts',(1.47980070347095,-1.,1.28194158939517));
#22369=CARTESIAN_POINT('Ctrl Pts',(1.4744717526707,-1.,1.2794891824849));
#22370=CARTESIAN_POINT('Ctrl Pts',(1.46916035917133,-1.,1.2769641483109));
#22371=CARTESIAN_POINT('Ctrl Pts',(1.46382431332476,-1.,1.27433119897822));
#22372=CARTESIAN_POINT('Ctrl Pts',(1.45843906294697,-1.,1.27156805265289));
#22373=CARTESIAN_POINT('Ctrl Pts',(1.45301422764247,-1.,1.2686778680489));
#22374=CARTESIAN_POINT('Ctrl Pts',(1.44761985001662,-1.,1.26570925118868));
#22375=CARTESIAN_POINT('Ctrl Pts',(1.44236470511303,-1.,1.26273903323859));
#22376=CARTESIAN_POINT('Ctrl Pts',(1.43734919180847,-1.,1.25983531012005));
#22377=CARTESIAN_POINT('Ctrl Pts',(1.43262645609691,-1.,1.25702687965755));
#22378=CARTESIAN_POINT('Ctrl Pts',(1.42815938799387,-1.,1.25426945222639));
#22379=CARTESIAN_POINT('Ctrl Pts',(1.42378102115575,-1.,1.2514145557001));
#22380=CARTESIAN_POINT('Ctrl Pts',(1.41923722596025,-1.,1.24824430986571));
#22381=CARTESIAN_POINT('Ctrl Pts',(1.41422913175179,-1.,1.24450600513056));
#22382=CARTESIAN_POINT('Ctrl Pts',(1.40845295531283,-1.,1.23994455029534));
#22383=CARTESIAN_POINT('Ctrl Pts',(1.40164708206106,-1.,1.23434087290423));
#22384=CARTESIAN_POINT('Ctrl Pts',(1.39361389568796,-1.,1.22752961899387));
#22385=CARTESIAN_POINT('Ctrl Pts',(1.38420564527715,-1.,1.21938737280852));
#22386=CARTESIAN_POINT('Ctrl Pts',(1.37331915607905,-1.,1.20982812925645));
#22387=CARTESIAN_POINT('Ctrl Pts',(1.36088705043885,-1.,1.1987959077932));
#22388=CARTESIAN_POINT('Ctrl Pts',(1.34687054001093,-1.,1.18625865667441));
#22389=CARTESIAN_POINT('Ctrl Pts',(1.33437539347008,-1.,1.17501305789857));
#22390=CARTESIAN_POINT('Ctrl Pts',(1.32428080721772,-1.,1.16589330093588));
#22391=CARTESIAN_POINT('Ctrl Pts',(1.31722977216397,-1.,1.15950888730809));
#22392=CARTESIAN_POINT('Ctrl Pts',(1.31362392696032,-1.,1.15624053661742));
#22393=CARTESIAN_POINT('',(1.15624053661742,-1.,1.31362392696033));
#22394=CARTESIAN_POINT('Origin',(0.,-1.,0.));
#22395=CARTESIAN_POINT('',(1.34869019493419,-1.,1.73811241238545));
#22396=CARTESIAN_POINT('Ctrl Pts',(1.15624053661742,-1.,1.31362392696033));
#22397=CARTESIAN_POINT('Ctrl Pts',(1.15950888730433,-1.,1.3172297721596));
#22398=CARTESIAN_POINT('Ctrl Pts',(1.16589330092532,-1.,1.32428080720544));
#22399=CARTESIAN_POINT('Ctrl Pts',(1.17501305787994,-1.,1.33437539344842));
#22400=CARTESIAN_POINT('Ctrl Pts',(1.18625865664915,-1.,1.34687053998157));
#22401=CARTESIAN_POINT('Ctrl Pts',(1.1987959077656,-1.,1.36088705040677));
#22402=CARTESIAN_POINT('Ctrl Pts',(1.20982812923113,-1.,1.37331915604962));
#22403=CARTESIAN_POINT('Ctrl Pts',(1.21938737278853,-1.,1.38420564525391));
#22404=CARTESIAN_POINT('Ctrl Pts',(1.22752961898063,-1.,1.39361389567257));
#22405=CARTESIAN_POINT('Ctrl Pts',(1.23434087289768,-1.,1.40164708205345));
#22406=CARTESIAN_POINT('Ctrl Pts',(1.23994455029421,-1.,1.40845295531151));
#22407=CARTESIAN_POINT('Ctrl Pts',(1.24450600513278,-1.,1.41422913175437));
#22408=CARTESIAN_POINT('Ctrl Pts',(1.24824430986911,-1.,1.41923722596421));
#22409=CARTESIAN_POINT('Ctrl Pts',(1.25141455570299,-1.,1.42378102115911));
#22410=CARTESIAN_POINT('Ctrl Pts',(1.25426945222783,-1.,1.42815938799555));
#22411=CARTESIAN_POINT('Ctrl Pts',(1.25702687965744,-1.,1.43262645609679));
#22412=CARTESIAN_POINT('Ctrl Pts',(1.25983531011894,-1.,1.43734919180719));
#22413=CARTESIAN_POINT('Ctrl Pts',(1.26273903323723,-1.,1.44236470511145));
#22414=CARTESIAN_POINT('Ctrl Pts',(1.26570925118767,-1.,1.44761985001544));
#22415=CARTESIAN_POINT('Ctrl Pts',(1.26867786804854,-1.,1.45301422764205));
#22416=CARTESIAN_POINT('Ctrl Pts',(1.27156805265312,-1.,1.45843906294725));
#22417=CARTESIAN_POINT('Ctrl Pts',(1.27433119897877,-1.,1.4638243133254));
#22418=CARTESIAN_POINT('Ctrl Pts',(1.27696414831144,-1.,1.46916035917197));
#22419=CARTESIAN_POINT('Ctrl Pts',(1.27948918248524,-1.,1.4744717526711));
#22420=CARTESIAN_POINT('Ctrl Pts',(1.28194158939522,-1.,1.47980070347102));
#22421=CARTESIAN_POINT('Ctrl Pts',(1.28435533880184,-1.,1.48518817118891));
#22422=CARTESIAN_POINT('Ctrl Pts',(1.28674676116415,-1.,1.4906522831275));
#22423=CARTESIAN_POINT('Ctrl Pts',(1.28911506584232,-1.,1.49618896881729));
#22424=CARTESIAN_POINT('Ctrl Pts',(1.29145022885171,-1.,1.50178230149764));
#22425=CARTESIAN_POINT('Ctrl Pts',(1.29373841372843,-1.,1.50741159078367));
#22426=CARTESIAN_POINT('Ctrl Pts',(1.29596850710518,-1.,1.51305994241412));
#22427=CARTESIAN_POINT('Ctrl Pts',(1.29813791800757,-1.,1.51872184912735));
#22428=CARTESIAN_POINT('Ctrl Pts',(1.30024984366334,-1.,1.5243995786107));
#22429=CARTESIAN_POINT('Ctrl Pts',(1.3023106439557,-1.,1.53009970283893));
#22430=CARTESIAN_POINT('Ctrl Pts',(1.30432735639487,-1.,1.53582981268976));
#22431=CARTESIAN_POINT('Ctrl Pts',(1.30630475189553,-1.,1.54159462645428));
#22432=CARTESIAN_POINT('Ctrl Pts',(1.30824393907471,-1.,1.54739413957183));
#22433=CARTESIAN_POINT('Ctrl Pts',(1.31014393684221,-1.,1.55322568759481));
#22434=CARTESIAN_POINT('Ctrl Pts',(1.31200264341696,-1.,1.55908521254822));
#22435=CARTESIAN_POINT('Ctrl Pts',(1.31381795281002,-1.,1.56496872402352));
#22436=CARTESIAN_POINT('Ctrl Pts',(1.31558903860015,-1.,1.57087397835721));
#22437=CARTESIAN_POINT('Ctrl Pts',(1.31731642317183,-1.,1.57680056505585));
#22438=CARTESIAN_POINT('Ctrl Pts',(1.31900135021428,-1.,1.58274907898829));
#22439=CARTESIAN_POINT('Ctrl Pts',(1.32064537110891,-1.,1.58872057258244));
#22440=CARTESIAN_POINT('Ctrl Pts',(1.32224985747686,-1.,1.59471591079408));
#22441=CARTESIAN_POINT('Ctrl Pts',(1.32381550858266,-1.,1.600735118587));
#22442=CARTESIAN_POINT('Ctrl Pts',(1.32534250785794,-1.,1.6067775829097));
#22443=CARTESIAN_POINT('Ctrl Pts',(1.32683074483365,-1.,1.61284234015762));
#22444=CARTESIAN_POINT('Ctrl Pts',(1.32828000610448,-1.,1.61892832270723));
#22445=CARTESIAN_POINT('Ctrl Pts',(1.32969019505665,-1.,1.62503464209777));
#22446=CARTESIAN_POINT('Ctrl Pts',(1.33106149345618,-1.,1.63116079730887));
#22447=CARTESIAN_POINT('Ctrl Pts',(1.33239425103694,-1.,1.6373065347505));
#22448=CARTESIAN_POINT('Ctrl Pts',(1.33368890676554,-1.,1.64347174856007));
#22449=CARTESIAN_POINT('Ctrl Pts',(1.33494590468003,-1.,1.64965637286843));
#22450=CARTESIAN_POINT('Ctrl Pts',(1.33616559745217,-1.,1.65586025952651));
#22451=CARTESIAN_POINT('Ctrl Pts',(1.33734820885331,-1.,1.66208312542073));
#22452=CARTESIAN_POINT('Ctrl Pts',(1.33849388654458,-1.,1.66832460784078));
#22453=CARTESIAN_POINT('Ctrl Pts',(1.33960273470372,-1.,1.67458429426126));
#22454=CARTESIAN_POINT('Ctrl Pts',(1.3406748518516,-1.,1.68086176030308));
#22455=CARTESIAN_POINT('Ctrl Pts',(1.34171037484673,-1.,1.68715660868602));
#22456=CARTESIAN_POINT('Ctrl Pts',(1.34270948206139,-1.,1.6934684849664));
#22457=CARTESIAN_POINT('Ctrl Pts',(1.34367237124322,-1.,1.69979707754221));
#22458=CARTESIAN_POINT('Ctrl Pts',(1.34459924533783,-1.,1.70614212266676));
#22459=CARTESIAN_POINT('Ctrl Pts',(1.34549029589563,-1.,1.71250340687011));
#22460=CARTESIAN_POINT('Ctrl Pts',(1.34634568653586,-1.,1.7188807715095));
#22461=CARTESIAN_POINT('Ctrl Pts',(1.34716554820013,-1.,1.72527410681298));
#22462=CARTESIAN_POINT('Ctrl Pts',(1.3477930915247,-1.,1.73040149654497));
#22463=CARTESIAN_POINT('Ctrl Pts',(1.34824783113158,-1.,1.73425417886255));
#22464=CARTESIAN_POINT('Ctrl Pts',(1.34854391898145,-1.,1.73682580585819));
#22465=CARTESIAN_POINT('Ctrl Pts',(1.34869019493419,-1.,1.73811241238545));
#22466=CARTESIAN_POINT('',(1.23627494547115,-1.,1.81978687191668));
#22467=CARTESIAN_POINT('',(1.34869019493419,-1.,1.73811241238545));
#22468=CARTESIAN_POINT('',(0.892032620296855,-1.,1.5055822144029));
#22469=CARTESIAN_POINT('Ctrl Pts',(1.23627494547115,-1.,1.81978687191668));
#22470=CARTESIAN_POINT('Ctrl Pts',(1.23509651170384,-1.,1.81925017193531));
#22471=CARTESIAN_POINT('Ctrl Pts',(1.23274224526804,-1.,1.81817389920914));
#22472=CARTESIAN_POINT('Ctrl Pts',(1.22921864890975,-1.,1.81655087183054));
#22473=CARTESIAN_POINT('Ctrl Pts',(1.22453613304507,-1.,1.81436959209778));
#22474=CARTESIAN_POINT('Ctrl Pts',(1.2187090610323,-1.,1.81161420806172));
#22475=CARTESIAN_POINT('Ctrl Pts',(1.2129081570818,-1.,1.80882996916931));
#22476=CARTESIAN_POINT('Ctrl Pts',(1.20713356605519,-1.,1.80601678480772));
#22477=CARTESIAN_POINT('Ctrl Pts',(1.2013854893912,-1.,1.8031745483882));
#22478=CARTESIAN_POINT('Ctrl Pts',(1.19566418930405,-1.,1.80030314370121));
#22479=CARTESIAN_POINT('Ctrl Pts',(1.1899699793456,-1.,1.79740245923649));
#22480=CARTESIAN_POINT('Ctrl Pts',(1.18430321697471,-1.,1.79447240321572));
#22481=CARTESIAN_POINT('Ctrl Pts',(1.17866429440781,-1.,1.79151291552646));
#22482=CARTESIAN_POINT('Ctrl Pts',(1.17305363177265,-1.,1.78852398877523));
#22483=CARTESIAN_POINT('Ctrl Pts',(1.16747166312239,-1.,1.78550566040349));
#22484=CARTESIAN_POINT('Ctrl Pts',(1.16191881298458,-1.,1.78245795880949));
#22485=CARTESIAN_POINT('Ctrl Pts',(1.15639547194689,-1.,1.77938085564261));
#22486=CARTESIAN_POINT('Ctrl Pts',(1.15090197841531,-1.,1.77627422557034));
#22487=CARTESIAN_POINT('Ctrl Pts',(1.14543858226948,-1.,1.77313777896234));
#22488=CARTESIAN_POINT('Ctrl Pts',(1.14000548337,-1.,1.76997111386806));
#22489=CARTESIAN_POINT('Ctrl Pts',(1.13460291804634,-1.,1.76677384551883));
#22490=CARTESIAN_POINT('Ctrl Pts',(1.12923123555076,-1.,1.76354571966171));
#22491=CARTESIAN_POINT('Ctrl Pts',(1.12389096855078,-1.,1.76028671825084));
#22492=CARTESIAN_POINT('Ctrl Pts',(1.11858293216752,-1.,1.75699720772089));
#22493=CARTESIAN_POINT('Ctrl Pts',(1.11330807582542,-1.,1.75367772094617));
#22494=CARTESIAN_POINT('Ctrl Pts',(1.10806728183003,-1.,1.75032866075914));
#22495=CARTESIAN_POINT('Ctrl Pts',(1.10286118991144,-1.,1.74695004214924));
#22496=CARTESIAN_POINT('Ctrl Pts',(1.09768999241229,-1.,1.74354119236212));
#22497=CARTESIAN_POINT('Ctrl Pts',(1.09255329056496,-1.,1.74010053962252));
#22498=CARTESIAN_POINT('Ctrl Pts',(1.08745056285429,-1.,1.73662628326093));
#22499=CARTESIAN_POINT('Ctrl Pts',(1.08238162784749,-1.,1.73311705663407));
#22500=CARTESIAN_POINT('Ctrl Pts',(1.0773470373727,-1.,1.72957248977424));
#22501=CARTESIAN_POINT('Ctrl Pts',(1.07234866990252,-1.,1.72599406198489));
#22502=CARTESIAN_POINT('Ctrl Pts',(1.06738966975463,-1.,1.72238500928456));
#22503=CARTESIAN_POINT('Ctrl Pts',(1.06247324680649,-1.,1.71874858456908));
#22504=CARTESIAN_POINT('Ctrl Pts',(1.05760163192481,-1.,1.71508654427022));
#22505=CARTESIAN_POINT('Ctrl Pts',(1.05277517202853,-1.,1.71139783543986));
#22506=CARTESIAN_POINT('Ctrl Pts',(1.0479908540499,-1.,1.70767646263641));
#22507=CARTESIAN_POINT('Ctrl Pts',(1.04324363334546,-1.,1.70391338707969));
#22508=CARTESIAN_POINT('Ctrl Pts',(1.03852922490782,-1.,1.70010052930951));
#22509=CARTESIAN_POINT('Ctrl Pts',(1.03384646003587,-1.,1.69623414782769));
#22510=CARTESIAN_POINT('Ctrl Pts',(1.02919977579155,-1.,1.69231840863471));
#22511=CARTESIAN_POINT('Ctrl Pts',(1.02460180535272,-1.,1.68836910178475));
#22512=CARTESIAN_POINT('Ctrl Pts',(1.02006795074222,-1.,1.68440578021739));
#22513=CARTESIAN_POINT('Ctrl Pts',(1.01561026162786,-1.,1.6804428989482));
#22514=CARTESIAN_POINT('Ctrl Pts',(1.01123236493507,-1.,1.67648246776457));
#22515=CARTESIAN_POINT('Ctrl Pts',(1.00692206696387,-1.,1.67250335383248));
#22516=CARTESIAN_POINT('Ctrl Pts',(1.00265091003682,-1.,1.66846059277231));
#22517=CARTESIAN_POINT('Ctrl Pts',(0.998389654952317,-1.,1.66430758030304));
#22518=CARTESIAN_POINT('Ctrl Pts',(0.994121836661115,-1.,1.66001553809916));
#22519=CARTESIAN_POINT('Ctrl Pts',(0.98985562785445,-1.,1.65559044289746));
#22520=CARTESIAN_POINT('Ctrl Pts',(0.985642622921626,-1.,1.6511001661277));
#22521=CARTESIAN_POINT('Ctrl Pts',(0.981562530940574,-1.,1.64665139190834));
#22522=CARTESIAN_POINT('Ctrl Pts',(0.977689794120296,-1.,1.64233990826831));
#22523=CARTESIAN_POINT('Ctrl Pts',(0.974066058287501,-1.,1.63820952658157));
#22524=CARTESIAN_POINT('Ctrl Pts',(0.970669715996356,-1.,1.63420665729609));
#22525=CARTESIAN_POINT('Ctrl Pts',(0.967387853228041,-1.,1.63013849959083));
#22526=CARTESIAN_POINT('Ctrl Pts',(0.964046107037821,-1.,1.6257193066974));
#22527=CARTESIAN_POINT('Ctrl Pts',(0.960438326099958,-1.,1.62061638139929));
#22528=CARTESIAN_POINT('Ctrl Pts',(0.956354422921572,-1.,1.61449324337233));
#22529=CARTESIAN_POINT('Ctrl Pts',(0.951613284361247,-1.,1.60706069897794));
#22530=CARTESIAN_POINT('Ctrl Pts',(0.946078063325795,-1.,1.59810042045408));
#22531=CARTESIAN_POINT('Ctrl Pts',(0.939646377909319,-1.,1.58744937489796));
#22532=CARTESIAN_POINT('Ctrl Pts',(0.932246680128848,-1.,1.57499388385561));
#22533=CARTESIAN_POINT('Ctrl Pts',(0.923832188966322,-1.,1.56065988582509));
#22534=CARTESIAN_POINT('Ctrl Pts',(0.914375919046579,-1.,1.54440491152808));
#22535=CARTESIAN_POINT('Ctrl Pts',(0.905967409640498,-1.,1.52984849890434));
#22536=CARTESIAN_POINT('Ctrl Pts',(0.89918504749193,-1.,1.51805569591479));
#22537=CARTESIAN_POINT('Ctrl Pts',(0.894452006967538,-1.,1.50980486807181));
#22538=CARTESIAN_POINT('Ctrl Pts',(0.892032620296855,-1.,1.5055822144029));
#22539=CARTESIAN_POINT('',(0.693717979106305,-1.,1.60662857109684));
#22540=CARTESIAN_POINT('Origin',(0.,-1.,0.));
#22541=CARTESIAN_POINT('',(0.7455743247944,-1.,2.0698113262342));
#22542=CARTESIAN_POINT('Ctrl Pts',(0.693717979106305,-1.,1.60662857109684));
#22543=CARTESIAN_POINT('Ctrl Pts',(0.69571209787897,-1.,1.61106790957619));
#22544=CARTESIAN_POINT('Ctrl Pts',(0.699605146398836,-1.,1.61974673471117));
#22545=CARTESIAN_POINT('Ctrl Pts',(0.705159151977294,-1.,1.6321654166204));
#22546=CARTESIAN_POINT('Ctrl Pts',(0.711993139340447,-1.,1.64752408828442));
#22547=CARTESIAN_POINT('Ctrl Pts',(0.719585433787949,-1.,1.66472880551777));
#22548=CARTESIAN_POINT('Ctrl Pts',(0.726235967982445,-1.,1.67996158451922));
#22549=CARTESIAN_POINT('Ctrl Pts',(0.731963238685357,-1.,1.69326921972915));
#22550=CARTESIAN_POINT('Ctrl Pts',(0.736799665716932,-1.,1.70473309004249));
#22551=CARTESIAN_POINT('Ctrl Pts',(0.74079516202821,-1.,1.71447789751001));
#22552=CARTESIAN_POINT('Ctrl Pts',(0.744021445433093,-1.,1.72268229916769));
#22553=CARTESIAN_POINT('Ctrl Pts',(0.746574710097752,-1.,1.72958533647714));
#22554=CARTESIAN_POINT('Ctrl Pts',(0.74858246295687,-1.,1.7355035168033));
#22555=CARTESIAN_POINT('Ctrl Pts',(0.750193435981249,-1.,1.74080458267114));
#22556=CARTESIAN_POINT('Ctrl Pts',(0.751555614164482,-1.,1.74585086852502));
#22557=CARTESIAN_POINT('Ctrl Pts',(0.752797683531314,-1.,1.75095139468794));
#22558=CARTESIAN_POINT('Ctrl Pts',(0.754009254027828,-1.,1.75631083600019));
#22559=CARTESIAN_POINT('Ctrl Pts',(0.755220979974461,-1.,1.76197817240128));
#22560=CARTESIAN_POINT('Ctrl Pts',(0.75642189602781,-1.,1.76789396002998));
#22561=CARTESIAN_POINT('Ctrl Pts',(0.757578264077028,-1.,1.77394167108292));
#22562=CARTESIAN_POINT('Ctrl Pts',(0.758650626677518,-1.,1.77999411220945));
#22563=CARTESIAN_POINT('Ctrl Pts',(0.759614401110189,-1.,1.78596964884604));
#22564=CARTESIAN_POINT('Ctrl Pts',(0.760469555880749,-1.,1.7918581561088));
#22565=CARTESIAN_POINT('Ctrl Pts',(0.761229695230558,-1.,1.79768986997783));
#22566=CARTESIAN_POINT('Ctrl Pts',(0.761915336443547,-1.,1.80351583877342));
#22567=CARTESIAN_POINT('Ctrl Pts',(0.762546129463938,-1.,1.80938551463965));
#22568=CARTESIAN_POINT('Ctrl Pts',(0.763132003836634,-1.,1.8153211840553));
#22569=CARTESIAN_POINT('Ctrl Pts',(0.763673465462726,-1.,1.82131873145266));
#22570=CARTESIAN_POINT('Ctrl Pts',(0.764165902605995,-1.,1.82735991200065));
#22571=CARTESIAN_POINT('Ctrl Pts',(0.764602549687853,-1.,1.83342077227142));
#22572=CARTESIAN_POINT('Ctrl Pts',(0.764978057881737,-1.,1.83948181064835));
#22573=CARTESIAN_POINT('Ctrl Pts',(0.765291664862029,-1.,1.84553698875924));
#22574=CARTESIAN_POINT('Ctrl Pts',(0.765545710619062,-1.,1.85158945130063));
#22575=CARTESIAN_POINT('Ctrl Pts',(0.765744212909318,-1.,1.85764741390394));
#22576=CARTESIAN_POINT('Ctrl Pts',(0.765891519092547,-1.,1.86372027063312));
#22577=CARTESIAN_POINT('Ctrl Pts',(0.765990708546091,-1.,1.86981398314341));
#22578=CARTESIAN_POINT('Ctrl Pts',(0.766042837036744,-1.,1.87592888967883));
#22579=CARTESIAN_POINT('Ctrl Pts',(0.766047794851864,-1.,1.88206215302561));
#22580=CARTESIAN_POINT('Ctrl Pts',(0.766004837062091,-1.,1.88820926433409));
#22581=CARTESIAN_POINT('Ctrl Pts',(0.765913193856978,-1.,1.89436577771388));
#22582=CARTESIAN_POINT('Ctrl Pts',(0.765772772593386,-1.,1.90052930393596));
#22583=CARTESIAN_POINT('Ctrl Pts',(0.765584196937919,-1.,1.90669961402356));
#22584=CARTESIAN_POINT('Ctrl Pts',(0.765348465884722,-1.,1.91287765805169));
#22585=CARTESIAN_POINT('Ctrl Pts',(0.765066729667088,-1.,1.91906491634196));
#22586=CARTESIAN_POINT('Ctrl Pts',(0.764740025488211,-1.,1.92526263537048));
#22587=CARTESIAN_POINT('Ctrl Pts',(0.76436901067394,-1.,1.93147105496382));
#22588=CARTESIAN_POINT('Ctrl Pts',(0.763954049121458,-1.,1.93768964875886));
#22589=CARTESIAN_POINT('Ctrl Pts',(0.763495333538629,-1.,1.9439174661764));
#22590=CARTESIAN_POINT('Ctrl Pts',(0.762992990878769,-1.,1.95015342590024));
#22591=CARTESIAN_POINT('Ctrl Pts',(0.762447203806178,-1.,1.95639665309869));
#22592=CARTESIAN_POINT('Ctrl Pts',(0.761858300014423,-1.,1.96264672744186));
#22593=CARTESIAN_POINT('Ctrl Pts',(0.76122669048382,-1.,1.96890351582499));
#22594=CARTESIAN_POINT('Ctrl Pts',(0.760552825409757,-1.,1.97516705321494));
#22595=CARTESIAN_POINT('Ctrl Pts',(0.75983714745219,-1.,1.98143741418172));
#22596=CARTESIAN_POINT('Ctrl Pts',(0.759080037802488,-1.,1.98771456680874));
#22597=CARTESIAN_POINT('Ctrl Pts',(0.758281796766761,-1.,1.99399831098817));
#22598=CARTESIAN_POINT('Ctrl Pts',(0.757442676862724,-1.,2.00028834739178));
#22599=CARTESIAN_POINT('Ctrl Pts',(0.75656290464667,-1.,2.0065843158773));
#22600=CARTESIAN_POINT('Ctrl Pts',(0.755642704957865,-1.,2.01288584328084));
#22601=CARTESIAN_POINT('Ctrl Pts',(0.754682330722816,-1.,2.01919259405809));
#22602=CARTESIAN_POINT('Ctrl Pts',(0.753682061112768,-1.,2.02550428623313));
#22603=CARTESIAN_POINT('Ctrl Pts',(0.75264218048721,-1.,2.03182068456221));
#22604=CARTESIAN_POINT('Ctrl Pts',(0.751562963361115,-1.,2.03814160092099));
#22605=CARTESIAN_POINT('Ctrl Pts',(0.750444657875575,-1.,2.04446689147979));
#22606=CARTESIAN_POINT('Ctrl Pts',(0.749287468665046,-1.,2.05079645592154));
#22607=CARTESIAN_POINT('Ctrl Pts',(0.748091554183802,-1.,2.05713023031007));
#22608=CARTESIAN_POINT('Ctrl Pts',(0.747103932787919,-1.,2.06220058927826));
#22609=CARTESIAN_POINT('Ctrl Pts',(0.7463458715442,-1.,2.06600523016815));
#22610=CARTESIAN_POINT('Ctrl Pts',(0.745832791378367,-1.,2.06854248895728));
#22611=CARTESIAN_POINT('Ctrl Pts',(0.7455743247944,-1.,2.0698113262342));
#22612=CARTESIAN_POINT('',(0.61342227326009,-1.,2.11275013067528));
#22613=CARTESIAN_POINT('',(0.7455743247944,-1.,2.0698113262342));
#22614=CARTESIAN_POINT('',(0.383122945602004,-1.,1.7075470150345));
#22615=CARTESIAN_POINT('Ctrl Pts',(0.61342227326009,-1.,2.11275013067528));
#22616=CARTESIAN_POINT('Ctrl Pts',(0.6124673655618,-1.,2.11187554259986));
#22617=CARTESIAN_POINT('Ctrl Pts',(0.610560911689898,-1.,2.11012443807238));
#22618=CARTESIAN_POINT('Ctrl Pts',(0.607711315454876,-1.,2.1074919961518));
#22619=CARTESIAN_POINT('Ctrl Pts',(0.60393203073603,-1.,2.10397049886949));
#22620=CARTESIAN_POINT('Ctrl Pts',(0.599241616420533,-1.,2.0995493086477));
#22621=CARTESIAN_POINT('Ctrl Pts',(0.594585006052162,-1.,2.0951087622027));
#22622=CARTESIAN_POINT('Ctrl Pts',(0.589962365403406,-1.,2.09064881812129));
#22623=CARTESIAN_POINT('Ctrl Pts',(0.585373918991617,-1.,2.08616943727951));
#22624=CARTESIAN_POINT('Ctrl Pts',(0.580819952108063,-1.,2.08167059018418));
#22625=CARTESIAN_POINT('Ctrl Pts',(0.576300797416844,-1.,2.07715226767559));
#22626=CARTESIAN_POINT('Ctrl Pts',(0.571816823242602,-1.,2.07261449292824));
#22627=CARTESIAN_POINT('Ctrl Pts',(0.567368421181087,-1.,2.06805732997334));
#22628=CARTESIAN_POINT('Ctrl Pts',(0.562955993082261,-1.,2.06348090160589));
#22629=CARTESIAN_POINT('Ctrl Pts',(0.558579940185151,-1.,2.05888537756462));
#22630=CARTESIAN_POINT('Ctrl Pts',(0.554240657463906,-1.,2.05427091604413));
#22631=CARTESIAN_POINT('Ctrl Pts',(0.549938525150295,-1.,2.04963761077958));
#22632=CARTESIAN_POINT('Ctrl Pts',(0.54567390381743,-1.,2.04498544714588));
#22633=CARTESIAN_POINT('Ctrl Pts',(0.541447120615659,-1.,2.04031422690527));
#22634=CARTESIAN_POINT('Ctrl Pts',(0.537258489833262,-1.,2.03562362954037));
#22635=CARTESIAN_POINT('Ctrl Pts',(0.533108355132976,-1.,2.03091336214426));
#22636=CARTESIAN_POINT('Ctrl Pts',(0.528997127241914,-1.,2.0261832908329));
#22637=CARTESIAN_POINT('Ctrl Pts',(0.524925318333476,-1.,2.02143356304698));
#22638=CARTESIAN_POINT('Ctrl Pts',(0.52089359039937,-1.,2.01666477917286));
#22639=CARTESIAN_POINT('Ctrl Pts',(0.516902681728687,-1.,2.01187773939242));
#22640=CARTESIAN_POINT('Ctrl Pts',(0.512953306961792,-1.,2.00707309946949));
#22641=CARTESIAN_POINT('Ctrl Pts',(0.509046069886157,-1.,2.00225107134734));
#22642=CARTESIAN_POINT('Ctrl Pts',(0.505181361323026,-1.,1.99741107463572));
#22643=CARTESIAN_POINT('Ctrl Pts',(0.501359287727146,-1.,1.99255149126155));
#22644=CARTESIAN_POINT('Ctrl Pts',(0.497579909545574,-1.,1.98767044752932));
#22645=CARTESIAN_POINT('Ctrl Pts',(0.493843476541494,-1.,1.98276658761821));
#22646=CARTESIAN_POINT('Ctrl Pts',(0.490150627860952,-1.,1.97783973019229));
#22647=CARTESIAN_POINT('Ctrl Pts',(0.486502692907658,-1.,1.97289186263272));
#22648=CARTESIAN_POINT('Ctrl Pts',(0.48290166212069,-1.,1.96792703422362));
#22649=CARTESIAN_POINT('Ctrl Pts',(0.479349583074855,-1.,1.96294933055943));
#22650=CARTESIAN_POINT('Ctrl Pts',(0.475848034683176,-1.,1.95796111148177));
#22651=CARTESIAN_POINT('Ctrl Pts',(0.472397672264072,-1.,1.95296148278133));
#22652=CARTESIAN_POINT('Ctrl Pts',(0.468997482913135,-1.,1.94794381136514));
#22653=CARTESIAN_POINT('Ctrl Pts',(0.46564546202603,-1.,1.9428979419619));
#22654=CARTESIAN_POINT('Ctrl Pts',(0.462340031009056,-1.,1.93781486640821));
#22655=CARTESIAN_POINT('Ctrl Pts',(0.459081234547926,-1.,1.93269066517934));
#22656=CARTESIAN_POINT('Ctrl Pts',(0.45587200517437,-1.,1.92753067150476));
#22657=CARTESIAN_POINT('Ctrl Pts',(0.452719478359432,-1.,1.92235380648502));
#22658=CARTESIAN_POINT('Ctrl Pts',(0.449632260106662,-1.,1.91718342555755));
#22659=CARTESIAN_POINT('Ctrl Pts',(0.446617343485711,-1.,1.9120369998112));
#22660=CARTESIAN_POINT('Ctrl Pts',(0.44367755684915,-1.,1.90691756144898));
#22661=CARTESIAN_POINT('Ctrl Pts',(0.440807833704038,-1.,1.90180124389086));
#22662=CARTESIAN_POINT('Ctrl Pts',(0.437995003948244,-1.,1.89663648956466));
#22663=CARTESIAN_POINT('Ctrl Pts',(0.435225660963383,-1.,1.89136993975504));
#22664=CARTESIAN_POINT('Ctrl Pts',(0.432493038548748,-1.,1.88596913666793));
#22665=CARTESIAN_POINT('Ctrl Pts',(0.429803062482344,-1.,1.88044229001832));
#22666=CARTESIAN_POINT('Ctrl Pts',(0.427183828519102,-1.,1.87486989291484));
#22667=CARTESIAN_POINT('Ctrl Pts',(0.424678177291358,-1.,1.86937803944323));
#22668=CARTESIAN_POINT('Ctrl Pts',(0.422327307418275,-1.,1.86408083334028));
#22669=CARTESIAN_POINT('Ctrl Pts',(0.420157287975619,-1.,1.85903281096686));
#22670=CARTESIAN_POINT('Ctrl Pts',(0.418164129143534,-1.,1.85417632856234));
#22671=CARTESIAN_POINT('Ctrl Pts',(0.416300022038864,-1.,1.84929312929882));
#22672=CARTESIAN_POINT('Ctrl Pts',(0.41448743825434,-1.,1.8440575707371));
#22673=CARTESIAN_POINT('Ctrl Pts',(0.412633125322161,-1.,1.83808953475839));
#22674=CARTESIAN_POINT('Ctrl Pts',(0.410641256301674,-1.,1.83100408895216));
#22675=CARTESIAN_POINT('Ctrl Pts',(0.408428948108533,-1.,1.8224702267854));
#22676=CARTESIAN_POINT('Ctrl Pts',(0.405933518411838,-1.,1.81223801813988));
#22677=CARTESIAN_POINT('Ctrl Pts',(0.403107976170441,-1.,1.80012077176221));
#22678=CARTESIAN_POINT('Ctrl Pts',(0.39991940378308,-1.,1.78598826347533));
#22679=CARTESIAN_POINT('Ctrl Pts',(0.39634619612042,-1.,1.7697556004756));
#22680=CARTESIAN_POINT('Ctrl Pts',(0.392375812294307,-1.,1.75137405313962));
#22681=CARTESIAN_POINT('Ctrl Pts',(0.388877023509191,-1.,1.7349317097561));
#22682=CARTESIAN_POINT('Ctrl Pts',(0.38607079032701,-1.,1.72162022246158));
#22683=CARTESIAN_POINT('Ctrl Pts',(0.384119047315541,-1.,1.71231062891958));
#22684=CARTESIAN_POINT('Ctrl Pts',(0.383122945602004,-1.,1.7075470150345));
#22685=CARTESIAN_POINT('',(0.163289472382896,-1.,1.74236521665491));
#22686=CARTESIAN_POINT('Origin',(0.,-1.,0.));
#22687=CARTESIAN_POINT('',(0.0694764450219578,-1.,2.19890268624765));
#22688=CARTESIAN_POINT('Ctrl Pts',(0.163289472382896,-1.,1.74236521665491));
#22689=CARTESIAN_POINT('Ctrl Pts',(0.163814161002002,-1.,1.7472034950333));
#22690=CARTESIAN_POINT('Ctrl Pts',(0.164834765707158,-1.,1.75666056638427));
#22691=CARTESIAN_POINT('Ctrl Pts',(0.1662793551464,-1.,1.77018771684844));
#22692=CARTESIAN_POINT('Ctrl Pts',(0.168032772805197,-1.,1.7869064998507));
#22693=CARTESIAN_POINT('Ctrl Pts',(0.169936923904608,-1.,1.80561530629706));
#22694=CARTESIAN_POINT('Ctrl Pts',(0.171554770204119,-1.,1.82215766811545));
#22695=CARTESIAN_POINT('Ctrl Pts',(0.1728894428919,-1.,1.83658380527692));
#22696=CARTESIAN_POINT('Ctrl Pts',(0.173946627587731,-1.,1.8489811319852));
#22697=CARTESIAN_POINT('Ctrl Pts',(0.17473525927603,-1.,1.85948367088837));
#22698=CARTESIAN_POINT('Ctrl Pts',(0.175268337590757,-1.,1.86828349694799));
#22699=CARTESIAN_POINT('Ctrl Pts',(0.175563480746485,-1.,1.87563767773588));
#22700=CARTESIAN_POINT('Ctrl Pts',(0.175644148889698,-1.,1.88188663145367));
#22701=CARTESIAN_POINT('Ctrl Pts',(0.175538155840648,-1.,1.88742606273259));
#22702=CARTESIAN_POINT('Ctrl Pts',(0.175274276190844,-1.,1.892646301985));
#22703=CARTESIAN_POINT('Ctrl Pts',(0.174879405091263,-1.,1.89788101117132));
#22704=CARTESIAN_POINT('Ctrl Pts',(0.174375518661085,-1.,1.90335253862834));
#22705=CARTESIAN_POINT('Ctrl Pts',(0.173776635257816,-1.,1.90911693975267));
#22706=CARTESIAN_POINT('Ctrl Pts',(0.173090695383496,-1.,1.91511429159527));
#22707=CARTESIAN_POINT('Ctrl Pts',(0.172321621259513,-1.,1.9212233439798));
#22708=CARTESIAN_POINT('Ctrl Pts',(0.171471191532988,-1.,1.92731093582036));
#22709=CARTESIAN_POINT('Ctrl Pts',(0.170541253116201,-1.,1.93329183155539));
#22710=CARTESIAN_POINT('Ctrl Pts',(0.16953490481749,-1.,1.93915639211581));
#22711=CARTESIAN_POINT('Ctrl Pts',(0.168455741607556,-1.,1.94493757756931));
#22712=CARTESIAN_POINT('Ctrl Pts',(0.167307501784475,-1.,1.95069027794294));
#22713=CARTESIAN_POINT('Ctrl Pts',(0.166093592002812,-1.,1.9564675971873));
#22714=CARTESIAN_POINT('Ctrl Pts',(0.164816568920269,-1.,1.96229379940136));
#22715=CARTESIAN_POINT('Ctrl Pts',(0.163478185457734,-1.,1.96816512677967));
#22716=CARTESIAN_POINT('Ctrl Pts',(0.162079693556288,-1.,1.97406280235188));
#22717=CARTESIAN_POINT('Ctrl Pts',(0.160622060784611,-1.,1.97996195437559));
#22718=CARTESIAN_POINT('Ctrl Pts',(0.159106226437299,-1.,1.98584238283292));
#22719=CARTESIAN_POINT('Ctrl Pts',(0.157533331459227,-1.,1.99169810931908));
#22720=CARTESIAN_POINT('Ctrl Pts',(0.155904629548783,-1.,1.99753284771497));
#22721=CARTESIAN_POINT('Ctrl Pts',(0.154221403049722,-1.,2.00335565310543));
#22722=CARTESIAN_POINT('Ctrl Pts',(0.152484883621449,-1.,2.00917680318424));
#22723=CARTESIAN_POINT('Ctrl Pts',(0.150696157673078,-1.,2.01500291940238));
#22724=CARTESIAN_POINT('Ctrl Pts',(0.148856124775337,-1.,2.02083464969894));
#22725=CARTESIAN_POINT('Ctrl Pts',(0.146965557332583,-1.,2.02666926182017));
#22726=CARTESIAN_POINT('Ctrl Pts',(0.145025140186057,-1.,2.03250223739942));
#22727=CARTESIAN_POINT('Ctrl Pts',(0.143035515058208,-1.,2.03832911025912));
#22728=CARTESIAN_POINT('Ctrl Pts',(0.140997332152546,-1.,2.04414757947916));
#22729=CARTESIAN_POINT('Ctrl Pts',(0.138911255368966,-1.,2.04995762001328));
#22730=CARTESIAN_POINT('Ctrl Pts',(0.136777941218043,-1.,2.05576044414264));
#22731=CARTESIAN_POINT('Ctrl Pts',(0.134598026192106,-1.,2.06155781517842));
#22732=CARTESIAN_POINT('Ctrl Pts',(0.13237211154771,-1.,2.06735123910326));
#22733=CARTESIAN_POINT('Ctrl Pts',(0.130100748328403,-1.,2.07314114713063));
#22734=CARTESIAN_POINT('Ctrl Pts',(0.12778444527612,-1.,2.07892715110987));
#22735=CARTESIAN_POINT('Ctrl Pts',(0.125423679412061,-1.,2.08470840653643));
#22736=CARTESIAN_POINT('Ctrl Pts',(0.123018905621083,-1.,2.09048392424825));
#22737=CARTESIAN_POINT('Ctrl Pts',(0.120570567965122,-1.,2.0962529286773));
#22738=CARTESIAN_POINT('Ctrl Pts',(0.118079107988355,-1.,2.102015121329));
#22739=CARTESIAN_POINT('Ctrl Pts',(0.115544957687926,-1.,2.10777050261309));
#22740=CARTESIAN_POINT('Ctrl Pts',(0.112968534419737,-1.,2.11351924490306));
#22741=CARTESIAN_POINT('Ctrl Pts',(0.110350236135025,-1.,2.11926155590865));
#22742=CARTESIAN_POINT('Ctrl Pts',(0.10769043523109,-1.,2.12499752307));
#22743=CARTESIAN_POINT('Ctrl Pts',(0.104989479152739,-1.,2.13072704887293));
#22744=CARTESIAN_POINT('Ctrl Pts',(0.1022477005561,-1.,2.13644992667165));
#22745=CARTESIAN_POINT('Ctrl Pts',(0.0994654261990913,-1.,2.14216588396025));
#22746=CARTESIAN_POINT('Ctrl Pts',(0.0966429852305456,-1.,2.14787463531795));
#22747=CARTESIAN_POINT('Ctrl Pts',(0.0937807218867641,-1.,2.1535759397817));
#22748=CARTESIAN_POINT('Ctrl Pts',(0.0908789888107263,-1.,2.15926961544516));
#22749=CARTESIAN_POINT('Ctrl Pts',(0.087938129138692,-1.,2.16495552645014));
#22750=CARTESIAN_POINT('Ctrl Pts',(0.084958462083537,-1.,2.17063357870952));
#22751=CARTESIAN_POINT('Ctrl Pts',(0.0819402680872763,-1.,2.176303712113));
#22752=CARTESIAN_POINT('Ctrl Pts',(0.078883772768524,-1.,2.18196589448887));
#22753=CARTESIAN_POINT('Ctrl Pts',(0.0757891465836145,-1.,2.1876201139953));
#22754=CARTESIAN_POINT('Ctrl Pts',(0.0732830357306722,-1.,2.19213712013662));
#22755=CARTESIAN_POINT('Ctrl Pts',(0.0713863779526151,-1.,2.19552129484002));
#22756=CARTESIAN_POINT('Ctrl Pts',(0.0701143536325487,-1.,2.19777582085423));
#22757=CARTESIAN_POINT('Ctrl Pts',(0.0694764450219578,-1.,2.19890268624765));
#22758=CARTESIAN_POINT('',(-0.0694764450219586,-1.,2.19890268624765));
#22759=CARTESIAN_POINT('',(0.0694764450219578,-1.,2.19890268624765));
#22760=CARTESIAN_POINT('',(-0.163289472382896,-1.,1.74236521665491));
#22761=CARTESIAN_POINT('Ctrl Pts',(-0.0694764450219586,-1.,2.19890268624765));
#22762=CARTESIAN_POINT('Ctrl Pts',(-0.0701143536324929,-1.,2.19777582085261));
#22763=CARTESIAN_POINT('Ctrl Pts',(-0.071386377952463,-1.,2.19552129483562));
#22764=CARTESIAN_POINT('Ctrl Pts',(-0.0732830357304279,-1.,2.19213712012956));
#22765=CARTESIAN_POINT('Ctrl Pts',(-0.0757891465833414,-1.,2.1876201139874));
#22766=CARTESIAN_POINT('Ctrl Pts',(-0.078883772768323,-1.,2.18196589448304));
#22767=CARTESIAN_POINT('Ctrl Pts',(-0.0819402680871942,-1.,2.1763037121106));
#22768=CARTESIAN_POINT('Ctrl Pts',(-0.0849584620835646,-1.,2.17063357871031));
#22769=CARTESIAN_POINT('Ctrl Pts',(-0.0879381291387825,-1.,2.16495552645275));
#22770=CARTESIAN_POINT('Ctrl Pts',(-0.0908789888108269,-1.,2.15926961544808));
#22771=CARTESIAN_POINT('Ctrl Pts',(-0.0937807218868348,-1.,2.15357593978377));
#22772=CARTESIAN_POINT('Ctrl Pts',(-0.0966429852305691,-1.,2.14787463531864));
#22773=CARTESIAN_POINT('Ctrl Pts',(-0.0994654261990745,-1.,2.14216588395974));
#22774=CARTESIAN_POINT('Ctrl Pts',(-0.102247700556064,-1.,2.13644992667052));
#22775=CARTESIAN_POINT('Ctrl Pts',(-0.104989479152703,-1.,2.1307270488718));
#22776=CARTESIAN_POINT('Ctrl Pts',(-0.107690435231068,-1.,2.12499752306927));
#22777=CARTESIAN_POINT('Ctrl Pts',(-0.11035023613502,-1.,2.11926155590849));
#22778=CARTESIAN_POINT('Ctrl Pts',(-0.112968534419746,-1.,2.11351924490335));
#22779=CARTESIAN_POINT('Ctrl Pts',(-0.115544957687941,-1.,2.10777050261359));
#22780=CARTESIAN_POINT('Ctrl Pts',(-0.118079107988368,-1.,2.10201512132945));
#22781=CARTESIAN_POINT('Ctrl Pts',(-0.120570567965129,-1.,2.09625292867756));
#22782=CARTESIAN_POINT('Ctrl Pts',(-0.123018905621083,-1.,2.09048392424826));
#22783=CARTESIAN_POINT('Ctrl Pts',(-0.125423679412058,-1.,2.08470840653628));
#22784=CARTESIAN_POINT('Ctrl Pts',(-0.127784445276116,-1.,2.07892715110967));
#22785=CARTESIAN_POINT('Ctrl Pts',(-0.130100748328401,-1.,2.07314114713047));
#22786=CARTESIAN_POINT('Ctrl Pts',(-0.13237211154771,-1.,2.06735123910319));
#22787=CARTESIAN_POINT('Ctrl Pts',(-0.134598026192107,-1.,2.06155781517844));
#22788=CARTESIAN_POINT('Ctrl Pts',(-0.136777941218044,-1.,2.0557604441427));
#22789=CARTESIAN_POINT('Ctrl Pts',(-0.138911255368966,-1.,2.04995762001333));
#22790=CARTESIAN_POINT('Ctrl Pts',(-0.140997332152546,-1.,2.04414757947919));
#22791=CARTESIAN_POINT('Ctrl Pts',(-0.143035515058208,-1.,2.03832911025913));
#22792=CARTESIAN_POINT('Ctrl Pts',(-0.145025140186058,-1.,2.03250223739941));
#22793=CARTESIAN_POINT('Ctrl Pts',(-0.146965557332586,-1.,2.02666926182017));
#22794=CARTESIAN_POINT('Ctrl Pts',(-0.148856124775343,-1.,2.02083464969897));
#22795=CARTESIAN_POINT('Ctrl Pts',(-0.150696157673084,-1.,2.01500291940243));
#22796=CARTESIAN_POINT('Ctrl Pts',(-0.152484883621452,-1.,2.00917680318426));
#22797=CARTESIAN_POINT('Ctrl Pts',(-0.154221403049719,-1.,2.00335565310539));
#22798=CARTESIAN_POINT('Ctrl Pts',(-0.155904629548775,-1.,1.99753284771487));
#22799=CARTESIAN_POINT('Ctrl Pts',(-0.157533331459215,-1.,1.99169810931893));
#22800=CARTESIAN_POINT('Ctrl Pts',(-0.159106226437289,-1.,1.98584238283279));
#22801=CARTESIAN_POINT('Ctrl Pts',(-0.16062206078461,-1.,1.97996195437557));
#22802=CARTESIAN_POINT('Ctrl Pts',(-0.162079693556302,-1.,1.97406280235204));
#22803=CARTESIAN_POINT('Ctrl Pts',(-0.16347818545776,-1.,1.96816512678));
#22804=CARTESIAN_POINT('Ctrl Pts',(-0.1648165689203,-1.,1.96229379940174));
#22805=CARTESIAN_POINT('Ctrl Pts',(-0.166093592002833,-1.,1.95646759718755));
#22806=CARTESIAN_POINT('Ctrl Pts',(-0.167307501784469,-1.,1.95069027794286));
#22807=CARTESIAN_POINT('Ctrl Pts',(-0.168455741607516,-1.,1.94493757756879));
#22808=CARTESIAN_POINT('Ctrl Pts',(-0.169534904817425,-1.,1.93915639211497));
#22809=CARTESIAN_POINT('Ctrl Pts',(-0.170541253116136,-1.,1.93329183155455));
#22810=CARTESIAN_POINT('Ctrl Pts',(-0.17147119153296,-1.,1.92731093582));
#22811=CARTESIAN_POINT('Ctrl Pts',(-0.172321621259557,-1.,1.92122334398034));
#22812=CARTESIAN_POINT('Ctrl Pts',(-0.173090695383619,-1.,1.91511429159681));
#22813=CARTESIAN_POINT('Ctrl Pts',(-0.173776635257984,-1.,1.90911693975475));
#22814=CARTESIAN_POINT('Ctrl Pts',(-0.174375518661222,-1.,1.90335253863003));
#22815=CARTESIAN_POINT('Ctrl Pts',(-0.174879405091277,-1.,1.89788101117148));
#22816=CARTESIAN_POINT('Ctrl Pts',(-0.175274276190664,-1.,1.89264630198279));
#22817=CARTESIAN_POINT('Ctrl Pts',(-0.175538155840286,-1.,1.88742606272818));
#22818=CARTESIAN_POINT('Ctrl Pts',(-0.175644148889271,-1.,1.88188663144846));
#22819=CARTESIAN_POINT('Ctrl Pts',(-0.175563480746206,-1.,1.87563767773249));
#22820=CARTESIAN_POINT('Ctrl Pts',(-0.175268337590901,-1.,1.86828349694972));
#22821=CARTESIAN_POINT('Ctrl Pts',(-0.174735259276856,-1.,1.85948367089838));
#22822=CARTESIAN_POINT('Ctrl Pts',(-0.173946627589401,-1.,1.84898113200543));
#22823=CARTESIAN_POINT('Ctrl Pts',(-0.17288944289442,-1.,1.83658380530747));
#22824=CARTESIAN_POINT('Ctrl Pts',(-0.171554770207306,-1.,1.82215766815414));
#22825=CARTESIAN_POINT('Ctrl Pts',(-0.169936923908078,-1.,1.80561530633924));
#22826=CARTESIAN_POINT('Ctrl Pts',(-0.16803277280837,-1.,1.78690649988931));
#22827=CARTESIAN_POINT('Ctrl Pts',(-0.166279355148738,-1.,1.77018771687692));
#22828=CARTESIAN_POINT('Ctrl Pts',(-0.164834765708484,-1.,1.75666056640041));
#22829=CARTESIAN_POINT('Ctrl Pts',(-0.163814161002474,-1.,1.74720349503904));
#22830=CARTESIAN_POINT('Ctrl Pts',(-0.163289472382896,-1.,1.74236521665491));
#22831=CARTESIAN_POINT('',(-0.383122945602004,-1.,1.7075470150345));
#22832=CARTESIAN_POINT('Origin',(0.,-1.,0.));
#22833=CARTESIAN_POINT('',(-0.61342227326009,-1.,2.11275013067528));
#22834=CARTESIAN_POINT('Ctrl Pts',(-0.383122945602004,-1.,1.7075470150345));
#22835=CARTESIAN_POINT('Ctrl Pts',(-0.384119047314215,-1.,1.71231062891398));
#22836=CARTESIAN_POINT('Ctrl Pts',(-0.386070790323281,-1.,1.72162022244582));
#22837=CARTESIAN_POINT('Ctrl Pts',(-0.388877023502615,-1.,1.73493170972829));
#22838=CARTESIAN_POINT('Ctrl Pts',(-0.392375812285395,-1.,1.75137405310193));
#22839=CARTESIAN_POINT('Ctrl Pts',(-0.396346196110688,-1.,1.76975560043442));
#22840=CARTESIAN_POINT('Ctrl Pts',(-0.399919403774155,-1.,1.78598826343754));
#22841=CARTESIAN_POINT('Ctrl Pts',(-0.403107976163396,-1.,1.80012077173238));
#22842=CARTESIAN_POINT('Ctrl Pts',(-0.405933518407175,-1.,1.81223801812013));
#22843=CARTESIAN_POINT('Ctrl Pts',(-0.408428948106227,-1.,1.82247022677562));
#22844=CARTESIAN_POINT('Ctrl Pts',(-0.410641256301276,-1.,1.83100408895047));
#22845=CARTESIAN_POINT('Ctrl Pts',(-0.412633125322945,-1.,1.8380895347617));
#22846=CARTESIAN_POINT('Ctrl Pts',(-0.414487438255542,-1.,1.84405757074218));
#22847=CARTESIAN_POINT('Ctrl Pts',(-0.416300022039885,-1.,1.84929312930314));
#22848=CARTESIAN_POINT('Ctrl Pts',(-0.418164129144045,-1.,1.8541763285645));
#22849=CARTESIAN_POINT('Ctrl Pts',(-0.420157287975583,-1.,1.8590328109667));
#22850=CARTESIAN_POINT('Ctrl Pts',(-0.422327307417885,-1.,1.86408083333863));
#22851=CARTESIAN_POINT('Ctrl Pts',(-0.424678177290876,-1.,1.8693780394412));
#22852=CARTESIAN_POINT('Ctrl Pts',(-0.427183828518743,-1.,1.87486989291333));
#22853=CARTESIAN_POINT('Ctrl Pts',(-0.429803062482217,-1.,1.88044229001778));
#22854=CARTESIAN_POINT('Ctrl Pts',(-0.432493038548833,-1.,1.88596913666828));
#22855=CARTESIAN_POINT('Ctrl Pts',(-0.43522566096358,-1.,1.89136993975585));
#22856=CARTESIAN_POINT('Ctrl Pts',(-0.437995003948443,-1.,1.89663648956549));
#22857=CARTESIAN_POINT('Ctrl Pts',(-0.440807833704161,-1.,1.90180124389137));
#22858=CARTESIAN_POINT('Ctrl Pts',(-0.44367755684917,-1.,1.90691756144906));
#22859=CARTESIAN_POINT('Ctrl Pts',(-0.446617343485651,-1.,1.91203699981095));
#22860=CARTESIAN_POINT('Ctrl Pts',(-0.449632260106572,-1.,1.91718342555717));
#22861=CARTESIAN_POINT('Ctrl Pts',(-0.452719478359356,-1.,1.9223538064847));
#22862=CARTESIAN_POINT('Ctrl Pts',(-0.455872005174335,-1.,1.92753067150461));
#22863=CARTESIAN_POINT('Ctrl Pts',(-0.459081234547931,-1.,1.93269066517936));
#22864=CARTESIAN_POINT('Ctrl Pts',(-0.462340031009087,-1.,1.93781486640834));
#22865=CARTESIAN_POINT('Ctrl Pts',(-0.465645462026065,-1.,1.94289794196205));
#22866=CARTESIAN_POINT('Ctrl Pts',(-0.468997482913158,-1.,1.94794381136524));
#22867=CARTESIAN_POINT('Ctrl Pts',(-0.47239767226408,-1.,1.95296148278136));
#22868=CARTESIAN_POINT('Ctrl Pts',(-0.475848034683172,-1.,1.95796111148175));
#22869=CARTESIAN_POINT('Ctrl Pts',(-0.479349583074846,-1.,1.96294933055938));
#22870=CARTESIAN_POINT('Ctrl Pts',(-0.482901662120687,-1.,1.96792703422358));
#22871=CARTESIAN_POINT('Ctrl Pts',(-0.486502692907661,-1.,1.97289186263272));
#22872=CARTESIAN_POINT('Ctrl Pts',(-0.490150627860955,-1.,1.97783973019229));
#22873=CARTESIAN_POINT('Ctrl Pts',(-0.493843476541492,-1.,1.9827665876182));
#22874=CARTESIAN_POINT('Ctrl Pts',(-0.497579909545564,-1.,1.98767044752929));
#22875=CARTESIAN_POINT('Ctrl Pts',(-0.501359287727129,-1.,1.9925514912615));
#22876=CARTESIAN_POINT('Ctrl Pts',(-0.505181361323011,-1.,1.99741107463567));
#22877=CARTESIAN_POINT('Ctrl Pts',(-0.509046069886152,-1.,2.00225107134733));
#22878=CARTESIAN_POINT('Ctrl Pts',(-0.512953306961814,-1.,2.00707309946955));
#22879=CARTESIAN_POINT('Ctrl Pts',(-0.516902681728733,-1.,2.01187773939257));
#22880=CARTESIAN_POINT('Ctrl Pts',(-0.520893590399428,-1.,2.01666477917305));
#22881=CARTESIAN_POINT('Ctrl Pts',(-0.524925318333518,-1.,2.02143356304712));
#22882=CARTESIAN_POINT('Ctrl Pts',(-0.528997127241911,-1.,2.02618329083289));
#22883=CARTESIAN_POINT('Ctrl Pts',(-0.533108355132905,-1.,2.03091336214401));
#22884=CARTESIAN_POINT('Ctrl Pts',(-0.537258489833134,-1.,2.03562362953993));
#22885=CARTESIAN_POINT('Ctrl Pts',(-0.54144712061552,-1.,2.0403142269048));
#22886=CARTESIAN_POINT('Ctrl Pts',(-0.545673903817348,-1.,2.0449854471456));
#22887=CARTESIAN_POINT('Ctrl Pts',(-0.549938525150342,-1.,2.04963761077974));
#22888=CARTESIAN_POINT('Ctrl Pts',(-0.55424065746411,-1.,2.05427091604482));
#22889=CARTESIAN_POINT('Ctrl Pts',(-0.558579940185467,-1.,2.05888537756571));
#22890=CARTESIAN_POINT('Ctrl Pts',(-0.562955993082574,-1.,2.06348090160697));
#22891=CARTESIAN_POINT('Ctrl Pts',(-0.567368421181229,-1.,2.06805732997383));
#22892=CARTESIAN_POINT('Ctrl Pts',(-0.571816823242411,-1.,2.07261449292757));
#22893=CARTESIAN_POINT('Ctrl Pts',(-0.576300797416275,-1.,2.07715226767361));
#22894=CARTESIAN_POINT('Ctrl Pts',(-0.580819952107257,-1.,2.08167059018138));
#22895=CARTESIAN_POINT('Ctrl Pts',(-0.585373918990895,-1.,2.086169437277));
#22896=CARTESIAN_POINT('Ctrl Pts',(-0.589962365403189,-1.,2.09064881812053));
#22897=CARTESIAN_POINT('Ctrl Pts',(-0.594585006052824,-1.,2.09510876220501));
#22898=CARTESIAN_POINT('Ctrl Pts',(-0.599241616422144,-1.,2.09954930865331));
#22899=CARTESIAN_POINT('Ctrl Pts',(-0.603932030738212,-1.,2.10397049887709));
#22900=CARTESIAN_POINT('Ctrl Pts',(-0.607711315456826,-1.,2.10749199615859));
#22901=CARTESIAN_POINT('Ctrl Pts',(-0.610560911691113,-1.,2.11012443807661));
#22902=CARTESIAN_POINT('Ctrl Pts',(-0.61246736556225,-1.,2.11187554260142));
#22903=CARTESIAN_POINT('Ctrl Pts',(-0.61342227326009,-1.,2.11275013067528));
#22904=CARTESIAN_POINT('',(-0.745574324794401,-1.,2.0698113262342));
#22905=CARTESIAN_POINT('',(-0.61342227326009,-1.,2.11275013067528));
#22906=CARTESIAN_POINT('',(-0.693717979106306,-1.,1.60662857109684));
#22907=CARTESIAN_POINT('Ctrl Pts',(-0.745574324794401,-1.,2.0698113262342));
#22908=CARTESIAN_POINT('Ctrl Pts',(-0.74583279137781,-1.,2.06854248895575));
#22909=CARTESIAN_POINT('Ctrl Pts',(-0.746345871542696,-1.,2.06600523016401));
#22910=CARTESIAN_POINT('Ctrl Pts',(-0.747103932785504,-1.,2.06220058927162));
#22911=CARTESIAN_POINT('Ctrl Pts',(-0.748091554181101,-1.,2.05713023030263));
#22912=CARTESIAN_POINT('Ctrl Pts',(-0.749287468663053,-1.,2.05079645591606));
#22913=CARTESIAN_POINT('Ctrl Pts',(-0.750444657874758,-1.,2.04446689147754));
#22914=CARTESIAN_POINT('Ctrl Pts',(-0.751562963361384,-1.,2.03814160092173));
#22915=CARTESIAN_POINT('Ctrl Pts',(-0.752642180488104,-1.,2.03182068456467));
#22916=CARTESIAN_POINT('Ctrl Pts',(-0.753682061113766,-1.,2.02550428623587));
#22917=CARTESIAN_POINT('Ctrl Pts',(-0.75468233072352,-1.,2.01919259406003));
#22918=CARTESIAN_POINT('Ctrl Pts',(-0.7556427049581,-1.,2.01288584328149));
#22919=CARTESIAN_POINT('Ctrl Pts',(-0.756562904646496,-1.,2.00658431587682));
#22920=CARTESIAN_POINT('Ctrl Pts',(-0.757442676862341,-1.,2.00028834739072));
#22921=CARTESIAN_POINT('Ctrl Pts',(-0.758281796766377,-1.,1.9939983109871));
#22922=CARTESIAN_POINT('Ctrl Pts',(-0.759080037802243,-1.,1.98771456680806));
#22923=CARTESIAN_POINT('Ctrl Pts',(-0.759837147452135,-1.,1.98143741418156));
#22924=CARTESIAN_POINT('Ctrl Pts',(-0.760552825409855,-1.,1.97516705321521));
#22925=CARTESIAN_POINT('Ctrl Pts',(-0.761226690483986,-1.,1.96890351582545));
#22926=CARTESIAN_POINT('Ctrl Pts',(-0.761858300014575,-1.,1.96264672744229));
#22927=CARTESIAN_POINT('Ctrl Pts',(-0.762447203806263,-1.,1.95639665309893));
#22928=CARTESIAN_POINT('Ctrl Pts',(-0.762992990878774,-1.,1.95015342590025));
#22929=CARTESIAN_POINT('Ctrl Pts',(-0.76349533353858,-1.,1.94391746617626));
#22930=CARTESIAN_POINT('Ctrl Pts',(-0.763954049121393,-1.,1.93768964875867));
#22931=CARTESIAN_POINT('Ctrl Pts',(-0.764369010673889,-1.,1.93147105496367));
#22932=CARTESIAN_POINT('Ctrl Pts',(-0.764740025488189,-1.,1.92526263537041));
#22933=CARTESIAN_POINT('Ctrl Pts',(-0.765066729667095,-1.,1.91906491634197));
#22934=CARTESIAN_POINT('Ctrl Pts',(-0.765348465884739,-1.,1.91287765805174));
#22935=CARTESIAN_POINT('Ctrl Pts',(-0.765584196937936,-1.,1.90669961402362));
#22936=CARTESIAN_POINT('Ctrl Pts',(-0.765772772593395,-1.,1.90052930393599));
#22937=CARTESIAN_POINT('Ctrl Pts',(-0.765913193856979,-1.,1.89436577771389));
#22938=CARTESIAN_POINT('Ctrl Pts',(-0.76600483706209,-1.,1.88820926433409));
#22939=CARTESIAN_POINT('Ctrl Pts',(-0.766047794851869,-1.,1.88206215302561));
#22940=CARTESIAN_POINT('Ctrl Pts',(-0.766042837036759,-1.,1.87592888967886));
#22941=CARTESIAN_POINT('Ctrl Pts',(-0.765990708546111,-1.,1.86981398314345));
#22942=CARTESIAN_POINT('Ctrl Pts',(-0.765891519092557,-1.,1.86372027063314));
#22943=CARTESIAN_POINT('Ctrl Pts',(-0.765744212909305,-1.,1.85764741390391));
#22944=CARTESIAN_POINT('Ctrl Pts',(-0.765545710619023,-1.,1.85158945130054));
#22945=CARTESIAN_POINT('Ctrl Pts',(-0.765291664861971,-1.,1.8455369887591));
#22946=CARTESIAN_POINT('Ctrl Pts',(-0.764978057881687,-1.,1.83948181064823));
#22947=CARTESIAN_POINT('Ctrl Pts',(-0.764602549687845,-1.,1.8334207722714));
#22948=CARTESIAN_POINT('Ctrl Pts',(-0.764165902606055,-1.,1.8273599120008));
#22949=CARTESIAN_POINT('Ctrl Pts',(-0.763673465462854,-1.,1.82131873145297));
#22950=CARTESIAN_POINT('Ctrl Pts',(-0.763132003836783,-1.,1.81532118405566));
#22951=CARTESIAN_POINT('Ctrl Pts',(-0.762546129464036,-1.,1.80938551463989));
#22952=CARTESIAN_POINT('Ctrl Pts',(-0.761915336443516,-1.,1.80351583877334));
#22953=CARTESIAN_POINT('Ctrl Pts',(-0.761229695230359,-1.,1.79768986997735));
#22954=CARTESIAN_POINT('Ctrl Pts',(-0.760469555880425,-1.,1.79185815610802));
#22955=CARTESIAN_POINT('Ctrl Pts',(-0.759614401109868,-1.,1.78596964884526));
#22956=CARTESIAN_POINT('Ctrl Pts',(-0.75865062667738,-1.,1.77999411220912));
#22957=CARTESIAN_POINT('Ctrl Pts',(-0.757578264077238,-1.,1.77394167108342));
#22958=CARTESIAN_POINT('Ctrl Pts',(-0.756421896028403,-1.,1.76789396003141));
#22959=CARTESIAN_POINT('Ctrl Pts',(-0.755220979975262,-1.,1.7619781724032));
#22960=CARTESIAN_POINT('Ctrl Pts',(-0.75400925402848,-1.,1.75631083600175));
#22961=CARTESIAN_POINT('Ctrl Pts',(-0.752797683531377,-1.,1.75095139468809));
#22962=CARTESIAN_POINT('Ctrl Pts',(-0.751555614163629,-1.,1.74585086852298));
#22963=CARTESIAN_POINT('Ctrl Pts',(-0.75019343597954,-1.,1.74080458266705));
#22964=CARTESIAN_POINT('Ctrl Pts',(-0.748582462954855,-1.,1.73550351679848));
#22965=CARTESIAN_POINT('Ctrl Pts',(-0.746574710096436,-1.,1.72958533647399));
#22966=CARTESIAN_POINT('Ctrl Pts',(-0.744021445433764,-1.,1.7226822991693));
#22967=CARTESIAN_POINT('Ctrl Pts',(-0.740795162032088,-1.,1.71447789751927));
#22968=CARTESIAN_POINT('Ctrl Pts',(-0.736799665724771,-1.,1.70473309006121));
#22969=CARTESIAN_POINT('Ctrl Pts',(-0.731963238697195,-1.,1.69326921975743));
#22970=CARTESIAN_POINT('Ctrl Pts',(-0.726235967997433,-1.,1.67996158455503));
#22971=CARTESIAN_POINT('Ctrl Pts',(-0.719585433804282,-1.,1.6647288055568));
#22972=CARTESIAN_POINT('Ctrl Pts',(-0.711993139355394,-1.,1.64752408832016));
#22973=CARTESIAN_POINT('Ctrl Pts',(-0.705159151988319,-1.,1.63216541664676));
#22974=CARTESIAN_POINT('Ctrl Pts',(-0.699605146405088,-1.,1.61974673472612));
#22975=CARTESIAN_POINT('Ctrl Pts',(-0.695712097881194,-1.,1.61106790958151));
#22976=CARTESIAN_POINT('Ctrl Pts',(-0.693717979106306,-1.,1.60662857109684));
#22977=CARTESIAN_POINT('',(-0.892032620296855,-1.,1.5055822144029));
#22978=CARTESIAN_POINT('Origin',(0.,-1.,0.));
#22979=CARTESIAN_POINT('',(-1.23627494547115,-1.,1.81978687191668));
#22980=CARTESIAN_POINT('Ctrl Pts',(-0.892032620296855,-1.,1.5055822144029));
#22981=CARTESIAN_POINT('Ctrl Pts',(-0.894452006964543,-1.,1.50980486806688));
#22982=CARTESIAN_POINT('Ctrl Pts',(-0.899185047483511,-1.,1.51805569590094));
#22983=CARTESIAN_POINT('Ctrl Pts',(-0.905967409625651,-1.,1.52984849887993));
#22984=CARTESIAN_POINT('Ctrl Pts',(-0.914375919026456,-1.,1.54440491149498));
#22985=CARTESIAN_POINT('Ctrl Pts',(-0.923832188944341,-1.,1.56065988578893));
#22986=CARTESIAN_POINT('Ctrl Pts',(-0.932246680108685,-1.,1.57499388382243));
#22987=CARTESIAN_POINT('Ctrl Pts',(-0.939646377893399,-1.,1.58744937487176));
#22988=CARTESIAN_POINT('Ctrl Pts',(-0.946078063315257,-1.,1.59810042043673));
#22989=CARTESIAN_POINT('Ctrl Pts',(-0.951613284356035,-1.,1.60706069896936));
#22990=CARTESIAN_POINT('Ctrl Pts',(-0.956354422920671,-1.,1.61449324337085));
#22991=CARTESIAN_POINT('Ctrl Pts',(-0.960438326101729,-1.,1.62061638140221));
#22992=CARTESIAN_POINT('Ctrl Pts',(-0.964046107040536,-1.,1.62571930670187));
#22993=CARTESIAN_POINT('Ctrl Pts',(-0.967387853230345,-1.,1.63013849959461));
#22994=CARTESIAN_POINT('Ctrl Pts',(-0.970669715997509,-1.,1.63420665729798));
#22995=CARTESIAN_POINT('Ctrl Pts',(-0.974066058287418,-1.,1.63820952658144));
#22996=CARTESIAN_POINT('Ctrl Pts',(-0.977689794119416,-1.,1.64233990826687));
#22997=CARTESIAN_POINT('Ctrl Pts',(-0.981562530939489,-1.,1.64665139190656));
#22998=CARTESIAN_POINT('Ctrl Pts',(-0.985642622920821,-1.,1.65110016612638));
#22999=CARTESIAN_POINT('Ctrl Pts',(-0.989855627854165,-1.,1.65559044289699));
#23000=CARTESIAN_POINT('Ctrl Pts',(-0.994121836661306,-1.,1.66001553809947));
#23001=CARTESIAN_POINT('Ctrl Pts',(-0.998389654952758,-1.,1.66430758030376));
#23002=CARTESIAN_POINT('Ctrl Pts',(-1.00265091003727,-1.,1.66846059277303));
#23003=CARTESIAN_POINT('Ctrl Pts',(-1.00692206696414,-1.,1.67250335383293));
#23004=CARTESIAN_POINT('Ctrl Pts',(-1.01123236493511,-1.,1.67648246776464));
#23005=CARTESIAN_POINT('Ctrl Pts',(-1.01561026162773,-1.,1.68044289894798));
#23006=CARTESIAN_POINT('Ctrl Pts',(-1.02006795074201,-1.,1.68440578021706));
#23007=CARTESIAN_POINT('Ctrl Pts',(-1.02460180535255,-1.,1.68836910178447));
#23008=CARTESIAN_POINT('Ctrl Pts',(-1.02919977579147,-1.,1.69231840863458));
#23009=CARTESIAN_POINT('Ctrl Pts',(-1.03384646003588,-1.,1.69623414782771));
#23010=CARTESIAN_POINT('Ctrl Pts',(-1.03852922490789,-1.,1.70010052930962));
#23011=CARTESIAN_POINT('Ctrl Pts',(-1.04324363334554,-1.,1.70391338707982));
#23012=CARTESIAN_POINT('Ctrl Pts',(-1.04799085404995,-1.,1.70767646263649));
#23013=CARTESIAN_POINT('Ctrl Pts',(-1.05277517202855,-1.,1.71139783543989));
#23014=CARTESIAN_POINT('Ctrl Pts',(-1.05760163192479,-1.,1.7150865442702));
#23015=CARTESIAN_POINT('Ctrl Pts',(-1.06247324680647,-1.,1.71874858456904));
#23016=CARTESIAN_POINT('Ctrl Pts',(-1.06738966975462,-1.,1.72238500928453));
#23017=CARTESIAN_POINT('Ctrl Pts',(-1.07234866990252,-1.,1.72599406198488));
#23018=CARTESIAN_POINT('Ctrl Pts',(-1.0773470373727,-1.,1.72957248977424));
#23019=CARTESIAN_POINT('Ctrl Pts',(-1.08238162784749,-1.,1.73311705663407));
#23020=CARTESIAN_POINT('Ctrl Pts',(-1.08745056285427,-1.,1.73662628326091));
#23021=CARTESIAN_POINT('Ctrl Pts',(-1.09255329056493,-1.,1.74010053962247));
#23022=CARTESIAN_POINT('Ctrl Pts',(-1.09768999241225,-1.,1.74354119236208));
#23023=CARTESIAN_POINT('Ctrl Pts',(-1.10286118991143,-1.,1.74695004214923));
#23024=CARTESIAN_POINT('Ctrl Pts',(-1.10806728183007,-1.,1.7503286607592));
#23025=CARTESIAN_POINT('Ctrl Pts',(-1.11330807582551,-1.,1.7536777209463));
#23026=CARTESIAN_POINT('Ctrl Pts',(-1.11858293216763,-1.,1.75699720772105));
#23027=CARTESIAN_POINT('Ctrl Pts',(-1.12389096855086,-1.,1.76028671825096));
#23028=CARTESIAN_POINT('Ctrl Pts',(-1.12923123555075,-1.,1.7635457196617));
#23029=CARTESIAN_POINT('Ctrl Pts',(-1.1346029180462,-1.,1.76677384551862));
#23030=CARTESIAN_POINT('Ctrl Pts',(-1.14000548336975,-1.,1.76997111386769));
#23031=CARTESIAN_POINT('Ctrl Pts',(-1.1454385822692,-1.,1.77313777896194));
#23032=CARTESIAN_POINT('Ctrl Pts',(-1.15090197841515,-1.,1.7762742255701));
#23033=CARTESIAN_POINT('Ctrl Pts',(-1.15639547194698,-1.,1.77938085564275));
#23034=CARTESIAN_POINT('Ctrl Pts',(-1.16191881298499,-1.,1.78245795881009));
#23035=CARTESIAN_POINT('Ctrl Pts',(-1.16747166312303,-1.,1.78550566040443));
#23036=CARTESIAN_POINT('Ctrl Pts',(-1.17305363177328,-1.,1.78852398877616));
#23037=CARTESIAN_POINT('Ctrl Pts',(-1.17866429440809,-1.,1.79151291552689));
#23038=CARTESIAN_POINT('Ctrl Pts',(-1.18430321697432,-1.,1.79447240321515));
#23039=CARTESIAN_POINT('Ctrl Pts',(-1.18996997934445,-1.,1.79740245923478));
#23040=CARTESIAN_POINT('Ctrl Pts',(-1.19566418930242,-1.,1.80030314369879));
#23041=CARTESIAN_POINT('Ctrl Pts',(-1.20138548938974,-1.,1.80317454838603));
#23042=CARTESIAN_POINT('Ctrl Pts',(-1.20713356605475,-1.,1.80601678480707));
#23043=CARTESIAN_POINT('Ctrl Pts',(-1.21290815708314,-1.,1.80882996917129));
#23044=CARTESIAN_POINT('Ctrl Pts',(-1.21870906103557,-1.,1.81161420806656));
#23045=CARTESIAN_POINT('Ctrl Pts',(-1.2245361330495,-1.,1.81436959210434));
#23046=CARTESIAN_POINT('Ctrl Pts',(-1.2292186489137,-1.,1.8165508718364));
#23047=CARTESIAN_POINT('Ctrl Pts',(-1.2327422452705,-1.,1.81817389921279));
#23048=CARTESIAN_POINT('Ctrl Pts',(-1.23509651170476,-1.,1.81925017193666));
#23049=CARTESIAN_POINT('Ctrl Pts',(-1.23627494547115,-1.,1.81978687191668));
#23050=CARTESIAN_POINT('',(-1.34869019493419,-1.,1.73811241238545));
#23051=CARTESIAN_POINT('',(-1.23627494547115,-1.,1.81978687191668));
#23052=CARTESIAN_POINT('',(-1.15624053661742,-1.,1.31362392696032));
#23053=CARTESIAN_POINT('Ctrl Pts',(-1.34869019493419,-1.,1.73811241238545));
#23054=CARTESIAN_POINT('Ctrl Pts',(-1.34854391898045,-1.,1.73682580585691));
#23055=CARTESIAN_POINT('Ctrl Pts',(-1.34824783112887,-1.,1.73425417885907));
#23056=CARTESIAN_POINT('Ctrl Pts',(-1.34779309152035,-1.,1.7304014965394));
#23057=CARTESIAN_POINT('Ctrl Pts',(-1.34716554819527,-1.,1.72527410680674));
#23058=CARTESIAN_POINT('Ctrl Pts',(-1.34634568653227,-1.,1.7188807715049));
#23059=CARTESIAN_POINT('Ctrl Pts',(-1.34549029589416,-1.,1.71250340686822));
#23060=CARTESIAN_POINT('Ctrl Pts',(-1.34459924533831,-1.,1.70614212266738));
#23061=CARTESIAN_POINT('Ctrl Pts',(-1.34367237124483,-1.,1.69979707754427));
#23062=CARTESIAN_POINT('Ctrl Pts',(-1.34270948206319,-1.,1.6934684849687));
#23063=CARTESIAN_POINT('Ctrl Pts',(-1.341710374848,-1.,1.68715660868764));
#23064=CARTESIAN_POINT('Ctrl Pts',(-1.34067485185203,-1.,1.68086176030362));
#23065=CARTESIAN_POINT('Ctrl Pts',(-1.3396027347034,-1.,1.67458429426086));
#23066=CARTESIAN_POINT('Ctrl Pts',(-1.33849388654388,-1.,1.66832460783989));
#23067=CARTESIAN_POINT('Ctrl Pts',(-1.33734820885262,-1.,1.66208312541983));
#23068=CARTESIAN_POINT('Ctrl Pts',(-1.33616559745172,-1.,1.65586025952593));
#23069=CARTESIAN_POINT('Ctrl Pts',(-1.33494590467993,-1.,1.6496563728683));
#23070=CARTESIAN_POINT('Ctrl Pts',(-1.33368890676572,-1.,1.6434717485603));
#23071=CARTESIAN_POINT('Ctrl Pts',(-1.33239425103724,-1.,1.63730653475089));
#23072=CARTESIAN_POINT('Ctrl Pts',(-1.33106149345645,-1.,1.63116079730923));
#23073=CARTESIAN_POINT('Ctrl Pts',(-1.3296901950568,-1.,1.62503464209797));
#23074=CARTESIAN_POINT('Ctrl Pts',(-1.32828000610449,-1.,1.61892832270724));
#23075=CARTESIAN_POINT('Ctrl Pts',(-1.32683074483356,-1.,1.6128423401575));
#23076=CARTESIAN_POINT('Ctrl Pts',(-1.32534250785782,-1.,1.60677758290954));
#23077=CARTESIAN_POINT('Ctrl Pts',(-1.32381550858256,-1.,1.60073511858687));
#23078=CARTESIAN_POINT('Ctrl Pts',(-1.32224985747682,-1.,1.59471591079403));
#23079=CARTESIAN_POINT('Ctrl Pts',(-1.32064537110892,-1.,1.58872057258245));
#23080=CARTESIAN_POINT('Ctrl Pts',(-1.31900135021432,-1.,1.58274907898834));
#23081=CARTESIAN_POINT('Ctrl Pts',(-1.31731642317187,-1.,1.5768005650559));
#23082=CARTESIAN_POINT('Ctrl Pts',(-1.31558903860016,-1.,1.57087397835723));
#23083=CARTESIAN_POINT('Ctrl Pts',(-1.31381795281002,-1.,1.56496872402353));
#23084=CARTESIAN_POINT('Ctrl Pts',(-1.31200264341696,-1.,1.55908521254821));
#23085=CARTESIAN_POINT('Ctrl Pts',(-1.31014393684222,-1.,1.55322568759481));
#23086=CARTESIAN_POINT('Ctrl Pts',(-1.30824393907473,-1.,1.54739413957185));
#23087=CARTESIAN_POINT('Ctrl Pts',(-1.30630475189556,-1.,1.54159462645432));
#23088=CARTESIAN_POINT('Ctrl Pts',(-1.30432735639489,-1.,1.53582981268977));
#23089=CARTESIAN_POINT('Ctrl Pts',(-1.30231064395568,-1.,1.53009970283891));
#23090=CARTESIAN_POINT('Ctrl Pts',(-1.30024984366328,-1.,1.52439957861062));
#23091=CARTESIAN_POINT('Ctrl Pts',(-1.29813791800747,-1.,1.51872184912724));
#23092=CARTESIAN_POINT('Ctrl Pts',(-1.29596850710509,-1.,1.51305994241402));
#23093=CARTESIAN_POINT('Ctrl Pts',(-1.29373841372842,-1.,1.50741159078365));
#23094=CARTESIAN_POINT('Ctrl Pts',(-1.29145022885181,-1.,1.50178230149776));
#23095=CARTESIAN_POINT('Ctrl Pts',(-1.28911506584254,-1.,1.49618896881754));
#23096=CARTESIAN_POINT('Ctrl Pts',(-1.2867467611644,-1.,1.4906522831278));
#23097=CARTESIAN_POINT('Ctrl Pts',(-1.28435533880201,-1.,1.4851881711891));
#23098=CARTESIAN_POINT('Ctrl Pts',(-1.28194158939517,-1.,1.47980070347095));
#23099=CARTESIAN_POINT('Ctrl Pts',(-1.2794891824849,-1.,1.4744717526707));
#23100=CARTESIAN_POINT('Ctrl Pts',(-1.27696414831089,-1.,1.46916035917133));
#23101=CARTESIAN_POINT('Ctrl Pts',(-1.27433119897822,-1.,1.46382431332476));
#23102=CARTESIAN_POINT('Ctrl Pts',(-1.27156805265289,-1.,1.45843906294697));
#23103=CARTESIAN_POINT('Ctrl Pts',(-1.2686778680489,-1.,1.45301422764247));
#23104=CARTESIAN_POINT('Ctrl Pts',(-1.26570925118868,-1.,1.44761985001662));
#23105=CARTESIAN_POINT('Ctrl Pts',(-1.26273903323859,-1.,1.44236470511303));
#23106=CARTESIAN_POINT('Ctrl Pts',(-1.25983531012005,-1.,1.43734919180848));
#23107=CARTESIAN_POINT('Ctrl Pts',(-1.25702687965755,-1.,1.43262645609691));
#23108=CARTESIAN_POINT('Ctrl Pts',(-1.25426945222639,-1.,1.42815938799387));
#23109=CARTESIAN_POINT('Ctrl Pts',(-1.2514145557001,-1.,1.42378102115575));
#23110=CARTESIAN_POINT('Ctrl Pts',(-1.24824430986571,-1.,1.41923722596025));
#23111=CARTESIAN_POINT('Ctrl Pts',(-1.24450600513056,-1.,1.41422913175179));
#23112=CARTESIAN_POINT('Ctrl Pts',(-1.23994455029534,-1.,1.40845295531283));
#23113=CARTESIAN_POINT('Ctrl Pts',(-1.23434087290423,-1.,1.40164708206106));
#23114=CARTESIAN_POINT('Ctrl Pts',(-1.22752961899387,-1.,1.39361389568796));
#23115=CARTESIAN_POINT('Ctrl Pts',(-1.21938737280852,-1.,1.38420564527715));
#23116=CARTESIAN_POINT('Ctrl Pts',(-1.20982812925645,-1.,1.37331915607905));
#23117=CARTESIAN_POINT('Ctrl Pts',(-1.1987959077932,-1.,1.36088705043885));
#23118=CARTESIAN_POINT('Ctrl Pts',(-1.18625865667441,-1.,1.34687054001093));
#23119=CARTESIAN_POINT('Ctrl Pts',(-1.17501305789857,-1.,1.33437539347008));
#23120=CARTESIAN_POINT('Ctrl Pts',(-1.16589330093588,-1.,1.32428080721772));
#23121=CARTESIAN_POINT('Ctrl Pts',(-1.15950888730809,-1.,1.31722977216397));
#23122=CARTESIAN_POINT('Ctrl Pts',(-1.15624053661742,-1.,1.31362392696032));
#23123=CARTESIAN_POINT('',(-1.31362392696033,-1.,1.15624053661742));
#23124=CARTESIAN_POINT('Origin',(0.,-1.,0.));
#23125=CARTESIAN_POINT('',(-1.73811241238545,-1.,1.34869019493419));
#23126=CARTESIAN_POINT('Ctrl Pts',(-1.31362392696033,-1.,1.15624053661742));
#23127=CARTESIAN_POINT('Ctrl Pts',(-1.3172297721596,-1.,1.15950888730433));
#23128=CARTESIAN_POINT('Ctrl Pts',(-1.32428080720544,-1.,1.16589330092532));
#23129=CARTESIAN_POINT('Ctrl Pts',(-1.33437539344842,-1.,1.17501305787994));
#23130=CARTESIAN_POINT('Ctrl Pts',(-1.34687053998157,-1.,1.18625865664915));
#23131=CARTESIAN_POINT('Ctrl Pts',(-1.36088705040677,-1.,1.1987959077656));
#23132=CARTESIAN_POINT('Ctrl Pts',(-1.37331915604962,-1.,1.20982812923113));
#23133=CARTESIAN_POINT('Ctrl Pts',(-1.38420564525391,-1.,1.21938737278853));
#23134=CARTESIAN_POINT('Ctrl Pts',(-1.39361389567257,-1.,1.22752961898063));
#23135=CARTESIAN_POINT('Ctrl Pts',(-1.40164708205345,-1.,1.23434087289768));
#23136=CARTESIAN_POINT('Ctrl Pts',(-1.40845295531151,-1.,1.23994455029421));
#23137=CARTESIAN_POINT('Ctrl Pts',(-1.41422913175437,-1.,1.24450600513278));
#23138=CARTESIAN_POINT('Ctrl Pts',(-1.41923722596421,-1.,1.24824430986911));
#23139=CARTESIAN_POINT('Ctrl Pts',(-1.42378102115911,-1.,1.25141455570299));
#23140=CARTESIAN_POINT('Ctrl Pts',(-1.42815938799555,-1.,1.25426945222783));
#23141=CARTESIAN_POINT('Ctrl Pts',(-1.43262645609679,-1.,1.25702687965744));
#23142=CARTESIAN_POINT('Ctrl Pts',(-1.43734919180719,-1.,1.25983531011894));
#23143=CARTESIAN_POINT('Ctrl Pts',(-1.44236470511145,-1.,1.26273903323723));
#23144=CARTESIAN_POINT('Ctrl Pts',(-1.44761985001544,-1.,1.26570925118767));
#23145=CARTESIAN_POINT('Ctrl Pts',(-1.45301422764205,-1.,1.26867786804854));
#23146=CARTESIAN_POINT('Ctrl Pts',(-1.45843906294725,-1.,1.27156805265312));
#23147=CARTESIAN_POINT('Ctrl Pts',(-1.4638243133254,-1.,1.27433119897877));
#23148=CARTESIAN_POINT('Ctrl Pts',(-1.46916035917197,-1.,1.27696414831144));
#23149=CARTESIAN_POINT('Ctrl Pts',(-1.4744717526711,-1.,1.27948918248524));
#23150=CARTESIAN_POINT('Ctrl Pts',(-1.47980070347102,-1.,1.28194158939522));
#23151=CARTESIAN_POINT('Ctrl Pts',(-1.48518817118891,-1.,1.28435533880184));
#23152=CARTESIAN_POINT('Ctrl Pts',(-1.4906522831275,-1.,1.28674676116415));
#23153=CARTESIAN_POINT('Ctrl Pts',(-1.49618896881729,-1.,1.28911506584232));
#23154=CARTESIAN_POINT('Ctrl Pts',(-1.50178230149764,-1.,1.29145022885171));
#23155=CARTESIAN_POINT('Ctrl Pts',(-1.50741159078367,-1.,1.29373841372843));
#23156=CARTESIAN_POINT('Ctrl Pts',(-1.51305994241412,-1.,1.29596850710518));
#23157=CARTESIAN_POINT('Ctrl Pts',(-1.51872184912735,-1.,1.29813791800757));
#23158=CARTESIAN_POINT('Ctrl Pts',(-1.5243995786107,-1.,1.30024984366334));
#23159=CARTESIAN_POINT('Ctrl Pts',(-1.53009970283893,-1.,1.3023106439557));
#23160=CARTESIAN_POINT('Ctrl Pts',(-1.53582981268976,-1.,1.30432735639487));
#23161=CARTESIAN_POINT('Ctrl Pts',(-1.54159462645428,-1.,1.30630475189553));
#23162=CARTESIAN_POINT('Ctrl Pts',(-1.54739413957183,-1.,1.30824393907471));
#23163=CARTESIAN_POINT('Ctrl Pts',(-1.55322568759481,-1.,1.31014393684221));
#23164=CARTESIAN_POINT('Ctrl Pts',(-1.55908521254822,-1.,1.31200264341696));
#23165=CARTESIAN_POINT('Ctrl Pts',(-1.56496872402352,-1.,1.31381795281002));
#23166=CARTESIAN_POINT('Ctrl Pts',(-1.57087397835721,-1.,1.31558903860015));
#23167=CARTESIAN_POINT('Ctrl Pts',(-1.57680056505585,-1.,1.31731642317183));
#23168=CARTESIAN_POINT('Ctrl Pts',(-1.58274907898829,-1.,1.31900135021428));
#23169=CARTESIAN_POINT('Ctrl Pts',(-1.58872057258244,-1.,1.32064537110891));
#23170=CARTESIAN_POINT('Ctrl Pts',(-1.59471591079408,-1.,1.32224985747686));
#23171=CARTESIAN_POINT('Ctrl Pts',(-1.600735118587,-1.,1.32381550858266));
#23172=CARTESIAN_POINT('Ctrl Pts',(-1.6067775829097,-1.,1.32534250785794));
#23173=CARTESIAN_POINT('Ctrl Pts',(-1.61284234015762,-1.,1.32683074483365));
#23174=CARTESIAN_POINT('Ctrl Pts',(-1.61892832270723,-1.,1.32828000610448));
#23175=CARTESIAN_POINT('Ctrl Pts',(-1.62503464209777,-1.,1.32969019505665));
#23176=CARTESIAN_POINT('Ctrl Pts',(-1.63116079730887,-1.,1.33106149345618));
#23177=CARTESIAN_POINT('Ctrl Pts',(-1.6373065347505,-1.,1.33239425103694));
#23178=CARTESIAN_POINT('Ctrl Pts',(-1.64347174856007,-1.,1.33368890676554));
#23179=CARTESIAN_POINT('Ctrl Pts',(-1.64965637286843,-1.,1.33494590468003));
#23180=CARTESIAN_POINT('Ctrl Pts',(-1.65586025952651,-1.,1.33616559745217));
#23181=CARTESIAN_POINT('Ctrl Pts',(-1.66208312542073,-1.,1.33734820885331));
#23182=CARTESIAN_POINT('Ctrl Pts',(-1.66832460784078,-1.,1.33849388654458));
#23183=CARTESIAN_POINT('Ctrl Pts',(-1.67458429426126,-1.,1.33960273470372));
#23184=CARTESIAN_POINT('Ctrl Pts',(-1.68086176030308,-1.,1.3406748518516));
#23185=CARTESIAN_POINT('Ctrl Pts',(-1.68715660868602,-1.,1.34171037484673));
#23186=CARTESIAN_POINT('Ctrl Pts',(-1.6934684849664,-1.,1.34270948206139));
#23187=CARTESIAN_POINT('Ctrl Pts',(-1.69979707754221,-1.,1.34367237124322));
#23188=CARTESIAN_POINT('Ctrl Pts',(-1.70614212266676,-1.,1.34459924533783));
#23189=CARTESIAN_POINT('Ctrl Pts',(-1.71250340687011,-1.,1.34549029589563));
#23190=CARTESIAN_POINT('Ctrl Pts',(-1.7188807715095,-1.,1.34634568653586));
#23191=CARTESIAN_POINT('Ctrl Pts',(-1.72527410681298,-1.,1.34716554820013));
#23192=CARTESIAN_POINT('Ctrl Pts',(-1.73040149654497,-1.,1.3477930915247));
#23193=CARTESIAN_POINT('Ctrl Pts',(-1.73425417886255,-1.,1.34824783113158));
#23194=CARTESIAN_POINT('Ctrl Pts',(-1.73682580585819,-1.,1.34854391898145));
#23195=CARTESIAN_POINT('Ctrl Pts',(-1.73811241238545,-1.,1.34869019493419));
#23196=CARTESIAN_POINT('',(-1.81978687191668,-1.,1.23627494547115));
#23197=CARTESIAN_POINT('',(-1.73811241238545,-1.,1.34869019493419));
#23198=CARTESIAN_POINT('',(-1.5055822144029,-1.,0.892032620296855));
#23199=CARTESIAN_POINT('Ctrl Pts',(-1.81978687191668,-1.,1.23627494547115));
#23200=CARTESIAN_POINT('Ctrl Pts',(-1.81925017193531,-1.,1.23509651170384));
#23201=CARTESIAN_POINT('Ctrl Pts',(-1.81817389920914,-1.,1.23274224526804));
#23202=CARTESIAN_POINT('Ctrl Pts',(-1.81655087183054,-1.,1.22921864890975));
#23203=CARTESIAN_POINT('Ctrl Pts',(-1.81436959209778,-1.,1.22453613304507));
#23204=CARTESIAN_POINT('Ctrl Pts',(-1.81161420806172,-1.,1.2187090610323));
#23205=CARTESIAN_POINT('Ctrl Pts',(-1.80882996916931,-1.,1.2129081570818));
#23206=CARTESIAN_POINT('Ctrl Pts',(-1.80601678480772,-1.,1.20713356605519));
#23207=CARTESIAN_POINT('Ctrl Pts',(-1.8031745483882,-1.,1.2013854893912));
#23208=CARTESIAN_POINT('Ctrl Pts',(-1.80030314370121,-1.,1.19566418930405));
#23209=CARTESIAN_POINT('Ctrl Pts',(-1.79740245923649,-1.,1.1899699793456));
#23210=CARTESIAN_POINT('Ctrl Pts',(-1.79447240321572,-1.,1.18430321697471));
#23211=CARTESIAN_POINT('Ctrl Pts',(-1.79151291552646,-1.,1.17866429440781));
#23212=CARTESIAN_POINT('Ctrl Pts',(-1.78852398877523,-1.,1.17305363177265));
#23213=CARTESIAN_POINT('Ctrl Pts',(-1.78550566040349,-1.,1.16747166312239));
#23214=CARTESIAN_POINT('Ctrl Pts',(-1.78245795880949,-1.,1.16191881298458));
#23215=CARTESIAN_POINT('Ctrl Pts',(-1.77938085564261,-1.,1.15639547194689));
#23216=CARTESIAN_POINT('Ctrl Pts',(-1.77627422557034,-1.,1.15090197841531));
#23217=CARTESIAN_POINT('Ctrl Pts',(-1.77313777896234,-1.,1.14543858226948));
#23218=CARTESIAN_POINT('Ctrl Pts',(-1.76997111386806,-1.,1.14000548337));
#23219=CARTESIAN_POINT('Ctrl Pts',(-1.76677384551883,-1.,1.13460291804635));
#23220=CARTESIAN_POINT('Ctrl Pts',(-1.76354571966171,-1.,1.12923123555076));
#23221=CARTESIAN_POINT('Ctrl Pts',(-1.76028671825084,-1.,1.12389096855078));
#23222=CARTESIAN_POINT('Ctrl Pts',(-1.75699720772089,-1.,1.11858293216752));
#23223=CARTESIAN_POINT('Ctrl Pts',(-1.75367772094617,-1.,1.11330807582542));
#23224=CARTESIAN_POINT('Ctrl Pts',(-1.75032866075914,-1.,1.10806728183003));
#23225=CARTESIAN_POINT('Ctrl Pts',(-1.74695004214924,-1.,1.10286118991144));
#23226=CARTESIAN_POINT('Ctrl Pts',(-1.74354119236212,-1.,1.09768999241229));
#23227=CARTESIAN_POINT('Ctrl Pts',(-1.74010053962252,-1.,1.09255329056496));
#23228=CARTESIAN_POINT('Ctrl Pts',(-1.73662628326093,-1.,1.08745056285429));
#23229=CARTESIAN_POINT('Ctrl Pts',(-1.73311705663407,-1.,1.08238162784749));
#23230=CARTESIAN_POINT('Ctrl Pts',(-1.72957248977424,-1.,1.0773470373727));
#23231=CARTESIAN_POINT('Ctrl Pts',(-1.72599406198489,-1.,1.07234866990252));
#23232=CARTESIAN_POINT('Ctrl Pts',(-1.72238500928456,-1.,1.06738966975463));
#23233=CARTESIAN_POINT('Ctrl Pts',(-1.71874858456908,-1.,1.0624732468065));
#23234=CARTESIAN_POINT('Ctrl Pts',(-1.71508654427022,-1.,1.05760163192481));
#23235=CARTESIAN_POINT('Ctrl Pts',(-1.71139783543986,-1.,1.05277517202854));
#23236=CARTESIAN_POINT('Ctrl Pts',(-1.70767646263641,-1.,1.0479908540499));
#23237=CARTESIAN_POINT('Ctrl Pts',(-1.70391338707969,-1.,1.04324363334546));
#23238=CARTESIAN_POINT('Ctrl Pts',(-1.70010052930951,-1.,1.03852922490782));
#23239=CARTESIAN_POINT('Ctrl Pts',(-1.69623414782769,-1.,1.03384646003587));
#23240=CARTESIAN_POINT('Ctrl Pts',(-1.69231840863471,-1.,1.02919977579155));
#23241=CARTESIAN_POINT('Ctrl Pts',(-1.68836910178475,-1.,1.02460180535272));
#23242=CARTESIAN_POINT('Ctrl Pts',(-1.68440578021739,-1.,1.02006795074222));
#23243=CARTESIAN_POINT('Ctrl Pts',(-1.6804428989482,-1.,1.01561026162787));
#23244=CARTESIAN_POINT('Ctrl Pts',(-1.67648246776457,-1.,1.01123236493507));
#23245=CARTESIAN_POINT('Ctrl Pts',(-1.67250335383248,-1.,1.00692206696387));
#23246=CARTESIAN_POINT('Ctrl Pts',(-1.66846059277231,-1.,1.00265091003682));
#23247=CARTESIAN_POINT('Ctrl Pts',(-1.66430758030304,-1.,0.998389654952317));
#23248=CARTESIAN_POINT('Ctrl Pts',(-1.66001553809916,-1.,0.994121836661116));
#23249=CARTESIAN_POINT('Ctrl Pts',(-1.65559044289746,-1.,0.98985562785445));
#23250=CARTESIAN_POINT('Ctrl Pts',(-1.6511001661277,-1.,0.985642622921626));
#23251=CARTESIAN_POINT('Ctrl Pts',(-1.64665139190834,-1.,0.981562530940574));
#23252=CARTESIAN_POINT('Ctrl Pts',(-1.64233990826831,-1.,0.977689794120297));
#23253=CARTESIAN_POINT('Ctrl Pts',(-1.63820952658157,-1.,0.974066058287501));
#23254=CARTESIAN_POINT('Ctrl Pts',(-1.63420665729609,-1.,0.970669715996356));
#23255=CARTESIAN_POINT('Ctrl Pts',(-1.63013849959083,-1.,0.967387853228041));
#23256=CARTESIAN_POINT('Ctrl Pts',(-1.6257193066974,-1.,0.964046107037821));
#23257=CARTESIAN_POINT('Ctrl Pts',(-1.62061638139929,-1.,0.960438326099958));
#23258=CARTESIAN_POINT('Ctrl Pts',(-1.61449324337233,-1.,0.956354422921573));
#23259=CARTESIAN_POINT('Ctrl Pts',(-1.60706069897794,-1.,0.951613284361248));
#23260=CARTESIAN_POINT('Ctrl Pts',(-1.59810042045408,-1.,0.946078063325796));
#23261=CARTESIAN_POINT('Ctrl Pts',(-1.58744937489796,-1.,0.939646377909319));
#23262=CARTESIAN_POINT('Ctrl Pts',(-1.57499388385561,-1.,0.932246680128849));
#23263=CARTESIAN_POINT('Ctrl Pts',(-1.56065988582509,-1.,0.923832188966322));
#23264=CARTESIAN_POINT('Ctrl Pts',(-1.54440491152808,-1.,0.91437591904658));
#23265=CARTESIAN_POINT('Ctrl Pts',(-1.52984849890434,-1.,0.905967409640499));
#23266=CARTESIAN_POINT('Ctrl Pts',(-1.51805569591479,-1.,0.89918504749193));
#23267=CARTESIAN_POINT('Ctrl Pts',(-1.50980486807181,-1.,0.894452006967538));
#23268=CARTESIAN_POINT('Ctrl Pts',(-1.5055822144029,-1.,0.892032620296855));
#23269=CARTESIAN_POINT('',(-1.60662857109684,-1.,0.693717979106305));
#23270=CARTESIAN_POINT('Origin',(0.,-1.,0.));
#23271=CARTESIAN_POINT('',(-2.0698113262342,-1.,0.7455743247944));
#23272=CARTESIAN_POINT('Ctrl Pts',(-1.60662857109684,-1.,0.693717979106305));
#23273=CARTESIAN_POINT('Ctrl Pts',(-1.61106790957619,-1.,0.69571209787897));
#23274=CARTESIAN_POINT('Ctrl Pts',(-1.61974673471117,-1.,0.699605146398837));
#23275=CARTESIAN_POINT('Ctrl Pts',(-1.6321654166204,-1.,0.705159151977294));
#23276=CARTESIAN_POINT('Ctrl Pts',(-1.64752408828442,-1.,0.711993139340447));
#23277=CARTESIAN_POINT('Ctrl Pts',(-1.66472880551777,-1.,0.71958543378795));
#23278=CARTESIAN_POINT('Ctrl Pts',(-1.67996158451922,-1.,0.726235967982445));
#23279=CARTESIAN_POINT('Ctrl Pts',(-1.69326921972915,-1.,0.731963238685357));
#23280=CARTESIAN_POINT('Ctrl Pts',(-1.70473309004249,-1.,0.736799665716932));
#23281=CARTESIAN_POINT('Ctrl Pts',(-1.71447789751001,-1.,0.74079516202821));
#23282=CARTESIAN_POINT('Ctrl Pts',(-1.72268229916769,-1.,0.744021445433093));
#23283=CARTESIAN_POINT('Ctrl Pts',(-1.72958533647714,-1.,0.746574710097752));
#23284=CARTESIAN_POINT('Ctrl Pts',(-1.7355035168033,-1.,0.74858246295687));
#23285=CARTESIAN_POINT('Ctrl Pts',(-1.74080458267114,-1.,0.750193435981249));
#23286=CARTESIAN_POINT('Ctrl Pts',(-1.74585086852502,-1.,0.751555614164482));
#23287=CARTESIAN_POINT('Ctrl Pts',(-1.75095139468794,-1.,0.752797683531314));
#23288=CARTESIAN_POINT('Ctrl Pts',(-1.75631083600019,-1.,0.754009254027829));
#23289=CARTESIAN_POINT('Ctrl Pts',(-1.76197817240128,-1.,0.755220979974461));
#23290=CARTESIAN_POINT('Ctrl Pts',(-1.76789396002998,-1.,0.75642189602781));
#23291=CARTESIAN_POINT('Ctrl Pts',(-1.77394167108292,-1.,0.757578264077029));
#23292=CARTESIAN_POINT('Ctrl Pts',(-1.77999411220945,-1.,0.758650626677518));
#23293=CARTESIAN_POINT('Ctrl Pts',(-1.78596964884604,-1.,0.759614401110189));
#23294=CARTESIAN_POINT('Ctrl Pts',(-1.7918581561088,-1.,0.760469555880749));
#23295=CARTESIAN_POINT('Ctrl Pts',(-1.79768986997783,-1.,0.761229695230558));
#23296=CARTESIAN_POINT('Ctrl Pts',(-1.80351583877342,-1.,0.761915336443547));
#23297=CARTESIAN_POINT('Ctrl Pts',(-1.80938551463965,-1.,0.762546129463938));
#23298=CARTESIAN_POINT('Ctrl Pts',(-1.8153211840553,-1.,0.763132003836634));
#23299=CARTESIAN_POINT('Ctrl Pts',(-1.82131873145266,-1.,0.763673465462726));
#23300=CARTESIAN_POINT('Ctrl Pts',(-1.82735991200065,-1.,0.764165902605995));
#23301=CARTESIAN_POINT('Ctrl Pts',(-1.83342077227142,-1.,0.764602549687853));
#23302=CARTESIAN_POINT('Ctrl Pts',(-1.83948181064835,-1.,0.764978057881737));
#23303=CARTESIAN_POINT('Ctrl Pts',(-1.84553698875924,-1.,0.765291664862029));
#23304=CARTESIAN_POINT('Ctrl Pts',(-1.85158945130063,-1.,0.765545710619062));
#23305=CARTESIAN_POINT('Ctrl Pts',(-1.85764741390394,-1.,0.765744212909318));
#23306=CARTESIAN_POINT('Ctrl Pts',(-1.86372027063312,-1.,0.765891519092547));
#23307=CARTESIAN_POINT('Ctrl Pts',(-1.86981398314341,-1.,0.765990708546091));
#23308=CARTESIAN_POINT('Ctrl Pts',(-1.87592888967883,-1.,0.766042837036744));
#23309=CARTESIAN_POINT('Ctrl Pts',(-1.88206215302561,-1.,0.766047794851864));
#23310=CARTESIAN_POINT('Ctrl Pts',(-1.88820926433409,-1.,0.766004837062091));
#23311=CARTESIAN_POINT('Ctrl Pts',(-1.89436577771388,-1.,0.765913193856978));
#23312=CARTESIAN_POINT('Ctrl Pts',(-1.90052930393596,-1.,0.765772772593386));
#23313=CARTESIAN_POINT('Ctrl Pts',(-1.90669961402356,-1.,0.765584196937919));
#23314=CARTESIAN_POINT('Ctrl Pts',(-1.91287765805169,-1.,0.765348465884722));
#23315=CARTESIAN_POINT('Ctrl Pts',(-1.91906491634196,-1.,0.765066729667088));
#23316=CARTESIAN_POINT('Ctrl Pts',(-1.92526263537048,-1.,0.764740025488211));
#23317=CARTESIAN_POINT('Ctrl Pts',(-1.93147105496382,-1.,0.76436901067394));
#23318=CARTESIAN_POINT('Ctrl Pts',(-1.93768964875886,-1.,0.763954049121458));
#23319=CARTESIAN_POINT('Ctrl Pts',(-1.9439174661764,-1.,0.763495333538629));
#23320=CARTESIAN_POINT('Ctrl Pts',(-1.95015342590024,-1.,0.762992990878769));
#23321=CARTESIAN_POINT('Ctrl Pts',(-1.95639665309869,-1.,0.762447203806179));
#23322=CARTESIAN_POINT('Ctrl Pts',(-1.96264672744186,-1.,0.761858300014423));
#23323=CARTESIAN_POINT('Ctrl Pts',(-1.96890351582499,-1.,0.76122669048382));
#23324=CARTESIAN_POINT('Ctrl Pts',(-1.97516705321494,-1.,0.760552825409757));
#23325=CARTESIAN_POINT('Ctrl Pts',(-1.98143741418172,-1.,0.75983714745219));
#23326=CARTESIAN_POINT('Ctrl Pts',(-1.98771456680874,-1.,0.759080037802488));
#23327=CARTESIAN_POINT('Ctrl Pts',(-1.99399831098817,-1.,0.758281796766761));
#23328=CARTESIAN_POINT('Ctrl Pts',(-2.00028834739178,-1.,0.757442676862724));
#23329=CARTESIAN_POINT('Ctrl Pts',(-2.0065843158773,-1.,0.75656290464667));
#23330=CARTESIAN_POINT('Ctrl Pts',(-2.01288584328084,-1.,0.755642704957865));
#23331=CARTESIAN_POINT('Ctrl Pts',(-2.01919259405809,-1.,0.754682330722816));
#23332=CARTESIAN_POINT('Ctrl Pts',(-2.02550428623313,-1.,0.753682061112768));
#23333=CARTESIAN_POINT('Ctrl Pts',(-2.03182068456221,-1.,0.752642180487211));
#23334=CARTESIAN_POINT('Ctrl Pts',(-2.03814160092099,-1.,0.751562963361115));
#23335=CARTESIAN_POINT('Ctrl Pts',(-2.04446689147979,-1.,0.750444657875576));
#23336=CARTESIAN_POINT('Ctrl Pts',(-2.05079645592154,-1.,0.749287468665046));
#23337=CARTESIAN_POINT('Ctrl Pts',(-2.05713023031006,-1.,0.748091554183802));
#23338=CARTESIAN_POINT('Ctrl Pts',(-2.06220058927826,-1.,0.747103932787919));
#23339=CARTESIAN_POINT('Ctrl Pts',(-2.06600523016815,-1.,0.7463458715442));
#23340=CARTESIAN_POINT('Ctrl Pts',(-2.06854248895728,-1.,0.745832791378367));
#23341=CARTESIAN_POINT('Ctrl Pts',(-2.0698113262342,-1.,0.7455743247944));
#23342=CARTESIAN_POINT('',(-2.11275013067528,-1.,0.61342227326009));
#23343=CARTESIAN_POINT('',(-2.0698113262342,-1.,0.7455743247944));
#23344=CARTESIAN_POINT('',(-1.7075470150345,-1.,0.383122945602004));
#23345=CARTESIAN_POINT('Ctrl Pts',(-2.11275013067528,-1.,0.61342227326009));
#23346=CARTESIAN_POINT('Ctrl Pts',(-2.11187554259986,-1.,0.6124673655618));
#23347=CARTESIAN_POINT('Ctrl Pts',(-2.11012443807238,-1.,0.610560911689899));
#23348=CARTESIAN_POINT('Ctrl Pts',(-2.1074919961518,-1.,0.607711315454876));
#23349=CARTESIAN_POINT('Ctrl Pts',(-2.10397049886949,-1.,0.60393203073603));
#23350=CARTESIAN_POINT('Ctrl Pts',(-2.0995493086477,-1.,0.599241616420533));
#23351=CARTESIAN_POINT('Ctrl Pts',(-2.0951087622027,-1.,0.594585006052162));
#23352=CARTESIAN_POINT('Ctrl Pts',(-2.09064881812129,-1.,0.589962365403406));
#23353=CARTESIAN_POINT('Ctrl Pts',(-2.08616943727951,-1.,0.585373918991617));
#23354=CARTESIAN_POINT('Ctrl Pts',(-2.08167059018418,-1.,0.580819952108063));
#23355=CARTESIAN_POINT('Ctrl Pts',(-2.07715226767559,-1.,0.576300797416844));
#23356=CARTESIAN_POINT('Ctrl Pts',(-2.07261449292824,-1.,0.571816823242603));
#23357=CARTESIAN_POINT('Ctrl Pts',(-2.06805732997334,-1.,0.567368421181087));
#23358=CARTESIAN_POINT('Ctrl Pts',(-2.06348090160589,-1.,0.562955993082261));
#23359=CARTESIAN_POINT('Ctrl Pts',(-2.05888537756462,-1.,0.558579940185151));
#23360=CARTESIAN_POINT('Ctrl Pts',(-2.05427091604413,-1.,0.554240657463906));
#23361=CARTESIAN_POINT('Ctrl Pts',(-2.04963761077958,-1.,0.549938525150295));
#23362=CARTESIAN_POINT('Ctrl Pts',(-2.04498544714588,-1.,0.54567390381743));
#23363=CARTESIAN_POINT('Ctrl Pts',(-2.04031422690527,-1.,0.541447120615659));
#23364=CARTESIAN_POINT('Ctrl Pts',(-2.03562362954037,-1.,0.537258489833262));
#23365=CARTESIAN_POINT('Ctrl Pts',(-2.03091336214426,-1.,0.533108355132976));
#23366=CARTESIAN_POINT('Ctrl Pts',(-2.0261832908329,-1.,0.528997127241914));
#23367=CARTESIAN_POINT('Ctrl Pts',(-2.02143356304698,-1.,0.524925318333476));
#23368=CARTESIAN_POINT('Ctrl Pts',(-2.01666477917286,-1.,0.52089359039937));
#23369=CARTESIAN_POINT('Ctrl Pts',(-2.01187773939242,-1.,0.516902681728687));
#23370=CARTESIAN_POINT('Ctrl Pts',(-2.00707309946949,-1.,0.512953306961792));
#23371=CARTESIAN_POINT('Ctrl Pts',(-2.00225107134734,-1.,0.509046069886157));
#23372=CARTESIAN_POINT('Ctrl Pts',(-1.99741107463572,-1.,0.505181361323026));
#23373=CARTESIAN_POINT('Ctrl Pts',(-1.99255149126155,-1.,0.501359287727146));
#23374=CARTESIAN_POINT('Ctrl Pts',(-1.98767044752932,-1.,0.497579909545574));
#23375=CARTESIAN_POINT('Ctrl Pts',(-1.98276658761821,-1.,0.493843476541494));
#23376=CARTESIAN_POINT('Ctrl Pts',(-1.97783973019229,-1.,0.490150627860952));
#23377=CARTESIAN_POINT('Ctrl Pts',(-1.97289186263272,-1.,0.486502692907659));
#23378=CARTESIAN_POINT('Ctrl Pts',(-1.96792703422362,-1.,0.48290166212069));
#23379=CARTESIAN_POINT('Ctrl Pts',(-1.96294933055943,-1.,0.479349583074855));
#23380=CARTESIAN_POINT('Ctrl Pts',(-1.95796111148177,-1.,0.475848034683176));
#23381=CARTESIAN_POINT('Ctrl Pts',(-1.95296148278133,-1.,0.472397672264072));
#23382=CARTESIAN_POINT('Ctrl Pts',(-1.94794381136514,-1.,0.468997482913135));
#23383=CARTESIAN_POINT('Ctrl Pts',(-1.9428979419619,-1.,0.46564546202603));
#23384=CARTESIAN_POINT('Ctrl Pts',(-1.93781486640821,-1.,0.462340031009056));
#23385=CARTESIAN_POINT('Ctrl Pts',(-1.93269066517934,-1.,0.459081234547926));
#23386=CARTESIAN_POINT('Ctrl Pts',(-1.92753067150476,-1.,0.455872005174371));
#23387=CARTESIAN_POINT('Ctrl Pts',(-1.92235380648502,-1.,0.452719478359432));
#23388=CARTESIAN_POINT('Ctrl Pts',(-1.91718342555755,-1.,0.449632260106662));
#23389=CARTESIAN_POINT('Ctrl Pts',(-1.9120369998112,-1.,0.446617343485711));
#23390=CARTESIAN_POINT('Ctrl Pts',(-1.90691756144898,-1.,0.44367755684915));
#23391=CARTESIAN_POINT('Ctrl Pts',(-1.90180124389086,-1.,0.440807833704038));
#23392=CARTESIAN_POINT('Ctrl Pts',(-1.89663648956466,-1.,0.437995003948244));
#23393=CARTESIAN_POINT('Ctrl Pts',(-1.89136993975504,-1.,0.435225660963383));
#23394=CARTESIAN_POINT('Ctrl Pts',(-1.88596913666793,-1.,0.432493038548748));
#23395=CARTESIAN_POINT('Ctrl Pts',(-1.88044229001832,-1.,0.429803062482344));
#23396=CARTESIAN_POINT('Ctrl Pts',(-1.87486989291484,-1.,0.427183828519102));
#23397=CARTESIAN_POINT('Ctrl Pts',(-1.86937803944323,-1.,0.424678177291359));
#23398=CARTESIAN_POINT('Ctrl Pts',(-1.86408083334028,-1.,0.422327307418275));
#23399=CARTESIAN_POINT('Ctrl Pts',(-1.85903281096686,-1.,0.420157287975619));
#23400=CARTESIAN_POINT('Ctrl Pts',(-1.85417632856234,-1.,0.418164129143534));
#23401=CARTESIAN_POINT('Ctrl Pts',(-1.84929312929882,-1.,0.416300022038864));
#23402=CARTESIAN_POINT('Ctrl Pts',(-1.8440575707371,-1.,0.41448743825434));
#23403=CARTESIAN_POINT('Ctrl Pts',(-1.83808953475839,-1.,0.412633125322161));
#23404=CARTESIAN_POINT('Ctrl Pts',(-1.83100408895216,-1.,0.410641256301675));
#23405=CARTESIAN_POINT('Ctrl Pts',(-1.8224702267854,-1.,0.408428948108533));
#23406=CARTESIAN_POINT('Ctrl Pts',(-1.81223801813988,-1.,0.405933518411838));
#23407=CARTESIAN_POINT('Ctrl Pts',(-1.80012077176221,-1.,0.403107976170441));
#23408=CARTESIAN_POINT('Ctrl Pts',(-1.78598826347533,-1.,0.39991940378308));
#23409=CARTESIAN_POINT('Ctrl Pts',(-1.7697556004756,-1.,0.39634619612042));
#23410=CARTESIAN_POINT('Ctrl Pts',(-1.75137405313962,-1.,0.392375812294307));
#23411=CARTESIAN_POINT('Ctrl Pts',(-1.7349317097561,-1.,0.388877023509191));
#23412=CARTESIAN_POINT('Ctrl Pts',(-1.72162022246158,-1.,0.38607079032701));
#23413=CARTESIAN_POINT('Ctrl Pts',(-1.71231062891958,-1.,0.384119047315542));
#23414=CARTESIAN_POINT('Ctrl Pts',(-1.7075470150345,-1.,0.383122945602004));
#23415=CARTESIAN_POINT('',(-1.74236521665491,-1.,0.163289472382896));
#23416=CARTESIAN_POINT('Origin',(0.,-1.,0.));
#23417=CARTESIAN_POINT('',(-2.19890268624765,-1.,0.069476445021958));
#23418=CARTESIAN_POINT('Ctrl Pts',(-1.74236521665491,-1.,0.163289472382896));
#23419=CARTESIAN_POINT('Ctrl Pts',(-1.7472034950333,-1.,0.163814161002002));
#23420=CARTESIAN_POINT('Ctrl Pts',(-1.75666056638427,-1.,0.164834765707158));
#23421=CARTESIAN_POINT('Ctrl Pts',(-1.77018771684844,-1.,0.1662793551464));
#23422=CARTESIAN_POINT('Ctrl Pts',(-1.7869064998507,-1.,0.168032772805197));
#23423=CARTESIAN_POINT('Ctrl Pts',(-1.80561530629706,-1.,0.169936923904608));
#23424=CARTESIAN_POINT('Ctrl Pts',(-1.82215766811545,-1.,0.171554770204119));
#23425=CARTESIAN_POINT('Ctrl Pts',(-1.83658380527692,-1.,0.1728894428919));
#23426=CARTESIAN_POINT('Ctrl Pts',(-1.8489811319852,-1.,0.173946627587731));
#23427=CARTESIAN_POINT('Ctrl Pts',(-1.85948367088837,-1.,0.17473525927603));
#23428=CARTESIAN_POINT('Ctrl Pts',(-1.86828349694799,-1.,0.175268337590758));
#23429=CARTESIAN_POINT('Ctrl Pts',(-1.87563767773588,-1.,0.175563480746485));
#23430=CARTESIAN_POINT('Ctrl Pts',(-1.88188663145367,-1.,0.175644148889698));
#23431=CARTESIAN_POINT('Ctrl Pts',(-1.88742606273259,-1.,0.175538155840648));
#23432=CARTESIAN_POINT('Ctrl Pts',(-1.892646301985,-1.,0.175274276190844));
#23433=CARTESIAN_POINT('Ctrl Pts',(-1.89788101117132,-1.,0.174879405091263));
#23434=CARTESIAN_POINT('Ctrl Pts',(-1.90335253862834,-1.,0.174375518661085));
#23435=CARTESIAN_POINT('Ctrl Pts',(-1.90911693975267,-1.,0.173776635257817));
#23436=CARTESIAN_POINT('Ctrl Pts',(-1.91511429159527,-1.,0.173090695383496));
#23437=CARTESIAN_POINT('Ctrl Pts',(-1.9212233439798,-1.,0.172321621259514));
#23438=CARTESIAN_POINT('Ctrl Pts',(-1.92731093582036,-1.,0.171471191532988));
#23439=CARTESIAN_POINT('Ctrl Pts',(-1.93329183155539,-1.,0.170541253116201));
#23440=CARTESIAN_POINT('Ctrl Pts',(-1.93915639211581,-1.,0.169534904817491));
#23441=CARTESIAN_POINT('Ctrl Pts',(-1.94493757756931,-1.,0.168455741607556));
#23442=CARTESIAN_POINT('Ctrl Pts',(-1.95069027794294,-1.,0.167307501784475));
#23443=CARTESIAN_POINT('Ctrl Pts',(-1.9564675971873,-1.,0.166093592002812));
#23444=CARTESIAN_POINT('Ctrl Pts',(-1.96229379940136,-1.,0.164816568920269));
#23445=CARTESIAN_POINT('Ctrl Pts',(-1.96816512677967,-1.,0.163478185457734));
#23446=CARTESIAN_POINT('Ctrl Pts',(-1.97406280235188,-1.,0.162079693556288));
#23447=CARTESIAN_POINT('Ctrl Pts',(-1.97996195437559,-1.,0.160622060784611));
#23448=CARTESIAN_POINT('Ctrl Pts',(-1.98584238283292,-1.,0.159106226437299));
#23449=CARTESIAN_POINT('Ctrl Pts',(-1.99169810931908,-1.,0.157533331459227));
#23450=CARTESIAN_POINT('Ctrl Pts',(-1.99753284771497,-1.,0.155904629548783));
#23451=CARTESIAN_POINT('Ctrl Pts',(-2.00335565310543,-1.,0.154221403049722));
#23452=CARTESIAN_POINT('Ctrl Pts',(-2.00917680318424,-1.,0.15248488362145));
#23453=CARTESIAN_POINT('Ctrl Pts',(-2.01500291940238,-1.,0.150696157673078));
#23454=CARTESIAN_POINT('Ctrl Pts',(-2.02083464969894,-1.,0.148856124775337));
#23455=CARTESIAN_POINT('Ctrl Pts',(-2.02666926182017,-1.,0.146965557332583));
#23456=CARTESIAN_POINT('Ctrl Pts',(-2.03250223739942,-1.,0.145025140186057));
#23457=CARTESIAN_POINT('Ctrl Pts',(-2.03832911025912,-1.,0.143035515058209));
#23458=CARTESIAN_POINT('Ctrl Pts',(-2.04414757947916,-1.,0.140997332152546));
#23459=CARTESIAN_POINT('Ctrl Pts',(-2.04995762001328,-1.,0.138911255368966));
#23460=CARTESIAN_POINT('Ctrl Pts',(-2.05576044414264,-1.,0.136777941218043));
#23461=CARTESIAN_POINT('Ctrl Pts',(-2.06155781517842,-1.,0.134598026192106));
#23462=CARTESIAN_POINT('Ctrl Pts',(-2.06735123910326,-1.,0.13237211154771));
#23463=CARTESIAN_POINT('Ctrl Pts',(-2.07314114713063,-1.,0.130100748328403));
#23464=CARTESIAN_POINT('Ctrl Pts',(-2.07892715110987,-1.,0.12778444527612));
#23465=CARTESIAN_POINT('Ctrl Pts',(-2.08470840653643,-1.,0.125423679412061));
#23466=CARTESIAN_POINT('Ctrl Pts',(-2.09048392424825,-1.,0.123018905621083));
#23467=CARTESIAN_POINT('Ctrl Pts',(-2.0962529286773,-1.,0.120570567965122));
#23468=CARTESIAN_POINT('Ctrl Pts',(-2.102015121329,-1.,0.118079107988355));
#23469=CARTESIAN_POINT('Ctrl Pts',(-2.10777050261309,-1.,0.115544957687926));
#23470=CARTESIAN_POINT('Ctrl Pts',(-2.11351924490306,-1.,0.112968534419737));
#23471=CARTESIAN_POINT('Ctrl Pts',(-2.11926155590865,-1.,0.110350236135025));
#23472=CARTESIAN_POINT('Ctrl Pts',(-2.12499752307,-1.,0.10769043523109));
#23473=CARTESIAN_POINT('Ctrl Pts',(-2.13072704887293,-1.,0.104989479152739));
#23474=CARTESIAN_POINT('Ctrl Pts',(-2.13644992667165,-1.,0.1022477005561));
#23475=CARTESIAN_POINT('Ctrl Pts',(-2.14216588396025,-1.,0.0994654261990914));
#23476=CARTESIAN_POINT('Ctrl Pts',(-2.14787463531795,-1.,0.0966429852305457));
#23477=CARTESIAN_POINT('Ctrl Pts',(-2.1535759397817,-1.,0.0937807218867642));
#23478=CARTESIAN_POINT('Ctrl Pts',(-2.15926961544516,-1.,0.0908789888107264));
#23479=CARTESIAN_POINT('Ctrl Pts',(-2.16495552645014,-1.,0.0879381291386921));
#23480=CARTESIAN_POINT('Ctrl Pts',(-2.17063357870952,-1.,0.0849584620835371));
#23481=CARTESIAN_POINT('Ctrl Pts',(-2.176303712113,-1.,0.0819402680872764));
#23482=CARTESIAN_POINT('Ctrl Pts',(-2.18196589448887,-1.,0.0788837727685241));
#23483=CARTESIAN_POINT('Ctrl Pts',(-2.1876201139953,-1.,0.0757891465836146));
#23484=CARTESIAN_POINT('Ctrl Pts',(-2.19213712013662,-1.,0.0732830357306724));
#23485=CARTESIAN_POINT('Ctrl Pts',(-2.19552129484002,-1.,0.0713863779526153));
#23486=CARTESIAN_POINT('Ctrl Pts',(-2.19777582085423,-1.,0.0701143536325489));
#23487=CARTESIAN_POINT('Ctrl Pts',(-2.19890268624765,-1.,0.069476445021958));
#23488=CARTESIAN_POINT('',(-2.19890268624765,-1.,-0.0694764450219585));
#23489=CARTESIAN_POINT('',(-2.19890268624765,-1.,0.069476445021958));
#23490=CARTESIAN_POINT('',(-1.74236521665491,-1.,-0.163289472382896));
#23491=CARTESIAN_POINT('Ctrl Pts',(-2.19890268624765,-1.,-0.0694764450219585));
#23492=CARTESIAN_POINT('Ctrl Pts',(-2.19777582085261,-1.,-0.0701143536324927));
#23493=CARTESIAN_POINT('Ctrl Pts',(-2.19552129483562,-1.,-0.0713863779524629));
#23494=CARTESIAN_POINT('Ctrl Pts',(-2.19213712012956,-1.,-0.0732830357304277));
#23495=CARTESIAN_POINT('Ctrl Pts',(-2.1876201139874,-1.,-0.0757891465833413));
#23496=CARTESIAN_POINT('Ctrl Pts',(-2.18196589448304,-1.,-0.0788837727683229));
#23497=CARTESIAN_POINT('Ctrl Pts',(-2.1763037121106,-1.,-0.0819402680871941));
#23498=CARTESIAN_POINT('Ctrl Pts',(-2.17063357871031,-1.,-0.0849584620835644));
#23499=CARTESIAN_POINT('Ctrl Pts',(-2.16495552645275,-1.,-0.0879381291387824));
#23500=CARTESIAN_POINT('Ctrl Pts',(-2.15926961544808,-1.,-0.0908789888108267));
#23501=CARTESIAN_POINT('Ctrl Pts',(-2.15357593978377,-1.,-0.0937807218868346));
#23502=CARTESIAN_POINT('Ctrl Pts',(-2.14787463531864,-1.,-0.096642985230569));
#23503=CARTESIAN_POINT('Ctrl Pts',(-2.14216588395974,-1.,-0.0994654261990744));
#23504=CARTESIAN_POINT('Ctrl Pts',(-2.13644992667052,-1.,-0.102247700556064));
#23505=CARTESIAN_POINT('Ctrl Pts',(-2.1307270488718,-1.,-0.104989479152703));
#23506=CARTESIAN_POINT('Ctrl Pts',(-2.12499752306927,-1.,-0.107690435231068));
#23507=CARTESIAN_POINT('Ctrl Pts',(-2.11926155590849,-1.,-0.11035023613502));
#23508=CARTESIAN_POINT('Ctrl Pts',(-2.11351924490335,-1.,-0.112968534419746));
#23509=CARTESIAN_POINT('Ctrl Pts',(-2.10777050261359,-1.,-0.11554495768794));
#23510=CARTESIAN_POINT('Ctrl Pts',(-2.10201512132945,-1.,-0.118079107988368));
#23511=CARTESIAN_POINT('Ctrl Pts',(-2.09625292867756,-1.,-0.120570567965129));
#23512=CARTESIAN_POINT('Ctrl Pts',(-2.09048392424826,-1.,-0.123018905621083));
#23513=CARTESIAN_POINT('Ctrl Pts',(-2.08470840653628,-1.,-0.125423679412058));
#23514=CARTESIAN_POINT('Ctrl Pts',(-2.07892715110967,-1.,-0.127784445276116));
#23515=CARTESIAN_POINT('Ctrl Pts',(-2.07314114713047,-1.,-0.130100748328401));
#23516=CARTESIAN_POINT('Ctrl Pts',(-2.06735123910319,-1.,-0.13237211154771));
#23517=CARTESIAN_POINT('Ctrl Pts',(-2.06155781517844,-1.,-0.134598026192107));
#23518=CARTESIAN_POINT('Ctrl Pts',(-2.0557604441427,-1.,-0.136777941218044));
#23519=CARTESIAN_POINT('Ctrl Pts',(-2.04995762001333,-1.,-0.138911255368966));
#23520=CARTESIAN_POINT('Ctrl Pts',(-2.04414757947919,-1.,-0.140997332152545));
#23521=CARTESIAN_POINT('Ctrl Pts',(-2.03832911025913,-1.,-0.143035515058208));
#23522=CARTESIAN_POINT('Ctrl Pts',(-2.03250223739941,-1.,-0.145025140186058));
#23523=CARTESIAN_POINT('Ctrl Pts',(-2.02666926182017,-1.,-0.146965557332586));
#23524=CARTESIAN_POINT('Ctrl Pts',(-2.02083464969897,-1.,-0.148856124775343));
#23525=CARTESIAN_POINT('Ctrl Pts',(-2.01500291940243,-1.,-0.150696157673084));
#23526=CARTESIAN_POINT('Ctrl Pts',(-2.00917680318426,-1.,-0.152484883621452));
#23527=CARTESIAN_POINT('Ctrl Pts',(-2.00335565310539,-1.,-0.154221403049719));
#23528=CARTESIAN_POINT('Ctrl Pts',(-1.99753284771487,-1.,-0.155904629548775));
#23529=CARTESIAN_POINT('Ctrl Pts',(-1.99169810931893,-1.,-0.157533331459215));
#23530=CARTESIAN_POINT('Ctrl Pts',(-1.98584238283279,-1.,-0.159106226437289));
#23531=CARTESIAN_POINT('Ctrl Pts',(-1.97996195437557,-1.,-0.16062206078461));
#23532=CARTESIAN_POINT('Ctrl Pts',(-1.97406280235204,-1.,-0.162079693556302));
#23533=CARTESIAN_POINT('Ctrl Pts',(-1.96816512678,-1.,-0.16347818545776));
#23534=CARTESIAN_POINT('Ctrl Pts',(-1.96229379940174,-1.,-0.1648165689203));
#23535=CARTESIAN_POINT('Ctrl Pts',(-1.95646759718755,-1.,-0.166093592002833));
#23536=CARTESIAN_POINT('Ctrl Pts',(-1.95069027794286,-1.,-0.167307501784469));
#23537=CARTESIAN_POINT('Ctrl Pts',(-1.94493757756879,-1.,-0.168455741607516));
#23538=CARTESIAN_POINT('Ctrl Pts',(-1.93915639211497,-1.,-0.169534904817425));
#23539=CARTESIAN_POINT('Ctrl Pts',(-1.93329183155455,-1.,-0.170541253116136));
#23540=CARTESIAN_POINT('Ctrl Pts',(-1.92731093582,-1.,-0.17147119153296));
#23541=CARTESIAN_POINT('Ctrl Pts',(-1.92122334398034,-1.,-0.172321621259557));
#23542=CARTESIAN_POINT('Ctrl Pts',(-1.91511429159681,-1.,-0.173090695383619));
#23543=CARTESIAN_POINT('Ctrl Pts',(-1.90911693975475,-1.,-0.173776635257984));
#23544=CARTESIAN_POINT('Ctrl Pts',(-1.90335253863003,-1.,-0.174375518661222));
#23545=CARTESIAN_POINT('Ctrl Pts',(-1.89788101117148,-1.,-0.174879405091277));
#23546=CARTESIAN_POINT('Ctrl Pts',(-1.89264630198279,-1.,-0.175274276190664));
#23547=CARTESIAN_POINT('Ctrl Pts',(-1.88742606272818,-1.,-0.175538155840286));
#23548=CARTESIAN_POINT('Ctrl Pts',(-1.88188663144846,-1.,-0.175644148889271));
#23549=CARTESIAN_POINT('Ctrl Pts',(-1.87563767773249,-1.,-0.175563480746205));
#23550=CARTESIAN_POINT('Ctrl Pts',(-1.86828349694972,-1.,-0.175268337590901));
#23551=CARTESIAN_POINT('Ctrl Pts',(-1.85948367089838,-1.,-0.174735259276856));
#23552=CARTESIAN_POINT('Ctrl Pts',(-1.84898113200543,-1.,-0.173946627589401));
#23553=CARTESIAN_POINT('Ctrl Pts',(-1.83658380530747,-1.,-0.17288944289442));
#23554=CARTESIAN_POINT('Ctrl Pts',(-1.82215766815414,-1.,-0.171554770207306));
#23555=CARTESIAN_POINT('Ctrl Pts',(-1.80561530633924,-1.,-0.169936923908078));
#23556=CARTESIAN_POINT('Ctrl Pts',(-1.78690649988931,-1.,-0.16803277280837));
#23557=CARTESIAN_POINT('Ctrl Pts',(-1.77018771687692,-1.,-0.166279355148738));
#23558=CARTESIAN_POINT('Ctrl Pts',(-1.75666056640041,-1.,-0.164834765708484));
#23559=CARTESIAN_POINT('Ctrl Pts',(-1.74720349503904,-1.,-0.163814161002474));
#23560=CARTESIAN_POINT('Ctrl Pts',(-1.74236521665491,-1.,-0.163289472382896));
#23561=CARTESIAN_POINT('',(-1.7075470150345,-1.,-0.383122945602004));
#23562=CARTESIAN_POINT('Origin',(0.,-1.,0.));
#23563=CARTESIAN_POINT('',(-2.11275013067528,-1.,-0.61342227326009));
#23564=CARTESIAN_POINT('Ctrl Pts',(-1.7075470150345,-1.,-0.383122945602004));
#23565=CARTESIAN_POINT('Ctrl Pts',(-1.71231062891398,-1.,-0.384119047314215));
#23566=CARTESIAN_POINT('Ctrl Pts',(-1.72162022244582,-1.,-0.386070790323281));
#23567=CARTESIAN_POINT('Ctrl Pts',(-1.73493170972829,-1.,-0.388877023502615));
#23568=CARTESIAN_POINT('Ctrl Pts',(-1.75137405310193,-1.,-0.392375812285395));
#23569=CARTESIAN_POINT('Ctrl Pts',(-1.76975560043442,-1.,-0.396346196110688));
#23570=CARTESIAN_POINT('Ctrl Pts',(-1.78598826343754,-1.,-0.399919403774155));
#23571=CARTESIAN_POINT('Ctrl Pts',(-1.80012077173238,-1.,-0.403107976163396));
#23572=CARTESIAN_POINT('Ctrl Pts',(-1.81223801812013,-1.,-0.405933518407175));
#23573=CARTESIAN_POINT('Ctrl Pts',(-1.82247022677562,-1.,-0.408428948106227));
#23574=CARTESIAN_POINT('Ctrl Pts',(-1.83100408895047,-1.,-0.410641256301276));
#23575=CARTESIAN_POINT('Ctrl Pts',(-1.8380895347617,-1.,-0.412633125322945));
#23576=CARTESIAN_POINT('Ctrl Pts',(-1.84405757074218,-1.,-0.414487438255542));
#23577=CARTESIAN_POINT('Ctrl Pts',(-1.84929312930314,-1.,-0.416300022039885));
#23578=CARTESIAN_POINT('Ctrl Pts',(-1.8541763285645,-1.,-0.418164129144045));
#23579=CARTESIAN_POINT('Ctrl Pts',(-1.8590328109667,-1.,-0.420157287975583));
#23580=CARTESIAN_POINT('Ctrl Pts',(-1.86408083333863,-1.,-0.422327307417884));
#23581=CARTESIAN_POINT('Ctrl Pts',(-1.8693780394412,-1.,-0.424678177290876));
#23582=CARTESIAN_POINT('Ctrl Pts',(-1.87486989291333,-1.,-0.427183828518743));
#23583=CARTESIAN_POINT('Ctrl Pts',(-1.88044229001778,-1.,-0.429803062482217));
#23584=CARTESIAN_POINT('Ctrl Pts',(-1.88596913666828,-1.,-0.432493038548833));
#23585=CARTESIAN_POINT('Ctrl Pts',(-1.89136993975585,-1.,-0.43522566096358));
#23586=CARTESIAN_POINT('Ctrl Pts',(-1.89663648956549,-1.,-0.437995003948443));
#23587=CARTESIAN_POINT('Ctrl Pts',(-1.90180124389137,-1.,-0.44080783370416));
#23588=CARTESIAN_POINT('Ctrl Pts',(-1.90691756144906,-1.,-0.44367755684917));
#23589=CARTESIAN_POINT('Ctrl Pts',(-1.91203699981095,-1.,-0.446617343485651));
#23590=CARTESIAN_POINT('Ctrl Pts',(-1.91718342555717,-1.,-0.449632260106572));
#23591=CARTESIAN_POINT('Ctrl Pts',(-1.9223538064847,-1.,-0.452719478359356));
#23592=CARTESIAN_POINT('Ctrl Pts',(-1.92753067150461,-1.,-0.455872005174335));
#23593=CARTESIAN_POINT('Ctrl Pts',(-1.93269066517936,-1.,-0.459081234547931));
#23594=CARTESIAN_POINT('Ctrl Pts',(-1.93781486640834,-1.,-0.462340031009087));
#23595=CARTESIAN_POINT('Ctrl Pts',(-1.94289794196205,-1.,-0.465645462026064));
#23596=CARTESIAN_POINT('Ctrl Pts',(-1.94794381136524,-1.,-0.468997482913158));
#23597=CARTESIAN_POINT('Ctrl Pts',(-1.95296148278136,-1.,-0.472397672264079));
#23598=CARTESIAN_POINT('Ctrl Pts',(-1.95796111148175,-1.,-0.475848034683171));
#23599=CARTESIAN_POINT('Ctrl Pts',(-1.96294933055938,-1.,-0.479349583074846));
#23600=CARTESIAN_POINT('Ctrl Pts',(-1.96792703422358,-1.,-0.482901662120686));
#23601=CARTESIAN_POINT('Ctrl Pts',(-1.97289186263272,-1.,-0.486502692907661));
#23602=CARTESIAN_POINT('Ctrl Pts',(-1.97783973019229,-1.,-0.490150627860955));
#23603=CARTESIAN_POINT('Ctrl Pts',(-1.9827665876182,-1.,-0.493843476541492));
#23604=CARTESIAN_POINT('Ctrl Pts',(-1.98767044752929,-1.,-0.497579909545564));
#23605=CARTESIAN_POINT('Ctrl Pts',(-1.9925514912615,-1.,-0.501359287727129));
#23606=CARTESIAN_POINT('Ctrl Pts',(-1.99741107463567,-1.,-0.505181361323011));
#23607=CARTESIAN_POINT('Ctrl Pts',(-2.00225107134733,-1.,-0.509046069886152));
#23608=CARTESIAN_POINT('Ctrl Pts',(-2.00707309946955,-1.,-0.512953306961813));
#23609=CARTESIAN_POINT('Ctrl Pts',(-2.01187773939257,-1.,-0.516902681728733));
#23610=CARTESIAN_POINT('Ctrl Pts',(-2.01666477917305,-1.,-0.520893590399428));
#23611=CARTESIAN_POINT('Ctrl Pts',(-2.02143356304712,-1.,-0.524925318333518));
#23612=CARTESIAN_POINT('Ctrl Pts',(-2.02618329083289,-1.,-0.52899712724191));
#23613=CARTESIAN_POINT('Ctrl Pts',(-2.03091336214401,-1.,-0.533108355132905));
#23614=CARTESIAN_POINT('Ctrl Pts',(-2.03562362953993,-1.,-0.537258489833134));
#23615=CARTESIAN_POINT('Ctrl Pts',(-2.0403142269048,-1.,-0.54144712061552));
#23616=CARTESIAN_POINT('Ctrl Pts',(-2.0449854471456,-1.,-0.545673903817348));
#23617=CARTESIAN_POINT('Ctrl Pts',(-2.04963761077974,-1.,-0.549938525150342));
#23618=CARTESIAN_POINT('Ctrl Pts',(-2.05427091604482,-1.,-0.554240657464109));
#23619=CARTESIAN_POINT('Ctrl Pts',(-2.05888537756571,-1.,-0.558579940185467));
#23620=CARTESIAN_POINT('Ctrl Pts',(-2.06348090160697,-1.,-0.562955993082574));
#23621=CARTESIAN_POINT('Ctrl Pts',(-2.06805732997383,-1.,-0.567368421181229));
#23622=CARTESIAN_POINT('Ctrl Pts',(-2.07261449292757,-1.,-0.571816823242411));
#23623=CARTESIAN_POINT('Ctrl Pts',(-2.07715226767361,-1.,-0.576300797416274));
#23624=CARTESIAN_POINT('Ctrl Pts',(-2.08167059018138,-1.,-0.580819952107257));
#23625=CARTESIAN_POINT('Ctrl Pts',(-2.086169437277,-1.,-0.585373918990895));
#23626=CARTESIAN_POINT('Ctrl Pts',(-2.09064881812053,-1.,-0.589962365403189));
#23627=CARTESIAN_POINT('Ctrl Pts',(-2.09510876220501,-1.,-0.594585006052823));
#23628=CARTESIAN_POINT('Ctrl Pts',(-2.09954930865331,-1.,-0.599241616422144));
#23629=CARTESIAN_POINT('Ctrl Pts',(-2.10397049887709,-1.,-0.603932030738212));
#23630=CARTESIAN_POINT('Ctrl Pts',(-2.10749199615859,-1.,-0.607711315456826));
#23631=CARTESIAN_POINT('Ctrl Pts',(-2.11012443807661,-1.,-0.610560911691113));
#23632=CARTESIAN_POINT('Ctrl Pts',(-2.11187554260142,-1.,-0.61246736556225));
#23633=CARTESIAN_POINT('Ctrl Pts',(-2.11275013067528,-1.,-0.61342227326009));
#23634=CARTESIAN_POINT('',(-2.0698113262342,-1.,-0.745574324794401));
#23635=CARTESIAN_POINT('',(-2.11275013067528,-1.,-0.61342227326009));
#23636=CARTESIAN_POINT('',(-1.60662857109684,-1.,-0.693717979106306));
#23637=CARTESIAN_POINT('Ctrl Pts',(-2.0698113262342,-1.,-0.745574324794401));
#23638=CARTESIAN_POINT('Ctrl Pts',(-2.06854248895575,-1.,-0.74583279137781));
#23639=CARTESIAN_POINT('Ctrl Pts',(-2.06600523016401,-1.,-0.746345871542695));
#23640=CARTESIAN_POINT('Ctrl Pts',(-2.06220058927162,-1.,-0.747103932785504));
#23641=CARTESIAN_POINT('Ctrl Pts',(-2.05713023030263,-1.,-0.748091554181101));
#23642=CARTESIAN_POINT('Ctrl Pts',(-2.05079645591606,-1.,-0.749287468663053));
#23643=CARTESIAN_POINT('Ctrl Pts',(-2.04446689147754,-1.,-0.750444657874758));
#23644=CARTESIAN_POINT('Ctrl Pts',(-2.03814160092173,-1.,-0.751562963361383));
#23645=CARTESIAN_POINT('Ctrl Pts',(-2.03182068456467,-1.,-0.752642180488104));
#23646=CARTESIAN_POINT('Ctrl Pts',(-2.02550428623587,-1.,-0.753682061113765));
#23647=CARTESIAN_POINT('Ctrl Pts',(-2.01919259406003,-1.,-0.75468233072352));
#23648=CARTESIAN_POINT('Ctrl Pts',(-2.01288584328149,-1.,-0.7556427049581));
#23649=CARTESIAN_POINT('Ctrl Pts',(-2.00658431587682,-1.,-0.756562904646496));
#23650=CARTESIAN_POINT('Ctrl Pts',(-2.00028834739072,-1.,-0.757442676862341));
#23651=CARTESIAN_POINT('Ctrl Pts',(-1.9939983109871,-1.,-0.758281796766377));
#23652=CARTESIAN_POINT('Ctrl Pts',(-1.98771456680806,-1.,-0.759080037802242));
#23653=CARTESIAN_POINT('Ctrl Pts',(-1.98143741418156,-1.,-0.759837147452135));
#23654=CARTESIAN_POINT('Ctrl Pts',(-1.97516705321521,-1.,-0.760552825409855));
#23655=CARTESIAN_POINT('Ctrl Pts',(-1.96890351582545,-1.,-0.761226690483986));
#23656=CARTESIAN_POINT('Ctrl Pts',(-1.96264672744229,-1.,-0.761858300014575));
#23657=CARTESIAN_POINT('Ctrl Pts',(-1.95639665309893,-1.,-0.762447203806263));
#23658=CARTESIAN_POINT('Ctrl Pts',(-1.95015342590025,-1.,-0.762992990878774));
#23659=CARTESIAN_POINT('Ctrl Pts',(-1.94391746617626,-1.,-0.76349533353858));
#23660=CARTESIAN_POINT('Ctrl Pts',(-1.93768964875867,-1.,-0.763954049121393));
#23661=CARTESIAN_POINT('Ctrl Pts',(-1.93147105496367,-1.,-0.764369010673889));
#23662=CARTESIAN_POINT('Ctrl Pts',(-1.92526263537041,-1.,-0.764740025488189));
#23663=CARTESIAN_POINT('Ctrl Pts',(-1.91906491634197,-1.,-0.765066729667095));
#23664=CARTESIAN_POINT('Ctrl Pts',(-1.91287765805174,-1.,-0.765348465884739));
#23665=CARTESIAN_POINT('Ctrl Pts',(-1.90669961402362,-1.,-0.765584196937936));
#23666=CARTESIAN_POINT('Ctrl Pts',(-1.90052930393599,-1.,-0.765772772593395));
#23667=CARTESIAN_POINT('Ctrl Pts',(-1.89436577771389,-1.,-0.765913193856979));
#23668=CARTESIAN_POINT('Ctrl Pts',(-1.88820926433409,-1.,-0.76600483706209));
#23669=CARTESIAN_POINT('Ctrl Pts',(-1.88206215302561,-1.,-0.766047794851868));
#23670=CARTESIAN_POINT('Ctrl Pts',(-1.87592888967886,-1.,-0.766042837036759));
#23671=CARTESIAN_POINT('Ctrl Pts',(-1.86981398314345,-1.,-0.765990708546111));
#23672=CARTESIAN_POINT('Ctrl Pts',(-1.86372027063314,-1.,-0.765891519092557));
#23673=CARTESIAN_POINT('Ctrl Pts',(-1.85764741390391,-1.,-0.765744212909305));
#23674=CARTESIAN_POINT('Ctrl Pts',(-1.85158945130054,-1.,-0.765545710619023));
#23675=CARTESIAN_POINT('Ctrl Pts',(-1.8455369887591,-1.,-0.765291664861971));
#23676=CARTESIAN_POINT('Ctrl Pts',(-1.83948181064823,-1.,-0.764978057881687));
#23677=CARTESIAN_POINT('Ctrl Pts',(-1.8334207722714,-1.,-0.764602549687845));
#23678=CARTESIAN_POINT('Ctrl Pts',(-1.8273599120008,-1.,-0.764165902606055));
#23679=CARTESIAN_POINT('Ctrl Pts',(-1.82131873145297,-1.,-0.763673465462854));
#23680=CARTESIAN_POINT('Ctrl Pts',(-1.81532118405566,-1.,-0.763132003836783));
#23681=CARTESIAN_POINT('Ctrl Pts',(-1.80938551463989,-1.,-0.762546129464036));
#23682=CARTESIAN_POINT('Ctrl Pts',(-1.80351583877334,-1.,-0.761915336443515));
#23683=CARTESIAN_POINT('Ctrl Pts',(-1.79768986997735,-1.,-0.761229695230359));
#23684=CARTESIAN_POINT('Ctrl Pts',(-1.79185815610802,-1.,-0.760469555880425));
#23685=CARTESIAN_POINT('Ctrl Pts',(-1.78596964884526,-1.,-0.759614401109868));
#23686=CARTESIAN_POINT('Ctrl Pts',(-1.77999411220912,-1.,-0.75865062667738));
#23687=CARTESIAN_POINT('Ctrl Pts',(-1.77394167108342,-1.,-0.757578264077238));
#23688=CARTESIAN_POINT('Ctrl Pts',(-1.76789396003141,-1.,-0.756421896028403));
#23689=CARTESIAN_POINT('Ctrl Pts',(-1.7619781724032,-1.,-0.755220979975262));
#23690=CARTESIAN_POINT('Ctrl Pts',(-1.75631083600175,-1.,-0.75400925402848));
#23691=CARTESIAN_POINT('Ctrl Pts',(-1.75095139468809,-1.,-0.752797683531377));
#23692=CARTESIAN_POINT('Ctrl Pts',(-1.74585086852298,-1.,-0.751555614163629));
#23693=CARTESIAN_POINT('Ctrl Pts',(-1.74080458266705,-1.,-0.75019343597954));
#23694=CARTESIAN_POINT('Ctrl Pts',(-1.73550351679848,-1.,-0.748582462954854));
#23695=CARTESIAN_POINT('Ctrl Pts',(-1.72958533647399,-1.,-0.746574710096436));
#23696=CARTESIAN_POINT('Ctrl Pts',(-1.7226822991693,-1.,-0.744021445433764));
#23697=CARTESIAN_POINT('Ctrl Pts',(-1.71447789751927,-1.,-0.740795162032087));
#23698=CARTESIAN_POINT('Ctrl Pts',(-1.70473309006121,-1.,-0.736799665724771));
#23699=CARTESIAN_POINT('Ctrl Pts',(-1.69326921975743,-1.,-0.731963238697195));
#23700=CARTESIAN_POINT('Ctrl Pts',(-1.67996158455503,-1.,-0.726235967997433));
#23701=CARTESIAN_POINT('Ctrl Pts',(-1.6647288055568,-1.,-0.719585433804282));
#23702=CARTESIAN_POINT('Ctrl Pts',(-1.64752408832016,-1.,-0.711993139355394));
#23703=CARTESIAN_POINT('Ctrl Pts',(-1.63216541664676,-1.,-0.705159151988319));
#23704=CARTESIAN_POINT('Ctrl Pts',(-1.61974673472612,-1.,-0.699605146405088));
#23705=CARTESIAN_POINT('Ctrl Pts',(-1.61106790958151,-1.,-0.695712097881194));
#23706=CARTESIAN_POINT('Ctrl Pts',(-1.60662857109684,-1.,-0.693717979106306));
#23707=CARTESIAN_POINT('',(-1.5055822144029,-1.,-0.892032620296855));
#23708=CARTESIAN_POINT('Origin',(0.,-1.,0.));
#23709=CARTESIAN_POINT('',(-1.81978687191668,-1.,-1.23627494547115));
#23710=CARTESIAN_POINT('Ctrl Pts',(-1.5055822144029,-1.,-0.892032620296855));
#23711=CARTESIAN_POINT('Ctrl Pts',(-1.50980486806688,-1.,-0.894452006964543));
#23712=CARTESIAN_POINT('Ctrl Pts',(-1.51805569590094,-1.,-0.899185047483511));
#23713=CARTESIAN_POINT('Ctrl Pts',(-1.52984849887993,-1.,-0.905967409625651));
#23714=CARTESIAN_POINT('Ctrl Pts',(-1.54440491149498,-1.,-0.914375919026456));
#23715=CARTESIAN_POINT('Ctrl Pts',(-1.56065988578893,-1.,-0.923832188944341));
#23716=CARTESIAN_POINT('Ctrl Pts',(-1.57499388382243,-1.,-0.932246680108685));
#23717=CARTESIAN_POINT('Ctrl Pts',(-1.58744937487176,-1.,-0.939646377893399));
#23718=CARTESIAN_POINT('Ctrl Pts',(-1.59810042043673,-1.,-0.946078063315257));
#23719=CARTESIAN_POINT('Ctrl Pts',(-1.60706069896936,-1.,-0.951613284356035));
#23720=CARTESIAN_POINT('Ctrl Pts',(-1.61449324337085,-1.,-0.956354422920671));
#23721=CARTESIAN_POINT('Ctrl Pts',(-1.62061638140221,-1.,-0.960438326101729));
#23722=CARTESIAN_POINT('Ctrl Pts',(-1.62571930670187,-1.,-0.964046107040536));
#23723=CARTESIAN_POINT('Ctrl Pts',(-1.63013849959461,-1.,-0.967387853230345));
#23724=CARTESIAN_POINT('Ctrl Pts',(-1.63420665729798,-1.,-0.970669715997509));
#23725=CARTESIAN_POINT('Ctrl Pts',(-1.63820952658144,-1.,-0.974066058287418));
#23726=CARTESIAN_POINT('Ctrl Pts',(-1.64233990826687,-1.,-0.977689794119416));
#23727=CARTESIAN_POINT('Ctrl Pts',(-1.64665139190656,-1.,-0.981562530939489));
#23728=CARTESIAN_POINT('Ctrl Pts',(-1.65110016612638,-1.,-0.985642622920821));
#23729=CARTESIAN_POINT('Ctrl Pts',(-1.65559044289699,-1.,-0.989855627854165));
#23730=CARTESIAN_POINT('Ctrl Pts',(-1.66001553809947,-1.,-0.994121836661306));
#23731=CARTESIAN_POINT('Ctrl Pts',(-1.66430758030376,-1.,-0.998389654952758));
#23732=CARTESIAN_POINT('Ctrl Pts',(-1.66846059277303,-1.,-1.00265091003727));
#23733=CARTESIAN_POINT('Ctrl Pts',(-1.67250335383293,-1.,-1.00692206696414));
#23734=CARTESIAN_POINT('Ctrl Pts',(-1.67648246776464,-1.,-1.01123236493511));
#23735=CARTESIAN_POINT('Ctrl Pts',(-1.68044289894798,-1.,-1.01561026162773));
#23736=CARTESIAN_POINT('Ctrl Pts',(-1.68440578021706,-1.,-1.02006795074201));
#23737=CARTESIAN_POINT('Ctrl Pts',(-1.68836910178447,-1.,-1.02460180535255));
#23738=CARTESIAN_POINT('Ctrl Pts',(-1.69231840863458,-1.,-1.02919977579147));
#23739=CARTESIAN_POINT('Ctrl Pts',(-1.69623414782771,-1.,-1.03384646003588));
#23740=CARTESIAN_POINT('Ctrl Pts',(-1.70010052930962,-1.,-1.03852922490789));
#23741=CARTESIAN_POINT('Ctrl Pts',(-1.70391338707982,-1.,-1.04324363334554));
#23742=CARTESIAN_POINT('Ctrl Pts',(-1.70767646263649,-1.,-1.04799085404995));
#23743=CARTESIAN_POINT('Ctrl Pts',(-1.71139783543989,-1.,-1.05277517202855));
#23744=CARTESIAN_POINT('Ctrl Pts',(-1.7150865442702,-1.,-1.05760163192479));
#23745=CARTESIAN_POINT('Ctrl Pts',(-1.71874858456904,-1.,-1.06247324680647));
#23746=CARTESIAN_POINT('Ctrl Pts',(-1.72238500928453,-1.,-1.06738966975462));
#23747=CARTESIAN_POINT('Ctrl Pts',(-1.72599406198488,-1.,-1.07234866990252));
#23748=CARTESIAN_POINT('Ctrl Pts',(-1.72957248977424,-1.,-1.0773470373727));
#23749=CARTESIAN_POINT('Ctrl Pts',(-1.73311705663407,-1.,-1.08238162784749));
#23750=CARTESIAN_POINT('Ctrl Pts',(-1.73662628326091,-1.,-1.08745056285427));
#23751=CARTESIAN_POINT('Ctrl Pts',(-1.74010053962247,-1.,-1.09255329056493));
#23752=CARTESIAN_POINT('Ctrl Pts',(-1.74354119236208,-1.,-1.09768999241225));
#23753=CARTESIAN_POINT('Ctrl Pts',(-1.74695004214923,-1.,-1.10286118991143));
#23754=CARTESIAN_POINT('Ctrl Pts',(-1.7503286607592,-1.,-1.10806728183007));
#23755=CARTESIAN_POINT('Ctrl Pts',(-1.7536777209463,-1.,-1.11330807582551));
#23756=CARTESIAN_POINT('Ctrl Pts',(-1.75699720772105,-1.,-1.11858293216763));
#23757=CARTESIAN_POINT('Ctrl Pts',(-1.76028671825096,-1.,-1.12389096855086));
#23758=CARTESIAN_POINT('Ctrl Pts',(-1.7635457196617,-1.,-1.12923123555075));
#23759=CARTESIAN_POINT('Ctrl Pts',(-1.76677384551862,-1.,-1.1346029180462));
#23760=CARTESIAN_POINT('Ctrl Pts',(-1.76997111386769,-1.,-1.14000548336975));
#23761=CARTESIAN_POINT('Ctrl Pts',(-1.77313777896194,-1.,-1.1454385822692));
#23762=CARTESIAN_POINT('Ctrl Pts',(-1.7762742255701,-1.,-1.15090197841515));
#23763=CARTESIAN_POINT('Ctrl Pts',(-1.77938085564275,-1.,-1.15639547194698));
#23764=CARTESIAN_POINT('Ctrl Pts',(-1.78245795881009,-1.,-1.16191881298499));
#23765=CARTESIAN_POINT('Ctrl Pts',(-1.78550566040443,-1.,-1.16747166312303));
#23766=CARTESIAN_POINT('Ctrl Pts',(-1.78852398877616,-1.,-1.17305363177328));
#23767=CARTESIAN_POINT('Ctrl Pts',(-1.79151291552689,-1.,-1.17866429440809));
#23768=CARTESIAN_POINT('Ctrl Pts',(-1.79447240321515,-1.,-1.18430321697432));
#23769=CARTESIAN_POINT('Ctrl Pts',(-1.79740245923478,-1.,-1.18996997934445));
#23770=CARTESIAN_POINT('Ctrl Pts',(-1.80030314369879,-1.,-1.19566418930242));
#23771=CARTESIAN_POINT('Ctrl Pts',(-1.80317454838603,-1.,-1.20138548938974));
#23772=CARTESIAN_POINT('Ctrl Pts',(-1.80601678480707,-1.,-1.20713356605475));
#23773=CARTESIAN_POINT('Ctrl Pts',(-1.80882996917129,-1.,-1.21290815708314));
#23774=CARTESIAN_POINT('Ctrl Pts',(-1.81161420806656,-1.,-1.21870906103557));
#23775=CARTESIAN_POINT('Ctrl Pts',(-1.81436959210434,-1.,-1.2245361330495));
#23776=CARTESIAN_POINT('Ctrl Pts',(-1.8165508718364,-1.,-1.2292186489137));
#23777=CARTESIAN_POINT('Ctrl Pts',(-1.81817389921279,-1.,-1.2327422452705));
#23778=CARTESIAN_POINT('Ctrl Pts',(-1.81925017193666,-1.,-1.23509651170476));
#23779=CARTESIAN_POINT('Ctrl Pts',(-1.81978687191668,-1.,-1.23627494547115));
#23780=CARTESIAN_POINT('',(-1.73811241238545,-1.,-1.34869019493419));
#23781=CARTESIAN_POINT('',(-1.81978687191668,-1.,-1.23627494547115));
#23782=CARTESIAN_POINT('',(-1.31362392696032,-1.,-1.15624053661742));
#23783=CARTESIAN_POINT('Ctrl Pts',(-1.73811241238545,-1.,-1.34869019493419));
#23784=CARTESIAN_POINT('Ctrl Pts',(-1.73682580585691,-1.,-1.34854391898045));
#23785=CARTESIAN_POINT('Ctrl Pts',(-1.73425417885907,-1.,-1.34824783112887));
#23786=CARTESIAN_POINT('Ctrl Pts',(-1.7304014965394,-1.,-1.34779309152035));
#23787=CARTESIAN_POINT('Ctrl Pts',(-1.72527410680674,-1.,-1.34716554819527));
#23788=CARTESIAN_POINT('Ctrl Pts',(-1.7188807715049,-1.,-1.34634568653227));
#23789=CARTESIAN_POINT('Ctrl Pts',(-1.71250340686822,-1.,-1.34549029589416));
#23790=CARTESIAN_POINT('Ctrl Pts',(-1.70614212266738,-1.,-1.34459924533831));
#23791=CARTESIAN_POINT('Ctrl Pts',(-1.69979707754427,-1.,-1.34367237124483));
#23792=CARTESIAN_POINT('Ctrl Pts',(-1.6934684849687,-1.,-1.34270948206319));
#23793=CARTESIAN_POINT('Ctrl Pts',(-1.68715660868764,-1.,-1.341710374848));
#23794=CARTESIAN_POINT('Ctrl Pts',(-1.68086176030362,-1.,-1.34067485185203));
#23795=CARTESIAN_POINT('Ctrl Pts',(-1.67458429426086,-1.,-1.3396027347034));
#23796=CARTESIAN_POINT('Ctrl Pts',(-1.66832460783989,-1.,-1.33849388654388));
#23797=CARTESIAN_POINT('Ctrl Pts',(-1.66208312541983,-1.,-1.33734820885262));
#23798=CARTESIAN_POINT('Ctrl Pts',(-1.65586025952593,-1.,-1.33616559745172));
#23799=CARTESIAN_POINT('Ctrl Pts',(-1.6496563728683,-1.,-1.33494590467993));
#23800=CARTESIAN_POINT('Ctrl Pts',(-1.6434717485603,-1.,-1.33368890676572));
#23801=CARTESIAN_POINT('Ctrl Pts',(-1.63730653475089,-1.,-1.33239425103724));
#23802=CARTESIAN_POINT('Ctrl Pts',(-1.63116079730923,-1.,-1.33106149345645));
#23803=CARTESIAN_POINT('Ctrl Pts',(-1.62503464209797,-1.,-1.3296901950568));
#23804=CARTESIAN_POINT('Ctrl Pts',(-1.61892832270724,-1.,-1.32828000610449));
#23805=CARTESIAN_POINT('Ctrl Pts',(-1.6128423401575,-1.,-1.32683074483356));
#23806=CARTESIAN_POINT('Ctrl Pts',(-1.60677758290954,-1.,-1.32534250785782));
#23807=CARTESIAN_POINT('Ctrl Pts',(-1.60073511858687,-1.,-1.32381550858256));
#23808=CARTESIAN_POINT('Ctrl Pts',(-1.59471591079403,-1.,-1.32224985747682));
#23809=CARTESIAN_POINT('Ctrl Pts',(-1.58872057258245,-1.,-1.32064537110892));
#23810=CARTESIAN_POINT('Ctrl Pts',(-1.58274907898834,-1.,-1.31900135021432));
#23811=CARTESIAN_POINT('Ctrl Pts',(-1.5768005650559,-1.,-1.31731642317187));
#23812=CARTESIAN_POINT('Ctrl Pts',(-1.57087397835723,-1.,-1.31558903860016));
#23813=CARTESIAN_POINT('Ctrl Pts',(-1.56496872402353,-1.,-1.31381795281002));
#23814=CARTESIAN_POINT('Ctrl Pts',(-1.55908521254821,-1.,-1.31200264341696));
#23815=CARTESIAN_POINT('Ctrl Pts',(-1.55322568759481,-1.,-1.31014393684222));
#23816=CARTESIAN_POINT('Ctrl Pts',(-1.54739413957185,-1.,-1.30824393907473));
#23817=CARTESIAN_POINT('Ctrl Pts',(-1.54159462645432,-1.,-1.30630475189556));
#23818=CARTESIAN_POINT('Ctrl Pts',(-1.53582981268977,-1.,-1.30432735639489));
#23819=CARTESIAN_POINT('Ctrl Pts',(-1.53009970283891,-1.,-1.30231064395568));
#23820=CARTESIAN_POINT('Ctrl Pts',(-1.52439957861062,-1.,-1.30024984366328));
#23821=CARTESIAN_POINT('Ctrl Pts',(-1.51872184912724,-1.,-1.29813791800747));
#23822=CARTESIAN_POINT('Ctrl Pts',(-1.51305994241402,-1.,-1.29596850710509));
#23823=CARTESIAN_POINT('Ctrl Pts',(-1.50741159078365,-1.,-1.29373841372842));
#23824=CARTESIAN_POINT('Ctrl Pts',(-1.50178230149776,-1.,-1.29145022885181));
#23825=CARTESIAN_POINT('Ctrl Pts',(-1.49618896881754,-1.,-1.28911506584254));
#23826=CARTESIAN_POINT('Ctrl Pts',(-1.4906522831278,-1.,-1.2867467611644));
#23827=CARTESIAN_POINT('Ctrl Pts',(-1.4851881711891,-1.,-1.28435533880201));
#23828=CARTESIAN_POINT('Ctrl Pts',(-1.47980070347095,-1.,-1.28194158939517));
#23829=CARTESIAN_POINT('Ctrl Pts',(-1.4744717526707,-1.,-1.2794891824849));
#23830=CARTESIAN_POINT('Ctrl Pts',(-1.46916035917133,-1.,-1.27696414831089));
#23831=CARTESIAN_POINT('Ctrl Pts',(-1.46382431332476,-1.,-1.27433119897822));
#23832=CARTESIAN_POINT('Ctrl Pts',(-1.45843906294697,-1.,-1.27156805265289));
#23833=CARTESIAN_POINT('Ctrl Pts',(-1.45301422764247,-1.,-1.2686778680489));
#23834=CARTESIAN_POINT('Ctrl Pts',(-1.44761985001662,-1.,-1.26570925118868));
#23835=CARTESIAN_POINT('Ctrl Pts',(-1.44236470511303,-1.,-1.26273903323859));
#23836=CARTESIAN_POINT('Ctrl Pts',(-1.43734919180848,-1.,-1.25983531012005));
#23837=CARTESIAN_POINT('Ctrl Pts',(-1.43262645609691,-1.,-1.25702687965755));
#23838=CARTESIAN_POINT('Ctrl Pts',(-1.42815938799387,-1.,-1.25426945222639));
#23839=CARTESIAN_POINT('Ctrl Pts',(-1.42378102115575,-1.,-1.2514145557001));
#23840=CARTESIAN_POINT('Ctrl Pts',(-1.41923722596025,-1.,-1.24824430986571));
#23841=CARTESIAN_POINT('Ctrl Pts',(-1.41422913175179,-1.,-1.24450600513056));
#23842=CARTESIAN_POINT('Ctrl Pts',(-1.40845295531283,-1.,-1.23994455029534));
#23843=CARTESIAN_POINT('Ctrl Pts',(-1.40164708206106,-1.,-1.23434087290423));
#23844=CARTESIAN_POINT('Ctrl Pts',(-1.39361389568796,-1.,-1.22752961899387));
#23845=CARTESIAN_POINT('Ctrl Pts',(-1.38420564527715,-1.,-1.21938737280852));
#23846=CARTESIAN_POINT('Ctrl Pts',(-1.37331915607905,-1.,-1.20982812925645));
#23847=CARTESIAN_POINT('Ctrl Pts',(-1.36088705043885,-1.,-1.1987959077932));
#23848=CARTESIAN_POINT('Ctrl Pts',(-1.34687054001093,-1.,-1.18625865667441));
#23849=CARTESIAN_POINT('Ctrl Pts',(-1.33437539347008,-1.,-1.17501305789857));
#23850=CARTESIAN_POINT('Ctrl Pts',(-1.32428080721772,-1.,-1.16589330093588));
#23851=CARTESIAN_POINT('Ctrl Pts',(-1.31722977216397,-1.,-1.15950888730809));
#23852=CARTESIAN_POINT('Ctrl Pts',(-1.31362392696032,-1.,-1.15624053661742));
#23853=CARTESIAN_POINT('',(-1.15624053661742,-1.,-1.31362392696033));
#23854=CARTESIAN_POINT('Origin',(0.,-1.,0.));
#23855=CARTESIAN_POINT('',(-1.34869019493419,-1.,-1.73811241238545));
#23856=CARTESIAN_POINT('Ctrl Pts',(-1.15624053661742,-1.,-1.31362392696033));
#23857=CARTESIAN_POINT('Ctrl Pts',(-1.15950888730433,-1.,-1.3172297721596));
#23858=CARTESIAN_POINT('Ctrl Pts',(-1.16589330092532,-1.,-1.32428080720544));
#23859=CARTESIAN_POINT('Ctrl Pts',(-1.17501305787994,-1.,-1.33437539344842));
#23860=CARTESIAN_POINT('Ctrl Pts',(-1.18625865664915,-1.,-1.34687053998157));
#23861=CARTESIAN_POINT('Ctrl Pts',(-1.1987959077656,-1.,-1.36088705040677));
#23862=CARTESIAN_POINT('Ctrl Pts',(-1.20982812923113,-1.,-1.37331915604962));
#23863=CARTESIAN_POINT('Ctrl Pts',(-1.21938737278853,-1.,-1.38420564525391));
#23864=CARTESIAN_POINT('Ctrl Pts',(-1.22752961898063,-1.,-1.39361389567257));
#23865=CARTESIAN_POINT('Ctrl Pts',(-1.23434087289768,-1.,-1.40164708205345));
#23866=CARTESIAN_POINT('Ctrl Pts',(-1.23994455029421,-1.,-1.40845295531151));
#23867=CARTESIAN_POINT('Ctrl Pts',(-1.24450600513278,-1.,-1.41422913175437));
#23868=CARTESIAN_POINT('Ctrl Pts',(-1.24824430986911,-1.,-1.41923722596421));
#23869=CARTESIAN_POINT('Ctrl Pts',(-1.25141455570299,-1.,-1.42378102115911));
#23870=CARTESIAN_POINT('Ctrl Pts',(-1.25426945222783,-1.,-1.42815938799555));
#23871=CARTESIAN_POINT('Ctrl Pts',(-1.25702687965744,-1.,-1.43262645609679));
#23872=CARTESIAN_POINT('Ctrl Pts',(-1.25983531011894,-1.,-1.43734919180719));
#23873=CARTESIAN_POINT('Ctrl Pts',(-1.26273903323723,-1.,-1.44236470511145));
#23874=CARTESIAN_POINT('Ctrl Pts',(-1.26570925118767,-1.,-1.44761985001544));
#23875=CARTESIAN_POINT('Ctrl Pts',(-1.26867786804854,-1.,-1.45301422764205));
#23876=CARTESIAN_POINT('Ctrl Pts',(-1.27156805265312,-1.,-1.45843906294725));
#23877=CARTESIAN_POINT('Ctrl Pts',(-1.27433119897877,-1.,-1.4638243133254));
#23878=CARTESIAN_POINT('Ctrl Pts',(-1.27696414831144,-1.,-1.46916035917197));
#23879=CARTESIAN_POINT('Ctrl Pts',(-1.27948918248524,-1.,-1.4744717526711));
#23880=CARTESIAN_POINT('Ctrl Pts',(-1.28194158939522,-1.,-1.47980070347102));
#23881=CARTESIAN_POINT('Ctrl Pts',(-1.28435533880184,-1.,-1.48518817118891));
#23882=CARTESIAN_POINT('Ctrl Pts',(-1.28674676116415,-1.,-1.4906522831275));
#23883=CARTESIAN_POINT('Ctrl Pts',(-1.28911506584232,-1.,-1.49618896881729));
#23884=CARTESIAN_POINT('Ctrl Pts',(-1.29145022885171,-1.,-1.50178230149764));
#23885=CARTESIAN_POINT('Ctrl Pts',(-1.29373841372843,-1.,-1.50741159078367));
#23886=CARTESIAN_POINT('Ctrl Pts',(-1.29596850710518,-1.,-1.51305994241412));
#23887=CARTESIAN_POINT('Ctrl Pts',(-1.29813791800757,-1.,-1.51872184912735));
#23888=CARTESIAN_POINT('Ctrl Pts',(-1.30024984366334,-1.,-1.5243995786107));
#23889=CARTESIAN_POINT('Ctrl Pts',(-1.3023106439557,-1.,-1.53009970283893));
#23890=CARTESIAN_POINT('Ctrl Pts',(-1.30432735639487,-1.,-1.53582981268976));
#23891=CARTESIAN_POINT('Ctrl Pts',(-1.30630475189553,-1.,-1.54159462645428));
#23892=CARTESIAN_POINT('Ctrl Pts',(-1.30824393907471,-1.,-1.54739413957183));
#23893=CARTESIAN_POINT('Ctrl Pts',(-1.31014393684221,-1.,-1.55322568759481));
#23894=CARTESIAN_POINT('Ctrl Pts',(-1.31200264341696,-1.,-1.55908521254822));
#23895=CARTESIAN_POINT('Ctrl Pts',(-1.31381795281002,-1.,-1.56496872402352));
#23896=CARTESIAN_POINT('Ctrl Pts',(-1.31558903860015,-1.,-1.57087397835721));
#23897=CARTESIAN_POINT('Ctrl Pts',(-1.31731642317183,-1.,-1.57680056505585));
#23898=CARTESIAN_POINT('Ctrl Pts',(-1.31900135021428,-1.,-1.58274907898829));
#23899=CARTESIAN_POINT('Ctrl Pts',(-1.32064537110891,-1.,-1.58872057258244));
#23900=CARTESIAN_POINT('Ctrl Pts',(-1.32224985747686,-1.,-1.59471591079408));
#23901=CARTESIAN_POINT('Ctrl Pts',(-1.32381550858266,-1.,-1.600735118587));
#23902=CARTESIAN_POINT('Ctrl Pts',(-1.32534250785794,-1.,-1.6067775829097));
#23903=CARTESIAN_POINT('Ctrl Pts',(-1.32683074483365,-1.,-1.61284234015762));
#23904=CARTESIAN_POINT('Ctrl Pts',(-1.32828000610448,-1.,-1.61892832270723));
#23905=CARTESIAN_POINT('Ctrl Pts',(-1.32969019505665,-1.,-1.62503464209777));
#23906=CARTESIAN_POINT('Ctrl Pts',(-1.33106149345618,-1.,-1.63116079730887));
#23907=CARTESIAN_POINT('Ctrl Pts',(-1.33239425103694,-1.,-1.6373065347505));
#23908=CARTESIAN_POINT('Ctrl Pts',(-1.33368890676554,-1.,-1.64347174856007));
#23909=CARTESIAN_POINT('Ctrl Pts',(-1.33494590468003,-1.,-1.64965637286843));
#23910=CARTESIAN_POINT('Ctrl Pts',(-1.33616559745217,-1.,-1.65586025952651));
#23911=CARTESIAN_POINT('Ctrl Pts',(-1.33734820885331,-1.,-1.66208312542073));
#23912=CARTESIAN_POINT('Ctrl Pts',(-1.33849388654458,-1.,-1.66832460784078));
#23913=CARTESIAN_POINT('Ctrl Pts',(-1.33960273470372,-1.,-1.67458429426126));
#23914=CARTESIAN_POINT('Ctrl Pts',(-1.3406748518516,-1.,-1.68086176030308));
#23915=CARTESIAN_POINT('Ctrl Pts',(-1.34171037484673,-1.,-1.68715660868602));
#23916=CARTESIAN_POINT('Ctrl Pts',(-1.34270948206139,-1.,-1.6934684849664));
#23917=CARTESIAN_POINT('Ctrl Pts',(-1.34367237124322,-1.,-1.69979707754221));
#23918=CARTESIAN_POINT('Ctrl Pts',(-1.34459924533783,-1.,-1.70614212266676));
#23919=CARTESIAN_POINT('Ctrl Pts',(-1.34549029589563,-1.,-1.71250340687011));
#23920=CARTESIAN_POINT('Ctrl Pts',(-1.34634568653586,-1.,-1.7188807715095));
#23921=CARTESIAN_POINT('Ctrl Pts',(-1.34716554820013,-1.,-1.72527410681298));
#23922=CARTESIAN_POINT('Ctrl Pts',(-1.3477930915247,-1.,-1.73040149654497));
#23923=CARTESIAN_POINT('Ctrl Pts',(-1.34824783113158,-1.,-1.73425417886255));
#23924=CARTESIAN_POINT('Ctrl Pts',(-1.34854391898145,-1.,-1.73682580585819));
#23925=CARTESIAN_POINT('Ctrl Pts',(-1.34869019493419,-1.,-1.73811241238545));
#23926=CARTESIAN_POINT('',(-1.23627494547115,-1.,-1.81978687191668));
#23927=CARTESIAN_POINT('',(-1.34869019493419,-1.,-1.73811241238545));
#23928=CARTESIAN_POINT('',(-0.892032620296855,-1.,-1.5055822144029));
#23929=CARTESIAN_POINT('Ctrl Pts',(-1.23627494547115,-1.,-1.81978687191668));
#23930=CARTESIAN_POINT('Ctrl Pts',(-1.23509651170384,-1.,-1.81925017193531));
#23931=CARTESIAN_POINT('Ctrl Pts',(-1.23274224526804,-1.,-1.81817389920914));
#23932=CARTESIAN_POINT('Ctrl Pts',(-1.22921864890975,-1.,-1.81655087183054));
#23933=CARTESIAN_POINT('Ctrl Pts',(-1.22453613304507,-1.,-1.81436959209778));
#23934=CARTESIAN_POINT('Ctrl Pts',(-1.2187090610323,-1.,-1.81161420806172));
#23935=CARTESIAN_POINT('Ctrl Pts',(-1.2129081570818,-1.,-1.80882996916931));
#23936=CARTESIAN_POINT('Ctrl Pts',(-1.20713356605519,-1.,-1.80601678480772));
#23937=CARTESIAN_POINT('Ctrl Pts',(-1.2013854893912,-1.,-1.8031745483882));
#23938=CARTESIAN_POINT('Ctrl Pts',(-1.19566418930405,-1.,-1.80030314370121));
#23939=CARTESIAN_POINT('Ctrl Pts',(-1.1899699793456,-1.,-1.79740245923649));
#23940=CARTESIAN_POINT('Ctrl Pts',(-1.18430321697471,-1.,-1.79447240321572));
#23941=CARTESIAN_POINT('Ctrl Pts',(-1.17866429440781,-1.,-1.79151291552646));
#23942=CARTESIAN_POINT('Ctrl Pts',(-1.17305363177265,-1.,-1.78852398877523));
#23943=CARTESIAN_POINT('Ctrl Pts',(-1.16747166312239,-1.,-1.78550566040349));
#23944=CARTESIAN_POINT('Ctrl Pts',(-1.16191881298458,-1.,-1.78245795880949));
#23945=CARTESIAN_POINT('Ctrl Pts',(-1.15639547194689,-1.,-1.77938085564261));
#23946=CARTESIAN_POINT('Ctrl Pts',(-1.15090197841531,-1.,-1.77627422557034));
#23947=CARTESIAN_POINT('Ctrl Pts',(-1.14543858226948,-1.,-1.77313777896234));
#23948=CARTESIAN_POINT('Ctrl Pts',(-1.14000548337,-1.,-1.76997111386806));
#23949=CARTESIAN_POINT('Ctrl Pts',(-1.13460291804635,-1.,-1.76677384551883));
#23950=CARTESIAN_POINT('Ctrl Pts',(-1.12923123555076,-1.,-1.76354571966171));
#23951=CARTESIAN_POINT('Ctrl Pts',(-1.12389096855078,-1.,-1.76028671825084));
#23952=CARTESIAN_POINT('Ctrl Pts',(-1.11858293216752,-1.,-1.75699720772089));
#23953=CARTESIAN_POINT('Ctrl Pts',(-1.11330807582542,-1.,-1.75367772094617));
#23954=CARTESIAN_POINT('Ctrl Pts',(-1.10806728183003,-1.,-1.75032866075914));
#23955=CARTESIAN_POINT('Ctrl Pts',(-1.10286118991144,-1.,-1.74695004214924));
#23956=CARTESIAN_POINT('Ctrl Pts',(-1.09768999241229,-1.,-1.74354119236212));
#23957=CARTESIAN_POINT('Ctrl Pts',(-1.09255329056496,-1.,-1.74010053962252));
#23958=CARTESIAN_POINT('Ctrl Pts',(-1.08745056285429,-1.,-1.73662628326093));
#23959=CARTESIAN_POINT('Ctrl Pts',(-1.08238162784749,-1.,-1.73311705663407));
#23960=CARTESIAN_POINT('Ctrl Pts',(-1.0773470373727,-1.,-1.72957248977424));
#23961=CARTESIAN_POINT('Ctrl Pts',(-1.07234866990252,-1.,-1.72599406198489));
#23962=CARTESIAN_POINT('Ctrl Pts',(-1.06738966975463,-1.,-1.72238500928456));
#23963=CARTESIAN_POINT('Ctrl Pts',(-1.0624732468065,-1.,-1.71874858456908));
#23964=CARTESIAN_POINT('Ctrl Pts',(-1.05760163192481,-1.,-1.71508654427022));
#23965=CARTESIAN_POINT('Ctrl Pts',(-1.05277517202854,-1.,-1.71139783543986));
#23966=CARTESIAN_POINT('Ctrl Pts',(-1.0479908540499,-1.,-1.70767646263641));
#23967=CARTESIAN_POINT('Ctrl Pts',(-1.04324363334546,-1.,-1.70391338707969));
#23968=CARTESIAN_POINT('Ctrl Pts',(-1.03852922490782,-1.,-1.70010052930951));
#23969=CARTESIAN_POINT('Ctrl Pts',(-1.03384646003587,-1.,-1.69623414782769));
#23970=CARTESIAN_POINT('Ctrl Pts',(-1.02919977579155,-1.,-1.69231840863471));
#23971=CARTESIAN_POINT('Ctrl Pts',(-1.02460180535272,-1.,-1.68836910178475));
#23972=CARTESIAN_POINT('Ctrl Pts',(-1.02006795074222,-1.,-1.68440578021739));
#23973=CARTESIAN_POINT('Ctrl Pts',(-1.01561026162787,-1.,-1.6804428989482));
#23974=CARTESIAN_POINT('Ctrl Pts',(-1.01123236493507,-1.,-1.67648246776457));
#23975=CARTESIAN_POINT('Ctrl Pts',(-1.00692206696387,-1.,-1.67250335383248));
#23976=CARTESIAN_POINT('Ctrl Pts',(-1.00265091003682,-1.,-1.66846059277231));
#23977=CARTESIAN_POINT('Ctrl Pts',(-0.998389654952317,-1.,-1.66430758030304));
#23978=CARTESIAN_POINT('Ctrl Pts',(-0.994121836661116,-1.,-1.66001553809916));
#23979=CARTESIAN_POINT('Ctrl Pts',(-0.98985562785445,-1.,-1.65559044289746));
#23980=CARTESIAN_POINT('Ctrl Pts',(-0.985642622921626,-1.,-1.6511001661277));
#23981=CARTESIAN_POINT('Ctrl Pts',(-0.981562530940574,-1.,-1.64665139190834));
#23982=CARTESIAN_POINT('Ctrl Pts',(-0.977689794120297,-1.,-1.64233990826831));
#23983=CARTESIAN_POINT('Ctrl Pts',(-0.974066058287501,-1.,-1.63820952658157));
#23984=CARTESIAN_POINT('Ctrl Pts',(-0.970669715996356,-1.,-1.63420665729609));
#23985=CARTESIAN_POINT('Ctrl Pts',(-0.967387853228041,-1.,-1.63013849959083));
#23986=CARTESIAN_POINT('Ctrl Pts',(-0.964046107037821,-1.,-1.6257193066974));
#23987=CARTESIAN_POINT('Ctrl Pts',(-0.960438326099958,-1.,-1.62061638139929));
#23988=CARTESIAN_POINT('Ctrl Pts',(-0.956354422921573,-1.,-1.61449324337233));
#23989=CARTESIAN_POINT('Ctrl Pts',(-0.951613284361248,-1.,-1.60706069897794));
#23990=CARTESIAN_POINT('Ctrl Pts',(-0.946078063325796,-1.,-1.59810042045408));
#23991=CARTESIAN_POINT('Ctrl Pts',(-0.939646377909319,-1.,-1.58744937489796));
#23992=CARTESIAN_POINT('Ctrl Pts',(-0.932246680128849,-1.,-1.57499388385561));
#23993=CARTESIAN_POINT('Ctrl Pts',(-0.923832188966322,-1.,-1.56065988582509));
#23994=CARTESIAN_POINT('Ctrl Pts',(-0.91437591904658,-1.,-1.54440491152808));
#23995=CARTESIAN_POINT('Ctrl Pts',(-0.905967409640499,-1.,-1.52984849890434));
#23996=CARTESIAN_POINT('Ctrl Pts',(-0.89918504749193,-1.,-1.51805569591479));
#23997=CARTESIAN_POINT('Ctrl Pts',(-0.894452006967538,-1.,-1.50980486807181));
#23998=CARTESIAN_POINT('Ctrl Pts',(-0.892032620296855,-1.,-1.5055822144029));
#23999=CARTESIAN_POINT('',(-0.693717979106305,-1.,-1.60662857109684));
#24000=CARTESIAN_POINT('Origin',(0.,-1.,0.));
#24001=CARTESIAN_POINT('',(-0.745574324794401,-1.,-2.0698113262342));
#24002=CARTESIAN_POINT('Ctrl Pts',(-0.693717979106305,-1.,-1.60662857109684));
#24003=CARTESIAN_POINT('Ctrl Pts',(-0.69571209787897,-1.,-1.61106790957619));
#24004=CARTESIAN_POINT('Ctrl Pts',(-0.699605146398837,-1.,-1.61974673471117));
#24005=CARTESIAN_POINT('Ctrl Pts',(-0.705159151977294,-1.,-1.6321654166204));
#24006=CARTESIAN_POINT('Ctrl Pts',(-0.711993139340447,-1.,-1.64752408828442));
#24007=CARTESIAN_POINT('Ctrl Pts',(-0.71958543378795,-1.,-1.66472880551777));
#24008=CARTESIAN_POINT('Ctrl Pts',(-0.726235967982445,-1.,-1.67996158451922));
#24009=CARTESIAN_POINT('Ctrl Pts',(-0.731963238685357,-1.,-1.69326921972915));
#24010=CARTESIAN_POINT('Ctrl Pts',(-0.736799665716932,-1.,-1.70473309004249));
#24011=CARTESIAN_POINT('Ctrl Pts',(-0.74079516202821,-1.,-1.71447789751001));
#24012=CARTESIAN_POINT('Ctrl Pts',(-0.744021445433093,-1.,-1.72268229916769));
#24013=CARTESIAN_POINT('Ctrl Pts',(-0.746574710097752,-1.,-1.72958533647714));
#24014=CARTESIAN_POINT('Ctrl Pts',(-0.74858246295687,-1.,-1.7355035168033));
#24015=CARTESIAN_POINT('Ctrl Pts',(-0.750193435981249,-1.,-1.74080458267114));
#24016=CARTESIAN_POINT('Ctrl Pts',(-0.751555614164482,-1.,-1.74585086852502));
#24017=CARTESIAN_POINT('Ctrl Pts',(-0.752797683531314,-1.,-1.75095139468794));
#24018=CARTESIAN_POINT('Ctrl Pts',(-0.754009254027829,-1.,-1.75631083600019));
#24019=CARTESIAN_POINT('Ctrl Pts',(-0.755220979974461,-1.,-1.76197817240128));
#24020=CARTESIAN_POINT('Ctrl Pts',(-0.75642189602781,-1.,-1.76789396002998));
#24021=CARTESIAN_POINT('Ctrl Pts',(-0.757578264077029,-1.,-1.77394167108292));
#24022=CARTESIAN_POINT('Ctrl Pts',(-0.758650626677518,-1.,-1.77999411220945));
#24023=CARTESIAN_POINT('Ctrl Pts',(-0.759614401110189,-1.,-1.78596964884604));
#24024=CARTESIAN_POINT('Ctrl Pts',(-0.760469555880749,-1.,-1.7918581561088));
#24025=CARTESIAN_POINT('Ctrl Pts',(-0.761229695230558,-1.,-1.79768986997783));
#24026=CARTESIAN_POINT('Ctrl Pts',(-0.761915336443547,-1.,-1.80351583877342));
#24027=CARTESIAN_POINT('Ctrl Pts',(-0.762546129463938,-1.,-1.80938551463965));
#24028=CARTESIAN_POINT('Ctrl Pts',(-0.763132003836634,-1.,-1.8153211840553));
#24029=CARTESIAN_POINT('Ctrl Pts',(-0.763673465462726,-1.,-1.82131873145266));
#24030=CARTESIAN_POINT('Ctrl Pts',(-0.764165902605995,-1.,-1.82735991200065));
#24031=CARTESIAN_POINT('Ctrl Pts',(-0.764602549687853,-1.,-1.83342077227142));
#24032=CARTESIAN_POINT('Ctrl Pts',(-0.764978057881737,-1.,-1.83948181064835));
#24033=CARTESIAN_POINT('Ctrl Pts',(-0.765291664862029,-1.,-1.84553698875924));
#24034=CARTESIAN_POINT('Ctrl Pts',(-0.765545710619062,-1.,-1.85158945130063));
#24035=CARTESIAN_POINT('Ctrl Pts',(-0.765744212909318,-1.,-1.85764741390394));
#24036=CARTESIAN_POINT('Ctrl Pts',(-0.765891519092547,-1.,-1.86372027063312));
#24037=CARTESIAN_POINT('Ctrl Pts',(-0.765990708546091,-1.,-1.86981398314341));
#24038=CARTESIAN_POINT('Ctrl Pts',(-0.766042837036744,-1.,-1.87592888967883));
#24039=CARTESIAN_POINT('Ctrl Pts',(-0.766047794851865,-1.,-1.88206215302561));
#24040=CARTESIAN_POINT('Ctrl Pts',(-0.766004837062091,-1.,-1.88820926433409));
#24041=CARTESIAN_POINT('Ctrl Pts',(-0.765913193856978,-1.,-1.89436577771388));
#24042=CARTESIAN_POINT('Ctrl Pts',(-0.765772772593386,-1.,-1.90052930393596));
#24043=CARTESIAN_POINT('Ctrl Pts',(-0.765584196937919,-1.,-1.90669961402356));
#24044=CARTESIAN_POINT('Ctrl Pts',(-0.765348465884722,-1.,-1.91287765805169));
#24045=CARTESIAN_POINT('Ctrl Pts',(-0.765066729667088,-1.,-1.91906491634196));
#24046=CARTESIAN_POINT('Ctrl Pts',(-0.764740025488211,-1.,-1.92526263537048));
#24047=CARTESIAN_POINT('Ctrl Pts',(-0.764369010673941,-1.,-1.93147105496382));
#24048=CARTESIAN_POINT('Ctrl Pts',(-0.763954049121458,-1.,-1.93768964875886));
#24049=CARTESIAN_POINT('Ctrl Pts',(-0.763495333538629,-1.,-1.9439174661764));
#24050=CARTESIAN_POINT('Ctrl Pts',(-0.762992990878769,-1.,-1.95015342590024));
#24051=CARTESIAN_POINT('Ctrl Pts',(-0.762447203806179,-1.,-1.95639665309869));
#24052=CARTESIAN_POINT('Ctrl Pts',(-0.761858300014423,-1.,-1.96264672744186));
#24053=CARTESIAN_POINT('Ctrl Pts',(-0.76122669048382,-1.,-1.96890351582499));
#24054=CARTESIAN_POINT('Ctrl Pts',(-0.760552825409757,-1.,-1.97516705321494));
#24055=CARTESIAN_POINT('Ctrl Pts',(-0.75983714745219,-1.,-1.98143741418172));
#24056=CARTESIAN_POINT('Ctrl Pts',(-0.759080037802488,-1.,-1.98771456680874));
#24057=CARTESIAN_POINT('Ctrl Pts',(-0.758281796766761,-1.,-1.99399831098817));
#24058=CARTESIAN_POINT('Ctrl Pts',(-0.757442676862724,-1.,-2.00028834739178));
#24059=CARTESIAN_POINT('Ctrl Pts',(-0.75656290464667,-1.,-2.0065843158773));
#24060=CARTESIAN_POINT('Ctrl Pts',(-0.755642704957865,-1.,-2.01288584328084));
#24061=CARTESIAN_POINT('Ctrl Pts',(-0.754682330722816,-1.,-2.01919259405809));
#24062=CARTESIAN_POINT('Ctrl Pts',(-0.753682061112768,-1.,-2.02550428623313));
#24063=CARTESIAN_POINT('Ctrl Pts',(-0.752642180487211,-1.,-2.03182068456221));
#24064=CARTESIAN_POINT('Ctrl Pts',(-0.751562963361115,-1.,-2.03814160092099));
#24065=CARTESIAN_POINT('Ctrl Pts',(-0.750444657875576,-1.,-2.04446689147979));
#24066=CARTESIAN_POINT('Ctrl Pts',(-0.749287468665046,-1.,-2.05079645592154));
#24067=CARTESIAN_POINT('Ctrl Pts',(-0.748091554183802,-1.,-2.05713023031006));
#24068=CARTESIAN_POINT('Ctrl Pts',(-0.747103932787919,-1.,-2.06220058927826));
#24069=CARTESIAN_POINT('Ctrl Pts',(-0.7463458715442,-1.,-2.06600523016815));
#24070=CARTESIAN_POINT('Ctrl Pts',(-0.745832791378367,-1.,-2.06854248895728));
#24071=CARTESIAN_POINT('Ctrl Pts',(-0.745574324794401,-1.,-2.0698113262342));
#24072=CARTESIAN_POINT('',(-0.61342227326009,-1.,-2.11275013067528));
#24073=CARTESIAN_POINT('',(-0.745574324794401,-1.,-2.0698113262342));
#24074=CARTESIAN_POINT('',(-0.383122945602004,-1.,-1.7075470150345));
#24075=CARTESIAN_POINT('Ctrl Pts',(-0.61342227326009,-1.,-2.11275013067528));
#24076=CARTESIAN_POINT('Ctrl Pts',(-0.6124673655618,-1.,-2.11187554259986));
#24077=CARTESIAN_POINT('Ctrl Pts',(-0.610560911689899,-1.,-2.11012443807238));
#24078=CARTESIAN_POINT('Ctrl Pts',(-0.607711315454876,-1.,-2.1074919961518));
#24079=CARTESIAN_POINT('Ctrl Pts',(-0.60393203073603,-1.,-2.10397049886949));
#24080=CARTESIAN_POINT('Ctrl Pts',(-0.599241616420533,-1.,-2.0995493086477));
#24081=CARTESIAN_POINT('Ctrl Pts',(-0.594585006052162,-1.,-2.0951087622027));
#24082=CARTESIAN_POINT('Ctrl Pts',(-0.589962365403406,-1.,-2.09064881812129));
#24083=CARTESIAN_POINT('Ctrl Pts',(-0.585373918991617,-1.,-2.08616943727951));
#24084=CARTESIAN_POINT('Ctrl Pts',(-0.580819952108063,-1.,-2.08167059018418));
#24085=CARTESIAN_POINT('Ctrl Pts',(-0.576300797416844,-1.,-2.07715226767559));
#24086=CARTESIAN_POINT('Ctrl Pts',(-0.571816823242603,-1.,-2.07261449292824));
#24087=CARTESIAN_POINT('Ctrl Pts',(-0.567368421181087,-1.,-2.06805732997334));
#24088=CARTESIAN_POINT('Ctrl Pts',(-0.562955993082261,-1.,-2.06348090160589));
#24089=CARTESIAN_POINT('Ctrl Pts',(-0.558579940185151,-1.,-2.05888537756462));
#24090=CARTESIAN_POINT('Ctrl Pts',(-0.554240657463906,-1.,-2.05427091604413));
#24091=CARTESIAN_POINT('Ctrl Pts',(-0.549938525150295,-1.,-2.04963761077958));
#24092=CARTESIAN_POINT('Ctrl Pts',(-0.54567390381743,-1.,-2.04498544714588));
#24093=CARTESIAN_POINT('Ctrl Pts',(-0.541447120615659,-1.,-2.04031422690527));
#24094=CARTESIAN_POINT('Ctrl Pts',(-0.537258489833262,-1.,-2.03562362954037));
#24095=CARTESIAN_POINT('Ctrl Pts',(-0.533108355132977,-1.,-2.03091336214426));
#24096=CARTESIAN_POINT('Ctrl Pts',(-0.528997127241914,-1.,-2.0261832908329));
#24097=CARTESIAN_POINT('Ctrl Pts',(-0.524925318333476,-1.,-2.02143356304698));
#24098=CARTESIAN_POINT('Ctrl Pts',(-0.52089359039937,-1.,-2.01666477917286));
#24099=CARTESIAN_POINT('Ctrl Pts',(-0.516902681728687,-1.,-2.01187773939242));
#24100=CARTESIAN_POINT('Ctrl Pts',(-0.512953306961792,-1.,-2.00707309946949));
#24101=CARTESIAN_POINT('Ctrl Pts',(-0.509046069886157,-1.,-2.00225107134734));
#24102=CARTESIAN_POINT('Ctrl Pts',(-0.505181361323026,-1.,-1.99741107463572));
#24103=CARTESIAN_POINT('Ctrl Pts',(-0.501359287727146,-1.,-1.99255149126155));
#24104=CARTESIAN_POINT('Ctrl Pts',(-0.497579909545574,-1.,-1.98767044752932));
#24105=CARTESIAN_POINT('Ctrl Pts',(-0.493843476541495,-1.,-1.98276658761821));
#24106=CARTESIAN_POINT('Ctrl Pts',(-0.490150627860952,-1.,-1.97783973019229));
#24107=CARTESIAN_POINT('Ctrl Pts',(-0.486502692907659,-1.,-1.97289186263272));
#24108=CARTESIAN_POINT('Ctrl Pts',(-0.482901662120691,-1.,-1.96792703422362));
#24109=CARTESIAN_POINT('Ctrl Pts',(-0.479349583074855,-1.,-1.96294933055943));
#24110=CARTESIAN_POINT('Ctrl Pts',(-0.475848034683176,-1.,-1.95796111148177));
#24111=CARTESIAN_POINT('Ctrl Pts',(-0.472397672264072,-1.,-1.95296148278133));
#24112=CARTESIAN_POINT('Ctrl Pts',(-0.468997482913135,-1.,-1.94794381136514));
#24113=CARTESIAN_POINT('Ctrl Pts',(-0.46564546202603,-1.,-1.9428979419619));
#24114=CARTESIAN_POINT('Ctrl Pts',(-0.462340031009056,-1.,-1.93781486640821));
#24115=CARTESIAN_POINT('Ctrl Pts',(-0.459081234547926,-1.,-1.93269066517934));
#24116=CARTESIAN_POINT('Ctrl Pts',(-0.455872005174371,-1.,-1.92753067150476));
#24117=CARTESIAN_POINT('Ctrl Pts',(-0.452719478359432,-1.,-1.92235380648502));
#24118=CARTESIAN_POINT('Ctrl Pts',(-0.449632260106662,-1.,-1.91718342555755));
#24119=CARTESIAN_POINT('Ctrl Pts',(-0.446617343485711,-1.,-1.9120369998112));
#24120=CARTESIAN_POINT('Ctrl Pts',(-0.443677556849151,-1.,-1.90691756144898));
#24121=CARTESIAN_POINT('Ctrl Pts',(-0.440807833704038,-1.,-1.90180124389086));
#24122=CARTESIAN_POINT('Ctrl Pts',(-0.437995003948244,-1.,-1.89663648956466));
#24123=CARTESIAN_POINT('Ctrl Pts',(-0.435225660963383,-1.,-1.89136993975504));
#24124=CARTESIAN_POINT('Ctrl Pts',(-0.432493038548748,-1.,-1.88596913666793));
#24125=CARTESIAN_POINT('Ctrl Pts',(-0.429803062482344,-1.,-1.88044229001832));
#24126=CARTESIAN_POINT('Ctrl Pts',(-0.427183828519102,-1.,-1.87486989291484));
#24127=CARTESIAN_POINT('Ctrl Pts',(-0.424678177291359,-1.,-1.86937803944323));
#24128=CARTESIAN_POINT('Ctrl Pts',(-0.422327307418275,-1.,-1.86408083334028));
#24129=CARTESIAN_POINT('Ctrl Pts',(-0.420157287975619,-1.,-1.85903281096686));
#24130=CARTESIAN_POINT('Ctrl Pts',(-0.418164129143534,-1.,-1.85417632856234));
#24131=CARTESIAN_POINT('Ctrl Pts',(-0.416300022038864,-1.,-1.84929312929882));
#24132=CARTESIAN_POINT('Ctrl Pts',(-0.41448743825434,-1.,-1.8440575707371));
#24133=CARTESIAN_POINT('Ctrl Pts',(-0.412633125322162,-1.,-1.83808953475839));
#24134=CARTESIAN_POINT('Ctrl Pts',(-0.410641256301675,-1.,-1.83100408895216));
#24135=CARTESIAN_POINT('Ctrl Pts',(-0.408428948108533,-1.,-1.8224702267854));
#24136=CARTESIAN_POINT('Ctrl Pts',(-0.405933518411838,-1.,-1.81223801813988));
#24137=CARTESIAN_POINT('Ctrl Pts',(-0.403107976170441,-1.,-1.80012077176221));
#24138=CARTESIAN_POINT('Ctrl Pts',(-0.39991940378308,-1.,-1.78598826347533));
#24139=CARTESIAN_POINT('Ctrl Pts',(-0.39634619612042,-1.,-1.7697556004756));
#24140=CARTESIAN_POINT('Ctrl Pts',(-0.392375812294307,-1.,-1.75137405313962));
#24141=CARTESIAN_POINT('Ctrl Pts',(-0.388877023509191,-1.,-1.7349317097561));
#24142=CARTESIAN_POINT('Ctrl Pts',(-0.38607079032701,-1.,-1.72162022246158));
#24143=CARTESIAN_POINT('Ctrl Pts',(-0.384119047315542,-1.,-1.71231062891958));
#24144=CARTESIAN_POINT('Ctrl Pts',(-0.383122945602004,-1.,-1.7075470150345));
#24145=CARTESIAN_POINT('',(-0.163289472382896,-1.,-1.74236521665491));
#24146=CARTESIAN_POINT('Origin',(0.,-1.,0.));
#24147=CARTESIAN_POINT('',(-0.0694764450219581,-1.,-2.19890268624765));
#24148=CARTESIAN_POINT('Ctrl Pts',(-0.163289472382896,-1.,-1.74236521665491));
#24149=CARTESIAN_POINT('Ctrl Pts',(-0.163814161002002,-1.,-1.7472034950333));
#24150=CARTESIAN_POINT('Ctrl Pts',(-0.164834765707158,-1.,-1.75666056638427));
#24151=CARTESIAN_POINT('Ctrl Pts',(-0.1662793551464,-1.,-1.77018771684844));
#24152=CARTESIAN_POINT('Ctrl Pts',(-0.168032772805197,-1.,-1.7869064998507));
#24153=CARTESIAN_POINT('Ctrl Pts',(-0.169936923904608,-1.,-1.80561530629706));
#24154=CARTESIAN_POINT('Ctrl Pts',(-0.171554770204119,-1.,-1.82215766811545));
#24155=CARTESIAN_POINT('Ctrl Pts',(-0.1728894428919,-1.,-1.83658380527692));
#24156=CARTESIAN_POINT('Ctrl Pts',(-0.173946627587731,-1.,-1.8489811319852));
#24157=CARTESIAN_POINT('Ctrl Pts',(-0.17473525927603,-1.,-1.85948367088837));
#24158=CARTESIAN_POINT('Ctrl Pts',(-0.175268337590758,-1.,-1.86828349694799));
#24159=CARTESIAN_POINT('Ctrl Pts',(-0.175563480746485,-1.,-1.87563767773588));
#24160=CARTESIAN_POINT('Ctrl Pts',(-0.175644148889699,-1.,-1.88188663145367));
#24161=CARTESIAN_POINT('Ctrl Pts',(-0.175538155840648,-1.,-1.88742606273259));
#24162=CARTESIAN_POINT('Ctrl Pts',(-0.175274276190844,-1.,-1.892646301985));
#24163=CARTESIAN_POINT('Ctrl Pts',(-0.174879405091263,-1.,-1.89788101117132));
#24164=CARTESIAN_POINT('Ctrl Pts',(-0.174375518661085,-1.,-1.90335253862834));
#24165=CARTESIAN_POINT('Ctrl Pts',(-0.173776635257817,-1.,-1.90911693975267));
#24166=CARTESIAN_POINT('Ctrl Pts',(-0.173090695383496,-1.,-1.91511429159527));
#24167=CARTESIAN_POINT('Ctrl Pts',(-0.172321621259514,-1.,-1.9212233439798));
#24168=CARTESIAN_POINT('Ctrl Pts',(-0.171471191532988,-1.,-1.92731093582036));
#24169=CARTESIAN_POINT('Ctrl Pts',(-0.170541253116202,-1.,-1.93329183155539));
#24170=CARTESIAN_POINT('Ctrl Pts',(-0.169534904817491,-1.,-1.93915639211581));
#24171=CARTESIAN_POINT('Ctrl Pts',(-0.168455741607556,-1.,-1.94493757756931));
#24172=CARTESIAN_POINT('Ctrl Pts',(-0.167307501784475,-1.,-1.95069027794294));
#24173=CARTESIAN_POINT('Ctrl Pts',(-0.166093592002812,-1.,-1.9564675971873));
#24174=CARTESIAN_POINT('Ctrl Pts',(-0.164816568920269,-1.,-1.96229379940136));
#24175=CARTESIAN_POINT('Ctrl Pts',(-0.163478185457734,-1.,-1.96816512677967));
#24176=CARTESIAN_POINT('Ctrl Pts',(-0.162079693556289,-1.,-1.97406280235188));
#24177=CARTESIAN_POINT('Ctrl Pts',(-0.160622060784611,-1.,-1.97996195437559));
#24178=CARTESIAN_POINT('Ctrl Pts',(-0.159106226437299,-1.,-1.98584238283292));
#24179=CARTESIAN_POINT('Ctrl Pts',(-0.157533331459227,-1.,-1.99169810931908));
#24180=CARTESIAN_POINT('Ctrl Pts',(-0.155904629548783,-1.,-1.99753284771497));
#24181=CARTESIAN_POINT('Ctrl Pts',(-0.154221403049722,-1.,-2.00335565310543));
#24182=CARTESIAN_POINT('Ctrl Pts',(-0.15248488362145,-1.,-2.00917680318424));
#24183=CARTESIAN_POINT('Ctrl Pts',(-0.150696157673078,-1.,-2.01500291940238));
#24184=CARTESIAN_POINT('Ctrl Pts',(-0.148856124775337,-1.,-2.02083464969894));
#24185=CARTESIAN_POINT('Ctrl Pts',(-0.146965557332583,-1.,-2.02666926182017));
#24186=CARTESIAN_POINT('Ctrl Pts',(-0.145025140186057,-1.,-2.03250223739942));
#24187=CARTESIAN_POINT('Ctrl Pts',(-0.143035515058209,-1.,-2.03832911025912));
#24188=CARTESIAN_POINT('Ctrl Pts',(-0.140997332152546,-1.,-2.04414757947916));
#24189=CARTESIAN_POINT('Ctrl Pts',(-0.138911255368966,-1.,-2.04995762001328));
#24190=CARTESIAN_POINT('Ctrl Pts',(-0.136777941218044,-1.,-2.05576044414264));
#24191=CARTESIAN_POINT('Ctrl Pts',(-0.134598026192106,-1.,-2.06155781517842));
#24192=CARTESIAN_POINT('Ctrl Pts',(-0.13237211154771,-1.,-2.06735123910326));
#24193=CARTESIAN_POINT('Ctrl Pts',(-0.130100748328403,-1.,-2.07314114713063));
#24194=CARTESIAN_POINT('Ctrl Pts',(-0.12778444527612,-1.,-2.07892715110987));
#24195=CARTESIAN_POINT('Ctrl Pts',(-0.125423679412061,-1.,-2.08470840653643));
#24196=CARTESIAN_POINT('Ctrl Pts',(-0.123018905621083,-1.,-2.09048392424825));
#24197=CARTESIAN_POINT('Ctrl Pts',(-0.120570567965122,-1.,-2.0962529286773));
#24198=CARTESIAN_POINT('Ctrl Pts',(-0.118079107988355,-1.,-2.102015121329));
#24199=CARTESIAN_POINT('Ctrl Pts',(-0.115544957687926,-1.,-2.10777050261309));
#24200=CARTESIAN_POINT('Ctrl Pts',(-0.112968534419737,-1.,-2.11351924490306));
#24201=CARTESIAN_POINT('Ctrl Pts',(-0.110350236135025,-1.,-2.11926155590865));
#24202=CARTESIAN_POINT('Ctrl Pts',(-0.10769043523109,-1.,-2.12499752307));
#24203=CARTESIAN_POINT('Ctrl Pts',(-0.104989479152739,-1.,-2.13072704887293));
#24204=CARTESIAN_POINT('Ctrl Pts',(-0.1022477005561,-1.,-2.13644992667165));
#24205=CARTESIAN_POINT('Ctrl Pts',(-0.0994654261990915,-1.,-2.14216588396025));
#24206=CARTESIAN_POINT('Ctrl Pts',(-0.0966429852305459,-1.,-2.14787463531795));
#24207=CARTESIAN_POINT('Ctrl Pts',(-0.0937807218867643,-1.,-2.1535759397817));
#24208=CARTESIAN_POINT('Ctrl Pts',(-0.0908789888107265,-1.,-2.15926961544516));
#24209=CARTESIAN_POINT('Ctrl Pts',(-0.0879381291386923,-1.,-2.16495552645014));
#24210=CARTESIAN_POINT('Ctrl Pts',(-0.0849584620835372,-1.,-2.17063357870952));
#24211=CARTESIAN_POINT('Ctrl Pts',(-0.0819402680872765,-1.,-2.176303712113));
#24212=CARTESIAN_POINT('Ctrl Pts',(-0.0788837727685243,-1.,-2.18196589448887));
#24213=CARTESIAN_POINT('Ctrl Pts',(-0.0757891465836148,-1.,-2.1876201139953));
#24214=CARTESIAN_POINT('Ctrl Pts',(-0.0732830357306725,-1.,-2.19213712013662));
#24215=CARTESIAN_POINT('Ctrl Pts',(-0.0713863779526154,-1.,-2.19552129484002));
#24216=CARTESIAN_POINT('Ctrl Pts',(-0.070114353632549,-1.,-2.19777582085423));
#24217=CARTESIAN_POINT('Ctrl Pts',(-0.0694764450219581,-1.,-2.19890268624765));
#24218=CARTESIAN_POINT('',(0.0694764450219584,-1.,-2.19890268624765));
#24219=CARTESIAN_POINT('',(-0.0694764450219581,-1.,-2.19890268624765));
#24220=CARTESIAN_POINT('',(0.163289472382896,-1.,-1.74236521665491));
#24221=CARTESIAN_POINT('Ctrl Pts',(0.0694764450219584,-1.,-2.19890268624765));
#24222=CARTESIAN_POINT('Ctrl Pts',(0.0701143536324926,-1.,-2.19777582085261));
#24223=CARTESIAN_POINT('Ctrl Pts',(0.0713863779524627,-1.,-2.19552129483562));
#24224=CARTESIAN_POINT('Ctrl Pts',(0.0732830357304276,-1.,-2.19213712012956));
#24225=CARTESIAN_POINT('Ctrl Pts',(0.0757891465833411,-1.,-2.1876201139874));
#24226=CARTESIAN_POINT('Ctrl Pts',(0.0788837727683228,-1.,-2.18196589448304));
#24227=CARTESIAN_POINT('Ctrl Pts',(0.0819402680871939,-1.,-2.1763037121106));
#24228=CARTESIAN_POINT('Ctrl Pts',(0.0849584620835643,-1.,-2.17063357871031));
#24229=CARTESIAN_POINT('Ctrl Pts',(0.0879381291387823,-1.,-2.16495552645275));
#24230=CARTESIAN_POINT('Ctrl Pts',(0.0908789888108266,-1.,-2.15926961544808));
#24231=CARTESIAN_POINT('Ctrl Pts',(0.0937807218868345,-1.,-2.15357593978377));
#24232=CARTESIAN_POINT('Ctrl Pts',(0.0966429852305689,-1.,-2.14787463531864));
#24233=CARTESIAN_POINT('Ctrl Pts',(0.0994654261990743,-1.,-2.14216588395974));
#24234=CARTESIAN_POINT('Ctrl Pts',(0.102247700556064,-1.,-2.13644992667052));
#24235=CARTESIAN_POINT('Ctrl Pts',(0.104989479152703,-1.,-2.1307270488718));
#24236=CARTESIAN_POINT('Ctrl Pts',(0.107690435231068,-1.,-2.12499752306927));
#24237=CARTESIAN_POINT('Ctrl Pts',(0.11035023613502,-1.,-2.11926155590849));
#24238=CARTESIAN_POINT('Ctrl Pts',(0.112968534419746,-1.,-2.11351924490335));
#24239=CARTESIAN_POINT('Ctrl Pts',(0.11554495768794,-1.,-2.10777050261359));
#24240=CARTESIAN_POINT('Ctrl Pts',(0.118079107988368,-1.,-2.10201512132945));
#24241=CARTESIAN_POINT('Ctrl Pts',(0.120570567965129,-1.,-2.09625292867756));
#24242=CARTESIAN_POINT('Ctrl Pts',(0.123018905621083,-1.,-2.09048392424826));
#24243=CARTESIAN_POINT('Ctrl Pts',(0.125423679412058,-1.,-2.08470840653628));
#24244=CARTESIAN_POINT('Ctrl Pts',(0.127784445276116,-1.,-2.07892715110967));
#24245=CARTESIAN_POINT('Ctrl Pts',(0.1301007483284,-1.,-2.07314114713047));
#24246=CARTESIAN_POINT('Ctrl Pts',(0.13237211154771,-1.,-2.06735123910319));
#24247=CARTESIAN_POINT('Ctrl Pts',(0.134598026192107,-1.,-2.06155781517844));
#24248=CARTESIAN_POINT('Ctrl Pts',(0.136777941218044,-1.,-2.0557604441427));
#24249=CARTESIAN_POINT('Ctrl Pts',(0.138911255368966,-1.,-2.04995762001333));
#24250=CARTESIAN_POINT('Ctrl Pts',(0.140997332152545,-1.,-2.04414757947919));
#24251=CARTESIAN_POINT('Ctrl Pts',(0.143035515058208,-1.,-2.03832911025913));
#24252=CARTESIAN_POINT('Ctrl Pts',(0.145025140186058,-1.,-2.03250223739941));
#24253=CARTESIAN_POINT('Ctrl Pts',(0.146965557332586,-1.,-2.02666926182017));
#24254=CARTESIAN_POINT('Ctrl Pts',(0.148856124775343,-1.,-2.02083464969897));
#24255=CARTESIAN_POINT('Ctrl Pts',(0.150696157673084,-1.,-2.01500291940243));
#24256=CARTESIAN_POINT('Ctrl Pts',(0.152484883621452,-1.,-2.00917680318426));
#24257=CARTESIAN_POINT('Ctrl Pts',(0.154221403049719,-1.,-2.00335565310539));
#24258=CARTESIAN_POINT('Ctrl Pts',(0.155904629548774,-1.,-1.99753284771487));
#24259=CARTESIAN_POINT('Ctrl Pts',(0.157533331459215,-1.,-1.99169810931893));
#24260=CARTESIAN_POINT('Ctrl Pts',(0.159106226437288,-1.,-1.98584238283279));
#24261=CARTESIAN_POINT('Ctrl Pts',(0.16062206078461,-1.,-1.97996195437557));
#24262=CARTESIAN_POINT('Ctrl Pts',(0.162079693556302,-1.,-1.97406280235204));
#24263=CARTESIAN_POINT('Ctrl Pts',(0.16347818545776,-1.,-1.96816512678));
#24264=CARTESIAN_POINT('Ctrl Pts',(0.1648165689203,-1.,-1.96229379940174));
#24265=CARTESIAN_POINT('Ctrl Pts',(0.166093592002833,-1.,-1.95646759718755));
#24266=CARTESIAN_POINT('Ctrl Pts',(0.167307501784469,-1.,-1.95069027794286));
#24267=CARTESIAN_POINT('Ctrl Pts',(0.168455741607516,-1.,-1.94493757756879));
#24268=CARTESIAN_POINT('Ctrl Pts',(0.169534904817425,-1.,-1.93915639211497));
#24269=CARTESIAN_POINT('Ctrl Pts',(0.170541253116136,-1.,-1.93329183155455));
#24270=CARTESIAN_POINT('Ctrl Pts',(0.17147119153296,-1.,-1.92731093582));
#24271=CARTESIAN_POINT('Ctrl Pts',(0.172321621259557,-1.,-1.92122334398034));
#24272=CARTESIAN_POINT('Ctrl Pts',(0.173090695383619,-1.,-1.91511429159681));
#24273=CARTESIAN_POINT('Ctrl Pts',(0.173776635257984,-1.,-1.90911693975475));
#24274=CARTESIAN_POINT('Ctrl Pts',(0.174375518661222,-1.,-1.90335253863003));
#24275=CARTESIAN_POINT('Ctrl Pts',(0.174879405091277,-1.,-1.89788101117148));
#24276=CARTESIAN_POINT('Ctrl Pts',(0.175274276190664,-1.,-1.89264630198279));
#24277=CARTESIAN_POINT('Ctrl Pts',(0.175538155840286,-1.,-1.88742606272818));
#24278=CARTESIAN_POINT('Ctrl Pts',(0.175644148889271,-1.,-1.88188663144846));
#24279=CARTESIAN_POINT('Ctrl Pts',(0.175563480746205,-1.,-1.87563767773249));
#24280=CARTESIAN_POINT('Ctrl Pts',(0.175268337590901,-1.,-1.86828349694972));
#24281=CARTESIAN_POINT('Ctrl Pts',(0.174735259276856,-1.,-1.85948367089838));
#24282=CARTESIAN_POINT('Ctrl Pts',(0.173946627589401,-1.,-1.84898113200543));
#24283=CARTESIAN_POINT('Ctrl Pts',(0.17288944289442,-1.,-1.83658380530747));
#24284=CARTESIAN_POINT('Ctrl Pts',(0.171554770207306,-1.,-1.82215766815414));
#24285=CARTESIAN_POINT('Ctrl Pts',(0.169936923908078,-1.,-1.80561530633924));
#24286=CARTESIAN_POINT('Ctrl Pts',(0.16803277280837,-1.,-1.78690649988931));
#24287=CARTESIAN_POINT('Ctrl Pts',(0.166279355148738,-1.,-1.77018771687692));
#24288=CARTESIAN_POINT('Ctrl Pts',(0.164834765708484,-1.,-1.75666056640041));
#24289=CARTESIAN_POINT('Ctrl Pts',(0.163814161002474,-1.,-1.74720349503904));
#24290=CARTESIAN_POINT('Ctrl Pts',(0.163289472382896,-1.,-1.74236521665491));
#24291=CARTESIAN_POINT('',(0.383122945602004,-1.,-1.7075470150345));
#24292=CARTESIAN_POINT('Origin',(0.,-1.,0.));
#24293=CARTESIAN_POINT('',(0.61342227326009,-1.,-2.11275013067528));
#24294=CARTESIAN_POINT('Ctrl Pts',(0.383122945602004,-1.,-1.7075470150345));
#24295=CARTESIAN_POINT('Ctrl Pts',(0.384119047314215,-1.,-1.71231062891398));
#24296=CARTESIAN_POINT('Ctrl Pts',(0.386070790323281,-1.,-1.72162022244582));
#24297=CARTESIAN_POINT('Ctrl Pts',(0.388877023502615,-1.,-1.73493170972829));
#24298=CARTESIAN_POINT('Ctrl Pts',(0.392375812285395,-1.,-1.75137405310193));
#24299=CARTESIAN_POINT('Ctrl Pts',(0.396346196110688,-1.,-1.76975560043442));
#24300=CARTESIAN_POINT('Ctrl Pts',(0.399919403774155,-1.,-1.78598826343754));
#24301=CARTESIAN_POINT('Ctrl Pts',(0.403107976163396,-1.,-1.80012077173238));
#24302=CARTESIAN_POINT('Ctrl Pts',(0.405933518407175,-1.,-1.81223801812013));
#24303=CARTESIAN_POINT('Ctrl Pts',(0.408428948106227,-1.,-1.82247022677562));
#24304=CARTESIAN_POINT('Ctrl Pts',(0.410641256301276,-1.,-1.83100408895047));
#24305=CARTESIAN_POINT('Ctrl Pts',(0.412633125322945,-1.,-1.8380895347617));
#24306=CARTESIAN_POINT('Ctrl Pts',(0.414487438255542,-1.,-1.84405757074218));
#24307=CARTESIAN_POINT('Ctrl Pts',(0.416300022039885,-1.,-1.84929312930314));
#24308=CARTESIAN_POINT('Ctrl Pts',(0.418164129144045,-1.,-1.8541763285645));
#24309=CARTESIAN_POINT('Ctrl Pts',(0.420157287975583,-1.,-1.8590328109667));
#24310=CARTESIAN_POINT('Ctrl Pts',(0.422327307417884,-1.,-1.86408083333863));
#24311=CARTESIAN_POINT('Ctrl Pts',(0.424678177290876,-1.,-1.8693780394412));
#24312=CARTESIAN_POINT('Ctrl Pts',(0.427183828518743,-1.,-1.87486989291334));
#24313=CARTESIAN_POINT('Ctrl Pts',(0.429803062482217,-1.,-1.88044229001779));
#24314=CARTESIAN_POINT('Ctrl Pts',(0.432493038548833,-1.,-1.88596913666828));
#24315=CARTESIAN_POINT('Ctrl Pts',(0.43522566096358,-1.,-1.89136993975585));
#24316=CARTESIAN_POINT('Ctrl Pts',(0.437995003948443,-1.,-1.89663648956549));
#24317=CARTESIAN_POINT('Ctrl Pts',(0.44080783370416,-1.,-1.90180124389137));
#24318=CARTESIAN_POINT('Ctrl Pts',(0.44367755684917,-1.,-1.90691756144906));
#24319=CARTESIAN_POINT('Ctrl Pts',(0.446617343485651,-1.,-1.91203699981095));
#24320=CARTESIAN_POINT('Ctrl Pts',(0.449632260106572,-1.,-1.91718342555717));
#24321=CARTESIAN_POINT('Ctrl Pts',(0.452719478359356,-1.,-1.9223538064847));
#24322=CARTESIAN_POINT('Ctrl Pts',(0.455872005174335,-1.,-1.92753067150461));
#24323=CARTESIAN_POINT('Ctrl Pts',(0.459081234547931,-1.,-1.93269066517936));
#24324=CARTESIAN_POINT('Ctrl Pts',(0.462340031009087,-1.,-1.93781486640834));
#24325=CARTESIAN_POINT('Ctrl Pts',(0.465645462026064,-1.,-1.94289794196205));
#24326=CARTESIAN_POINT('Ctrl Pts',(0.468997482913158,-1.,-1.94794381136524));
#24327=CARTESIAN_POINT('Ctrl Pts',(0.472397672264079,-1.,-1.95296148278136));
#24328=CARTESIAN_POINT('Ctrl Pts',(0.475848034683171,-1.,-1.95796111148175));
#24329=CARTESIAN_POINT('Ctrl Pts',(0.479349583074846,-1.,-1.96294933055938));
#24330=CARTESIAN_POINT('Ctrl Pts',(0.482901662120686,-1.,-1.96792703422358));
#24331=CARTESIAN_POINT('Ctrl Pts',(0.486502692907661,-1.,-1.97289186263272));
#24332=CARTESIAN_POINT('Ctrl Pts',(0.490150627860955,-1.,-1.97783973019229));
#24333=CARTESIAN_POINT('Ctrl Pts',(0.493843476541492,-1.,-1.9827665876182));
#24334=CARTESIAN_POINT('Ctrl Pts',(0.497579909545564,-1.,-1.98767044752929));
#24335=CARTESIAN_POINT('Ctrl Pts',(0.501359287727129,-1.,-1.9925514912615));
#24336=CARTESIAN_POINT('Ctrl Pts',(0.505181361323011,-1.,-1.99741107463567));
#24337=CARTESIAN_POINT('Ctrl Pts',(0.509046069886152,-1.,-2.00225107134733));
#24338=CARTESIAN_POINT('Ctrl Pts',(0.512953306961813,-1.,-2.00707309946955));
#24339=CARTESIAN_POINT('Ctrl Pts',(0.516902681728733,-1.,-2.01187773939257));
#24340=CARTESIAN_POINT('Ctrl Pts',(0.520893590399428,-1.,-2.01666477917306));
#24341=CARTESIAN_POINT('Ctrl Pts',(0.524925318333518,-1.,-2.02143356304712));
#24342=CARTESIAN_POINT('Ctrl Pts',(0.52899712724191,-1.,-2.02618329083289));
#24343=CARTESIAN_POINT('Ctrl Pts',(0.533108355132905,-1.,-2.03091336214401));
#24344=CARTESIAN_POINT('Ctrl Pts',(0.537258489833134,-1.,-2.03562362953993));
#24345=CARTESIAN_POINT('Ctrl Pts',(0.54144712061552,-1.,-2.0403142269048));
#24346=CARTESIAN_POINT('Ctrl Pts',(0.545673903817348,-1.,-2.0449854471456));
#24347=CARTESIAN_POINT('Ctrl Pts',(0.549938525150342,-1.,-2.04963761077974));
#24348=CARTESIAN_POINT('Ctrl Pts',(0.554240657464109,-1.,-2.05427091604482));
#24349=CARTESIAN_POINT('Ctrl Pts',(0.558579940185467,-1.,-2.05888537756571));
#24350=CARTESIAN_POINT('Ctrl Pts',(0.562955993082574,-1.,-2.06348090160697));
#24351=CARTESIAN_POINT('Ctrl Pts',(0.567368421181229,-1.,-2.06805732997383));
#24352=CARTESIAN_POINT('Ctrl Pts',(0.571816823242411,-1.,-2.07261449292758));
#24353=CARTESIAN_POINT('Ctrl Pts',(0.576300797416274,-1.,-2.07715226767361));
#24354=CARTESIAN_POINT('Ctrl Pts',(0.580819952107256,-1.,-2.08167059018138));
#24355=CARTESIAN_POINT('Ctrl Pts',(0.585373918990895,-1.,-2.086169437277));
#24356=CARTESIAN_POINT('Ctrl Pts',(0.589962365403189,-1.,-2.09064881812053));
#24357=CARTESIAN_POINT('Ctrl Pts',(0.594585006052823,-1.,-2.09510876220501));
#24358=CARTESIAN_POINT('Ctrl Pts',(0.599241616422144,-1.,-2.09954930865331));
#24359=CARTESIAN_POINT('Ctrl Pts',(0.603932030738212,-1.,-2.10397049887709));
#24360=CARTESIAN_POINT('Ctrl Pts',(0.607711315456826,-1.,-2.10749199615859));
#24361=CARTESIAN_POINT('Ctrl Pts',(0.610560911691113,-1.,-2.11012443807661));
#24362=CARTESIAN_POINT('Ctrl Pts',(0.61246736556225,-1.,-2.11187554260142));
#24363=CARTESIAN_POINT('Ctrl Pts',(0.61342227326009,-1.,-2.11275013067528));
#24364=CARTESIAN_POINT('',(0.745574324794401,-1.,-2.0698113262342));
#24365=CARTESIAN_POINT('',(0.61342227326009,-1.,-2.11275013067528));
#24366=CARTESIAN_POINT('',(0.693717979106306,-1.,-1.60662857109684));
#24367=CARTESIAN_POINT('Ctrl Pts',(0.745574324794401,-1.,-2.0698113262342));
#24368=CARTESIAN_POINT('Ctrl Pts',(0.74583279137781,-1.,-2.06854248895575));
#24369=CARTESIAN_POINT('Ctrl Pts',(0.746345871542695,-1.,-2.06600523016401));
#24370=CARTESIAN_POINT('Ctrl Pts',(0.747103932785504,-1.,-2.06220058927162));
#24371=CARTESIAN_POINT('Ctrl Pts',(0.748091554181101,-1.,-2.05713023030263));
#24372=CARTESIAN_POINT('Ctrl Pts',(0.749287468663053,-1.,-2.05079645591606));
#24373=CARTESIAN_POINT('Ctrl Pts',(0.750444657874758,-1.,-2.04446689147754));
#24374=CARTESIAN_POINT('Ctrl Pts',(0.751562963361383,-1.,-2.03814160092173));
#24375=CARTESIAN_POINT('Ctrl Pts',(0.752642180488104,-1.,-2.03182068456467));
#24376=CARTESIAN_POINT('Ctrl Pts',(0.753682061113765,-1.,-2.02550428623587));
#24377=CARTESIAN_POINT('Ctrl Pts',(0.75468233072352,-1.,-2.01919259406003));
#24378=CARTESIAN_POINT('Ctrl Pts',(0.7556427049581,-1.,-2.01288584328149));
#24379=CARTESIAN_POINT('Ctrl Pts',(0.756562904646496,-1.,-2.00658431587682));
#24380=CARTESIAN_POINT('Ctrl Pts',(0.757442676862341,-1.,-2.00028834739072));
#24381=CARTESIAN_POINT('Ctrl Pts',(0.758281796766377,-1.,-1.9939983109871));
#24382=CARTESIAN_POINT('Ctrl Pts',(0.759080037802242,-1.,-1.98771456680806));
#24383=CARTESIAN_POINT('Ctrl Pts',(0.759837147452135,-1.,-1.98143741418156));
#24384=CARTESIAN_POINT('Ctrl Pts',(0.760552825409855,-1.,-1.97516705321521));
#24385=CARTESIAN_POINT('Ctrl Pts',(0.761226690483986,-1.,-1.96890351582545));
#24386=CARTESIAN_POINT('Ctrl Pts',(0.761858300014575,-1.,-1.96264672744229));
#24387=CARTESIAN_POINT('Ctrl Pts',(0.762447203806263,-1.,-1.95639665309893));
#24388=CARTESIAN_POINT('Ctrl Pts',(0.762992990878774,-1.,-1.95015342590025));
#24389=CARTESIAN_POINT('Ctrl Pts',(0.76349533353858,-1.,-1.94391746617626));
#24390=CARTESIAN_POINT('Ctrl Pts',(0.763954049121393,-1.,-1.93768964875867));
#24391=CARTESIAN_POINT('Ctrl Pts',(0.764369010673889,-1.,-1.93147105496367));
#24392=CARTESIAN_POINT('Ctrl Pts',(0.764740025488189,-1.,-1.92526263537041));
#24393=CARTESIAN_POINT('Ctrl Pts',(0.765066729667095,-1.,-1.91906491634197));
#24394=CARTESIAN_POINT('Ctrl Pts',(0.765348465884739,-1.,-1.91287765805174));
#24395=CARTESIAN_POINT('Ctrl Pts',(0.765584196937936,-1.,-1.90669961402362));
#24396=CARTESIAN_POINT('Ctrl Pts',(0.765772772593395,-1.,-1.90052930393599));
#24397=CARTESIAN_POINT('Ctrl Pts',(0.765913193856979,-1.,-1.89436577771389));
#24398=CARTESIAN_POINT('Ctrl Pts',(0.76600483706209,-1.,-1.88820926433409));
#24399=CARTESIAN_POINT('Ctrl Pts',(0.766047794851868,-1.,-1.88206215302561));
#24400=CARTESIAN_POINT('Ctrl Pts',(0.766042837036759,-1.,-1.87592888967886));
#24401=CARTESIAN_POINT('Ctrl Pts',(0.765990708546111,-1.,-1.86981398314345));
#24402=CARTESIAN_POINT('Ctrl Pts',(0.765891519092557,-1.,-1.86372027063315));
#24403=CARTESIAN_POINT('Ctrl Pts',(0.765744212909305,-1.,-1.85764741390391));
#24404=CARTESIAN_POINT('Ctrl Pts',(0.765545710619023,-1.,-1.85158945130054));
#24405=CARTESIAN_POINT('Ctrl Pts',(0.765291664861971,-1.,-1.84553698875911));
#24406=CARTESIAN_POINT('Ctrl Pts',(0.764978057881687,-1.,-1.83948181064823));
#24407=CARTESIAN_POINT('Ctrl Pts',(0.764602549687845,-1.,-1.8334207722714));
#24408=CARTESIAN_POINT('Ctrl Pts',(0.764165902606055,-1.,-1.8273599120008));
#24409=CARTESIAN_POINT('Ctrl Pts',(0.763673465462854,-1.,-1.82131873145297));
#24410=CARTESIAN_POINT('Ctrl Pts',(0.763132003836783,-1.,-1.81532118405566));
#24411=CARTESIAN_POINT('Ctrl Pts',(0.762546129464036,-1.,-1.80938551463989));
#24412=CARTESIAN_POINT('Ctrl Pts',(0.761915336443515,-1.,-1.80351583877334));
#24413=CARTESIAN_POINT('Ctrl Pts',(0.761229695230359,-1.,-1.79768986997735));
#24414=CARTESIAN_POINT('Ctrl Pts',(0.760469555880425,-1.,-1.79185815610802));
#24415=CARTESIAN_POINT('Ctrl Pts',(0.759614401109868,-1.,-1.78596964884527));
#24416=CARTESIAN_POINT('Ctrl Pts',(0.75865062667738,-1.,-1.77999411220912));
#24417=CARTESIAN_POINT('Ctrl Pts',(0.757578264077238,-1.,-1.77394167108342));
#24418=CARTESIAN_POINT('Ctrl Pts',(0.756421896028403,-1.,-1.76789396003141));
#24419=CARTESIAN_POINT('Ctrl Pts',(0.755220979975262,-1.,-1.7619781724032));
#24420=CARTESIAN_POINT('Ctrl Pts',(0.75400925402848,-1.,-1.75631083600175));
#24421=CARTESIAN_POINT('Ctrl Pts',(0.752797683531377,-1.,-1.75095139468809));
#24422=CARTESIAN_POINT('Ctrl Pts',(0.751555614163629,-1.,-1.74585086852298));
#24423=CARTESIAN_POINT('Ctrl Pts',(0.75019343597954,-1.,-1.74080458266705));
#24424=CARTESIAN_POINT('Ctrl Pts',(0.748582462954854,-1.,-1.73550351679848));
#24425=CARTESIAN_POINT('Ctrl Pts',(0.746574710096436,-1.,-1.72958533647399));
#24426=CARTESIAN_POINT('Ctrl Pts',(0.744021445433764,-1.,-1.7226822991693));
#24427=CARTESIAN_POINT('Ctrl Pts',(0.740795162032087,-1.,-1.71447789751927));
#24428=CARTESIAN_POINT('Ctrl Pts',(0.736799665724771,-1.,-1.70473309006121));
#24429=CARTESIAN_POINT('Ctrl Pts',(0.731963238697195,-1.,-1.69326921975743));
#24430=CARTESIAN_POINT('Ctrl Pts',(0.726235967997433,-1.,-1.67996158455503));
#24431=CARTESIAN_POINT('Ctrl Pts',(0.719585433804282,-1.,-1.6647288055568));
#24432=CARTESIAN_POINT('Ctrl Pts',(0.711993139355394,-1.,-1.64752408832016));
#24433=CARTESIAN_POINT('Ctrl Pts',(0.705159151988319,-1.,-1.63216541664676));
#24434=CARTESIAN_POINT('Ctrl Pts',(0.699605146405088,-1.,-1.61974673472612));
#24435=CARTESIAN_POINT('Ctrl Pts',(0.695712097881194,-1.,-1.61106790958151));
#24436=CARTESIAN_POINT('Ctrl Pts',(0.693717979106306,-1.,-1.60662857109684));
#24437=CARTESIAN_POINT('',(0.892032620296855,-1.,-1.5055822144029));
#24438=CARTESIAN_POINT('Origin',(0.,-1.,0.));
#24439=CARTESIAN_POINT('',(1.23627494547115,-1.,-1.81978687191668));
#24440=CARTESIAN_POINT('Ctrl Pts',(0.892032620296855,-1.,-1.5055822144029));
#24441=CARTESIAN_POINT('Ctrl Pts',(0.894452006964543,-1.,-1.50980486806688));
#24442=CARTESIAN_POINT('Ctrl Pts',(0.89918504748351,-1.,-1.51805569590094));
#24443=CARTESIAN_POINT('Ctrl Pts',(0.905967409625651,-1.,-1.52984849887993));
#24444=CARTESIAN_POINT('Ctrl Pts',(0.914375919026456,-1.,-1.54440491149498));
#24445=CARTESIAN_POINT('Ctrl Pts',(0.923832188944341,-1.,-1.56065988578893));
#24446=CARTESIAN_POINT('Ctrl Pts',(0.932246680108685,-1.,-1.57499388382243));
#24447=CARTESIAN_POINT('Ctrl Pts',(0.939646377893399,-1.,-1.58744937487176));
#24448=CARTESIAN_POINT('Ctrl Pts',(0.946078063315257,-1.,-1.59810042043673));
#24449=CARTESIAN_POINT('Ctrl Pts',(0.951613284356035,-1.,-1.60706069896936));
#24450=CARTESIAN_POINT('Ctrl Pts',(0.95635442292067,-1.,-1.61449324337085));
#24451=CARTESIAN_POINT('Ctrl Pts',(0.960438326101728,-1.,-1.62061638140221));
#24452=CARTESIAN_POINT('Ctrl Pts',(0.964046107040535,-1.,-1.62571930670187));
#24453=CARTESIAN_POINT('Ctrl Pts',(0.967387853230345,-1.,-1.63013849959462));
#24454=CARTESIAN_POINT('Ctrl Pts',(0.970669715997509,-1.,-1.63420665729798));
#24455=CARTESIAN_POINT('Ctrl Pts',(0.974066058287418,-1.,-1.63820952658144));
#24456=CARTESIAN_POINT('Ctrl Pts',(0.977689794119416,-1.,-1.64233990826687));
#24457=CARTESIAN_POINT('Ctrl Pts',(0.981562530939489,-1.,-1.64665139190656));
#24458=CARTESIAN_POINT('Ctrl Pts',(0.98564262292082,-1.,-1.65110016612638));
#24459=CARTESIAN_POINT('Ctrl Pts',(0.989855627854164,-1.,-1.65559044289699));
#24460=CARTESIAN_POINT('Ctrl Pts',(0.994121836661305,-1.,-1.66001553809947));
#24461=CARTESIAN_POINT('Ctrl Pts',(0.998389654952757,-1.,-1.66430758030376));
#24462=CARTESIAN_POINT('Ctrl Pts',(1.00265091003727,-1.,-1.66846059277303));
#24463=CARTESIAN_POINT('Ctrl Pts',(1.00692206696414,-1.,-1.67250335383293));
#24464=CARTESIAN_POINT('Ctrl Pts',(1.01123236493511,-1.,-1.67648246776464));
#24465=CARTESIAN_POINT('Ctrl Pts',(1.01561026162773,-1.,-1.68044289894798));
#24466=CARTESIAN_POINT('Ctrl Pts',(1.02006795074201,-1.,-1.68440578021706));
#24467=CARTESIAN_POINT('Ctrl Pts',(1.02460180535255,-1.,-1.68836910178447));
#24468=CARTESIAN_POINT('Ctrl Pts',(1.02919977579147,-1.,-1.69231840863458));
#24469=CARTESIAN_POINT('Ctrl Pts',(1.03384646003588,-1.,-1.69623414782771));
#24470=CARTESIAN_POINT('Ctrl Pts',(1.03852922490789,-1.,-1.70010052930962));
#24471=CARTESIAN_POINT('Ctrl Pts',(1.04324363334554,-1.,-1.70391338707982));
#24472=CARTESIAN_POINT('Ctrl Pts',(1.04799085404995,-1.,-1.70767646263649));
#24473=CARTESIAN_POINT('Ctrl Pts',(1.05277517202855,-1.,-1.71139783543989));
#24474=CARTESIAN_POINT('Ctrl Pts',(1.05760163192479,-1.,-1.7150865442702));
#24475=CARTESIAN_POINT('Ctrl Pts',(1.06247324680647,-1.,-1.71874858456904));
#24476=CARTESIAN_POINT('Ctrl Pts',(1.06738966975462,-1.,-1.72238500928453));
#24477=CARTESIAN_POINT('Ctrl Pts',(1.07234866990252,-1.,-1.72599406198488));
#24478=CARTESIAN_POINT('Ctrl Pts',(1.0773470373727,-1.,-1.72957248977424));
#24479=CARTESIAN_POINT('Ctrl Pts',(1.08238162784749,-1.,-1.73311705663407));
#24480=CARTESIAN_POINT('Ctrl Pts',(1.08745056285427,-1.,-1.73662628326091));
#24481=CARTESIAN_POINT('Ctrl Pts',(1.09255329056493,-1.,-1.74010053962247));
#24482=CARTESIAN_POINT('Ctrl Pts',(1.09768999241225,-1.,-1.74354119236208));
#24483=CARTESIAN_POINT('Ctrl Pts',(1.10286118991143,-1.,-1.74695004214923));
#24484=CARTESIAN_POINT('Ctrl Pts',(1.10806728183007,-1.,-1.7503286607592));
#24485=CARTESIAN_POINT('Ctrl Pts',(1.11330807582551,-1.,-1.7536777209463));
#24486=CARTESIAN_POINT('Ctrl Pts',(1.11858293216763,-1.,-1.75699720772105));
#24487=CARTESIAN_POINT('Ctrl Pts',(1.12389096855086,-1.,-1.76028671825096));
#24488=CARTESIAN_POINT('Ctrl Pts',(1.12923123555075,-1.,-1.7635457196617));
#24489=CARTESIAN_POINT('Ctrl Pts',(1.1346029180462,-1.,-1.76677384551862));
#24490=CARTESIAN_POINT('Ctrl Pts',(1.14000548336975,-1.,-1.76997111386769));
#24491=CARTESIAN_POINT('Ctrl Pts',(1.1454385822692,-1.,-1.77313777896194));
#24492=CARTESIAN_POINT('Ctrl Pts',(1.15090197841514,-1.,-1.7762742255701));
#24493=CARTESIAN_POINT('Ctrl Pts',(1.15639547194698,-1.,-1.77938085564275));
#24494=CARTESIAN_POINT('Ctrl Pts',(1.16191881298499,-1.,-1.78245795881009));
#24495=CARTESIAN_POINT('Ctrl Pts',(1.16747166312303,-1.,-1.78550566040443));
#24496=CARTESIAN_POINT('Ctrl Pts',(1.17305363177328,-1.,-1.78852398877617));
#24497=CARTESIAN_POINT('Ctrl Pts',(1.17866429440809,-1.,-1.79151291552689));
#24498=CARTESIAN_POINT('Ctrl Pts',(1.18430321697432,-1.,-1.79447240321515));
#24499=CARTESIAN_POINT('Ctrl Pts',(1.18996997934445,-1.,-1.79740245923478));
#24500=CARTESIAN_POINT('Ctrl Pts',(1.19566418930242,-1.,-1.80030314369879));
#24501=CARTESIAN_POINT('Ctrl Pts',(1.20138548938974,-1.,-1.80317454838603));
#24502=CARTESIAN_POINT('Ctrl Pts',(1.20713356605475,-1.,-1.80601678480707));
#24503=CARTESIAN_POINT('Ctrl Pts',(1.21290815708314,-1.,-1.80882996917129));
#24504=CARTESIAN_POINT('Ctrl Pts',(1.21870906103557,-1.,-1.81161420806656));
#24505=CARTESIAN_POINT('Ctrl Pts',(1.2245361330495,-1.,-1.81436959210434));
#24506=CARTESIAN_POINT('Ctrl Pts',(1.2292186489137,-1.,-1.8165508718364));
#24507=CARTESIAN_POINT('Ctrl Pts',(1.2327422452705,-1.,-1.81817389921279));
#24508=CARTESIAN_POINT('Ctrl Pts',(1.23509651170476,-1.,-1.81925017193666));
#24509=CARTESIAN_POINT('Ctrl Pts',(1.23627494547115,-1.,-1.81978687191668));
#24510=CARTESIAN_POINT('',(1.34869019493419,-1.,-1.73811241238545));
#24511=CARTESIAN_POINT('',(1.23627494547115,-1.,-1.81978687191668));
#24512=CARTESIAN_POINT('',(1.15624053661742,-1.,-1.31362392696032));
#24513=CARTESIAN_POINT('Ctrl Pts',(1.34869019493419,-1.,-1.73811241238545));
#24514=CARTESIAN_POINT('Ctrl Pts',(1.34854391898045,-1.,-1.73682580585691));
#24515=CARTESIAN_POINT('Ctrl Pts',(1.34824783112887,-1.,-1.73425417885907));
#24516=CARTESIAN_POINT('Ctrl Pts',(1.34779309152035,-1.,-1.7304014965394));
#24517=CARTESIAN_POINT('Ctrl Pts',(1.34716554819527,-1.,-1.72527410680674));
#24518=CARTESIAN_POINT('Ctrl Pts',(1.34634568653227,-1.,-1.7188807715049));
#24519=CARTESIAN_POINT('Ctrl Pts',(1.34549029589416,-1.,-1.71250340686822));
#24520=CARTESIAN_POINT('Ctrl Pts',(1.34459924533831,-1.,-1.70614212266738));
#24521=CARTESIAN_POINT('Ctrl Pts',(1.34367237124483,-1.,-1.69979707754427));
#24522=CARTESIAN_POINT('Ctrl Pts',(1.34270948206319,-1.,-1.6934684849687));
#24523=CARTESIAN_POINT('Ctrl Pts',(1.341710374848,-1.,-1.68715660868764));
#24524=CARTESIAN_POINT('Ctrl Pts',(1.34067485185203,-1.,-1.68086176030362));
#24525=CARTESIAN_POINT('Ctrl Pts',(1.3396027347034,-1.,-1.67458429426086));
#24526=CARTESIAN_POINT('Ctrl Pts',(1.33849388654388,-1.,-1.66832460783989));
#24527=CARTESIAN_POINT('Ctrl Pts',(1.33734820885262,-1.,-1.66208312541983));
#24528=CARTESIAN_POINT('Ctrl Pts',(1.33616559745172,-1.,-1.65586025952593));
#24529=CARTESIAN_POINT('Ctrl Pts',(1.33494590467993,-1.,-1.6496563728683));
#24530=CARTESIAN_POINT('Ctrl Pts',(1.33368890676572,-1.,-1.6434717485603));
#24531=CARTESIAN_POINT('Ctrl Pts',(1.33239425103724,-1.,-1.63730653475089));
#24532=CARTESIAN_POINT('Ctrl Pts',(1.33106149345645,-1.,-1.63116079730923));
#24533=CARTESIAN_POINT('Ctrl Pts',(1.3296901950568,-1.,-1.62503464209797));
#24534=CARTESIAN_POINT('Ctrl Pts',(1.32828000610449,-1.,-1.61892832270724));
#24535=CARTESIAN_POINT('Ctrl Pts',(1.32683074483356,-1.,-1.6128423401575));
#24536=CARTESIAN_POINT('Ctrl Pts',(1.32534250785782,-1.,-1.60677758290954));
#24537=CARTESIAN_POINT('Ctrl Pts',(1.32381550858256,-1.,-1.60073511858687));
#24538=CARTESIAN_POINT('Ctrl Pts',(1.32224985747682,-1.,-1.59471591079403));
#24539=CARTESIAN_POINT('Ctrl Pts',(1.32064537110892,-1.,-1.58872057258245));
#24540=CARTESIAN_POINT('Ctrl Pts',(1.31900135021432,-1.,-1.58274907898834));
#24541=CARTESIAN_POINT('Ctrl Pts',(1.31731642317187,-1.,-1.5768005650559));
#24542=CARTESIAN_POINT('Ctrl Pts',(1.31558903860016,-1.,-1.57087397835723));
#24543=CARTESIAN_POINT('Ctrl Pts',(1.31381795281002,-1.,-1.56496872402353));
#24544=CARTESIAN_POINT('Ctrl Pts',(1.31200264341696,-1.,-1.55908521254821));
#24545=CARTESIAN_POINT('Ctrl Pts',(1.31014393684222,-1.,-1.55322568759481));
#24546=CARTESIAN_POINT('Ctrl Pts',(1.30824393907473,-1.,-1.54739413957185));
#24547=CARTESIAN_POINT('Ctrl Pts',(1.30630475189556,-1.,-1.54159462645432));
#24548=CARTESIAN_POINT('Ctrl Pts',(1.30432735639489,-1.,-1.53582981268977));
#24549=CARTESIAN_POINT('Ctrl Pts',(1.30231064395568,-1.,-1.53009970283891));
#24550=CARTESIAN_POINT('Ctrl Pts',(1.30024984366328,-1.,-1.52439957861062));
#24551=CARTESIAN_POINT('Ctrl Pts',(1.29813791800747,-1.,-1.51872184912724));
#24552=CARTESIAN_POINT('Ctrl Pts',(1.29596850710509,-1.,-1.51305994241402));
#24553=CARTESIAN_POINT('Ctrl Pts',(1.29373841372842,-1.,-1.50741159078365));
#24554=CARTESIAN_POINT('Ctrl Pts',(1.29145022885181,-1.,-1.50178230149776));
#24555=CARTESIAN_POINT('Ctrl Pts',(1.28911506584254,-1.,-1.49618896881754));
#24556=CARTESIAN_POINT('Ctrl Pts',(1.2867467611644,-1.,-1.4906522831278));
#24557=CARTESIAN_POINT('Ctrl Pts',(1.28435533880201,-1.,-1.4851881711891));
#24558=CARTESIAN_POINT('Ctrl Pts',(1.28194158939517,-1.,-1.47980070347096));
#24559=CARTESIAN_POINT('Ctrl Pts',(1.2794891824849,-1.,-1.4744717526707));
#24560=CARTESIAN_POINT('Ctrl Pts',(1.27696414831089,-1.,-1.46916035917133));
#24561=CARTESIAN_POINT('Ctrl Pts',(1.27433119897822,-1.,-1.46382431332476));
#24562=CARTESIAN_POINT('Ctrl Pts',(1.27156805265289,-1.,-1.45843906294697));
#24563=CARTESIAN_POINT('Ctrl Pts',(1.2686778680489,-1.,-1.45301422764247));
#24564=CARTESIAN_POINT('Ctrl Pts',(1.26570925118868,-1.,-1.44761985001662));
#24565=CARTESIAN_POINT('Ctrl Pts',(1.26273903323858,-1.,-1.44236470511303));
#24566=CARTESIAN_POINT('Ctrl Pts',(1.25983531012005,-1.,-1.43734919180848));
#24567=CARTESIAN_POINT('Ctrl Pts',(1.25702687965755,-1.,-1.43262645609691));
#24568=CARTESIAN_POINT('Ctrl Pts',(1.25426945222639,-1.,-1.42815938799387));
#24569=CARTESIAN_POINT('Ctrl Pts',(1.2514145557001,-1.,-1.42378102115575));
#24570=CARTESIAN_POINT('Ctrl Pts',(1.24824430986571,-1.,-1.41923722596025));
#24571=CARTESIAN_POINT('Ctrl Pts',(1.24450600513056,-1.,-1.41422913175179));
#24572=CARTESIAN_POINT('Ctrl Pts',(1.23994455029534,-1.,-1.40845295531283));
#24573=CARTESIAN_POINT('Ctrl Pts',(1.23434087290423,-1.,-1.40164708206106));
#24574=CARTESIAN_POINT('Ctrl Pts',(1.22752961899387,-1.,-1.39361389568796));
#24575=CARTESIAN_POINT('Ctrl Pts',(1.21938737280852,-1.,-1.38420564527715));
#24576=CARTESIAN_POINT('Ctrl Pts',(1.20982812925645,-1.,-1.37331915607905));
#24577=CARTESIAN_POINT('Ctrl Pts',(1.1987959077932,-1.,-1.36088705043885));
#24578=CARTESIAN_POINT('Ctrl Pts',(1.18625865667441,-1.,-1.34687054001093));
#24579=CARTESIAN_POINT('Ctrl Pts',(1.17501305789857,-1.,-1.33437539347008));
#24580=CARTESIAN_POINT('Ctrl Pts',(1.16589330093588,-1.,-1.32428080721772));
#24581=CARTESIAN_POINT('Ctrl Pts',(1.15950888730809,-1.,-1.31722977216397));
#24582=CARTESIAN_POINT('Ctrl Pts',(1.15624053661742,-1.,-1.31362392696032));
#24583=CARTESIAN_POINT('',(1.31362392696032,-1.,-1.15624053661742));
#24584=CARTESIAN_POINT('Origin',(0.,-1.,0.));
#24585=CARTESIAN_POINT('',(1.73811241238545,-1.,-1.34869019493419));
#24586=CARTESIAN_POINT('Ctrl Pts',(1.31362392696032,-1.,-1.15624053661742));
#24587=CARTESIAN_POINT('Ctrl Pts',(1.3172297721596,-1.,-1.15950888730433));
#24588=CARTESIAN_POINT('Ctrl Pts',(1.32428080720544,-1.,-1.16589330092532));
#24589=CARTESIAN_POINT('Ctrl Pts',(1.33437539344842,-1.,-1.17501305787994));
#24590=CARTESIAN_POINT('Ctrl Pts',(1.34687053998157,-1.,-1.18625865664915));
#24591=CARTESIAN_POINT('Ctrl Pts',(1.36088705040677,-1.,-1.1987959077656));
#24592=CARTESIAN_POINT('Ctrl Pts',(1.37331915604962,-1.,-1.20982812923113));
#24593=CARTESIAN_POINT('Ctrl Pts',(1.38420564525391,-1.,-1.21938737278853));
#24594=CARTESIAN_POINT('Ctrl Pts',(1.39361389567257,-1.,-1.22752961898063));
#24595=CARTESIAN_POINT('Ctrl Pts',(1.40164708205345,-1.,-1.23434087289768));
#24596=CARTESIAN_POINT('Ctrl Pts',(1.40845295531151,-1.,-1.23994455029421));
#24597=CARTESIAN_POINT('Ctrl Pts',(1.41422913175437,-1.,-1.24450600513278));
#24598=CARTESIAN_POINT('Ctrl Pts',(1.41923722596421,-1.,-1.24824430986911));
#24599=CARTESIAN_POINT('Ctrl Pts',(1.42378102115911,-1.,-1.25141455570299));
#24600=CARTESIAN_POINT('Ctrl Pts',(1.42815938799555,-1.,-1.25426945222783));
#24601=CARTESIAN_POINT('Ctrl Pts',(1.43262645609679,-1.,-1.25702687965744));
#24602=CARTESIAN_POINT('Ctrl Pts',(1.43734919180719,-1.,-1.25983531011894));
#24603=CARTESIAN_POINT('Ctrl Pts',(1.44236470511145,-1.,-1.26273903323723));
#24604=CARTESIAN_POINT('Ctrl Pts',(1.44761985001544,-1.,-1.26570925118767));
#24605=CARTESIAN_POINT('Ctrl Pts',(1.45301422764205,-1.,-1.26867786804854));
#24606=CARTESIAN_POINT('Ctrl Pts',(1.45843906294725,-1.,-1.27156805265312));
#24607=CARTESIAN_POINT('Ctrl Pts',(1.4638243133254,-1.,-1.27433119897877));
#24608=CARTESIAN_POINT('Ctrl Pts',(1.46916035917197,-1.,-1.27696414831144));
#24609=CARTESIAN_POINT('Ctrl Pts',(1.4744717526711,-1.,-1.27948918248524));
#24610=CARTESIAN_POINT('Ctrl Pts',(1.47980070347102,-1.,-1.28194158939522));
#24611=CARTESIAN_POINT('Ctrl Pts',(1.48518817118891,-1.,-1.28435533880184));
#24612=CARTESIAN_POINT('Ctrl Pts',(1.4906522831275,-1.,-1.28674676116415));
#24613=CARTESIAN_POINT('Ctrl Pts',(1.49618896881729,-1.,-1.28911506584232));
#24614=CARTESIAN_POINT('Ctrl Pts',(1.50178230149764,-1.,-1.29145022885171));
#24615=CARTESIAN_POINT('Ctrl Pts',(1.50741159078367,-1.,-1.29373841372843));
#24616=CARTESIAN_POINT('Ctrl Pts',(1.51305994241412,-1.,-1.29596850710518));
#24617=CARTESIAN_POINT('Ctrl Pts',(1.51872184912735,-1.,-1.29813791800757));
#24618=CARTESIAN_POINT('Ctrl Pts',(1.5243995786107,-1.,-1.30024984366334));
#24619=CARTESIAN_POINT('Ctrl Pts',(1.53009970283893,-1.,-1.3023106439557));
#24620=CARTESIAN_POINT('Ctrl Pts',(1.53582981268976,-1.,-1.30432735639487));
#24621=CARTESIAN_POINT('Ctrl Pts',(1.54159462645428,-1.,-1.30630475189553));
#24622=CARTESIAN_POINT('Ctrl Pts',(1.54739413957183,-1.,-1.30824393907471));
#24623=CARTESIAN_POINT('Ctrl Pts',(1.55322568759481,-1.,-1.31014393684221));
#24624=CARTESIAN_POINT('Ctrl Pts',(1.55908521254822,-1.,-1.31200264341696));
#24625=CARTESIAN_POINT('Ctrl Pts',(1.56496872402352,-1.,-1.31381795281002));
#24626=CARTESIAN_POINT('Ctrl Pts',(1.57087397835721,-1.,-1.31558903860015));
#24627=CARTESIAN_POINT('Ctrl Pts',(1.57680056505585,-1.,-1.31731642317183));
#24628=CARTESIAN_POINT('Ctrl Pts',(1.58274907898829,-1.,-1.31900135021428));
#24629=CARTESIAN_POINT('Ctrl Pts',(1.58872057258244,-1.,-1.32064537110891));
#24630=CARTESIAN_POINT('Ctrl Pts',(1.59471591079408,-1.,-1.32224985747686));
#24631=CARTESIAN_POINT('Ctrl Pts',(1.600735118587,-1.,-1.32381550858266));
#24632=CARTESIAN_POINT('Ctrl Pts',(1.6067775829097,-1.,-1.32534250785794));
#24633=CARTESIAN_POINT('Ctrl Pts',(1.61284234015762,-1.,-1.32683074483365));
#24634=CARTESIAN_POINT('Ctrl Pts',(1.61892832270723,-1.,-1.32828000610448));
#24635=CARTESIAN_POINT('Ctrl Pts',(1.62503464209777,-1.,-1.32969019505665));
#24636=CARTESIAN_POINT('Ctrl Pts',(1.63116079730887,-1.,-1.33106149345618));
#24637=CARTESIAN_POINT('Ctrl Pts',(1.63730653475049,-1.,-1.33239425103694));
#24638=CARTESIAN_POINT('Ctrl Pts',(1.64347174856007,-1.,-1.33368890676554));
#24639=CARTESIAN_POINT('Ctrl Pts',(1.64965637286843,-1.,-1.33494590468003));
#24640=CARTESIAN_POINT('Ctrl Pts',(1.65586025952651,-1.,-1.33616559745217));
#24641=CARTESIAN_POINT('Ctrl Pts',(1.66208312542073,-1.,-1.33734820885331));
#24642=CARTESIAN_POINT('Ctrl Pts',(1.66832460784078,-1.,-1.33849388654458));
#24643=CARTESIAN_POINT('Ctrl Pts',(1.67458429426126,-1.,-1.33960273470372));
#24644=CARTESIAN_POINT('Ctrl Pts',(1.68086176030308,-1.,-1.3406748518516));
#24645=CARTESIAN_POINT('Ctrl Pts',(1.68715660868602,-1.,-1.34171037484673));
#24646=CARTESIAN_POINT('Ctrl Pts',(1.6934684849664,-1.,-1.34270948206139));
#24647=CARTESIAN_POINT('Ctrl Pts',(1.69979707754221,-1.,-1.34367237124322));
#24648=CARTESIAN_POINT('Ctrl Pts',(1.70614212266676,-1.,-1.34459924533783));
#24649=CARTESIAN_POINT('Ctrl Pts',(1.71250340687011,-1.,-1.34549029589563));
#24650=CARTESIAN_POINT('Ctrl Pts',(1.7188807715095,-1.,-1.34634568653586));
#24651=CARTESIAN_POINT('Ctrl Pts',(1.72527410681298,-1.,-1.34716554820013));
#24652=CARTESIAN_POINT('Ctrl Pts',(1.73040149654497,-1.,-1.3477930915247));
#24653=CARTESIAN_POINT('Ctrl Pts',(1.73425417886254,-1.,-1.34824783113158));
#24654=CARTESIAN_POINT('Ctrl Pts',(1.73682580585819,-1.,-1.34854391898145));
#24655=CARTESIAN_POINT('Ctrl Pts',(1.73811241238545,-1.,-1.34869019493419));
#24656=CARTESIAN_POINT('',(1.81978687191668,-1.,-1.23627494547115));
#24657=CARTESIAN_POINT('',(1.73811241238545,-1.,-1.34869019493419));
#24658=CARTESIAN_POINT('',(1.5055822144029,-1.,-0.892032620296855));
#24659=CARTESIAN_POINT('Ctrl Pts',(1.81978687191668,-1.,-1.23627494547115));
#24660=CARTESIAN_POINT('Ctrl Pts',(1.81925017193531,-1.,-1.23509651170384));
#24661=CARTESIAN_POINT('Ctrl Pts',(1.81817389920914,-1.,-1.23274224526804));
#24662=CARTESIAN_POINT('Ctrl Pts',(1.81655087183054,-1.,-1.22921864890975));
#24663=CARTESIAN_POINT('Ctrl Pts',(1.81436959209778,-1.,-1.22453613304507));
#24664=CARTESIAN_POINT('Ctrl Pts',(1.81161420806172,-1.,-1.2187090610323));
#24665=CARTESIAN_POINT('Ctrl Pts',(1.80882996916931,-1.,-1.2129081570818));
#24666=CARTESIAN_POINT('Ctrl Pts',(1.80601678480772,-1.,-1.20713356605519));
#24667=CARTESIAN_POINT('Ctrl Pts',(1.8031745483882,-1.,-1.2013854893912));
#24668=CARTESIAN_POINT('Ctrl Pts',(1.80030314370121,-1.,-1.19566418930405));
#24669=CARTESIAN_POINT('Ctrl Pts',(1.79740245923649,-1.,-1.1899699793456));
#24670=CARTESIAN_POINT('Ctrl Pts',(1.79447240321572,-1.,-1.18430321697471));
#24671=CARTESIAN_POINT('Ctrl Pts',(1.79151291552646,-1.,-1.17866429440781));
#24672=CARTESIAN_POINT('Ctrl Pts',(1.78852398877523,-1.,-1.17305363177265));
#24673=CARTESIAN_POINT('Ctrl Pts',(1.78550566040349,-1.,-1.16747166312239));
#24674=CARTESIAN_POINT('Ctrl Pts',(1.78245795880949,-1.,-1.16191881298458));
#24675=CARTESIAN_POINT('Ctrl Pts',(1.77938085564261,-1.,-1.15639547194689));
#24676=CARTESIAN_POINT('Ctrl Pts',(1.77627422557034,-1.,-1.15090197841531));
#24677=CARTESIAN_POINT('Ctrl Pts',(1.77313777896234,-1.,-1.14543858226948));
#24678=CARTESIAN_POINT('Ctrl Pts',(1.76997111386806,-1.,-1.14000548337));
#24679=CARTESIAN_POINT('Ctrl Pts',(1.76677384551883,-1.,-1.13460291804635));
#24680=CARTESIAN_POINT('Ctrl Pts',(1.76354571966171,-1.,-1.12923123555076));
#24681=CARTESIAN_POINT('Ctrl Pts',(1.76028671825084,-1.,-1.12389096855078));
#24682=CARTESIAN_POINT('Ctrl Pts',(1.75699720772089,-1.,-1.11858293216752));
#24683=CARTESIAN_POINT('Ctrl Pts',(1.75367772094617,-1.,-1.11330807582542));
#24684=CARTESIAN_POINT('Ctrl Pts',(1.75032866075914,-1.,-1.10806728183003));
#24685=CARTESIAN_POINT('Ctrl Pts',(1.74695004214924,-1.,-1.10286118991144));
#24686=CARTESIAN_POINT('Ctrl Pts',(1.74354119236212,-1.,-1.09768999241229));
#24687=CARTESIAN_POINT('Ctrl Pts',(1.74010053962252,-1.,-1.09255329056496));
#24688=CARTESIAN_POINT('Ctrl Pts',(1.73662628326093,-1.,-1.08745056285429));
#24689=CARTESIAN_POINT('Ctrl Pts',(1.73311705663407,-1.,-1.08238162784749));
#24690=CARTESIAN_POINT('Ctrl Pts',(1.72957248977424,-1.,-1.0773470373727));
#24691=CARTESIAN_POINT('Ctrl Pts',(1.72599406198489,-1.,-1.07234866990252));
#24692=CARTESIAN_POINT('Ctrl Pts',(1.72238500928456,-1.,-1.06738966975463));
#24693=CARTESIAN_POINT('Ctrl Pts',(1.71874858456908,-1.,-1.0624732468065));
#24694=CARTESIAN_POINT('Ctrl Pts',(1.71508654427022,-1.,-1.05760163192481));
#24695=CARTESIAN_POINT('Ctrl Pts',(1.71139783543986,-1.,-1.05277517202854));
#24696=CARTESIAN_POINT('Ctrl Pts',(1.70767646263641,-1.,-1.0479908540499));
#24697=CARTESIAN_POINT('Ctrl Pts',(1.70391338707969,-1.,-1.04324363334546));
#24698=CARTESIAN_POINT('Ctrl Pts',(1.70010052930951,-1.,-1.03852922490782));
#24699=CARTESIAN_POINT('Ctrl Pts',(1.69623414782769,-1.,-1.03384646003587));
#24700=CARTESIAN_POINT('Ctrl Pts',(1.69231840863471,-1.,-1.02919977579155));
#24701=CARTESIAN_POINT('Ctrl Pts',(1.68836910178475,-1.,-1.02460180535272));
#24702=CARTESIAN_POINT('Ctrl Pts',(1.68440578021739,-1.,-1.02006795074222));
#24703=CARTESIAN_POINT('Ctrl Pts',(1.6804428989482,-1.,-1.01561026162787));
#24704=CARTESIAN_POINT('Ctrl Pts',(1.67648246776457,-1.,-1.01123236493507));
#24705=CARTESIAN_POINT('Ctrl Pts',(1.67250335383248,-1.,-1.00692206696387));
#24706=CARTESIAN_POINT('Ctrl Pts',(1.66846059277231,-1.,-1.00265091003682));
#24707=CARTESIAN_POINT('Ctrl Pts',(1.66430758030304,-1.,-0.998389654952317));
#24708=CARTESIAN_POINT('Ctrl Pts',(1.66001553809916,-1.,-0.994121836661116));
#24709=CARTESIAN_POINT('Ctrl Pts',(1.65559044289746,-1.,-0.98985562785445));
#24710=CARTESIAN_POINT('Ctrl Pts',(1.6511001661277,-1.,-0.985642622921626));
#24711=CARTESIAN_POINT('Ctrl Pts',(1.64665139190834,-1.,-0.981562530940574));
#24712=CARTESIAN_POINT('Ctrl Pts',(1.64233990826831,-1.,-0.977689794120297));
#24713=CARTESIAN_POINT('Ctrl Pts',(1.63820952658157,-1.,-0.974066058287501));
#24714=CARTESIAN_POINT('Ctrl Pts',(1.63420665729609,-1.,-0.970669715996356));
#24715=CARTESIAN_POINT('Ctrl Pts',(1.63013849959083,-1.,-0.967387853228041));
#24716=CARTESIAN_POINT('Ctrl Pts',(1.6257193066974,-1.,-0.964046107037821));
#24717=CARTESIAN_POINT('Ctrl Pts',(1.62061638139929,-1.,-0.960438326099958));
#24718=CARTESIAN_POINT('Ctrl Pts',(1.61449324337233,-1.,-0.956354422921573));
#24719=CARTESIAN_POINT('Ctrl Pts',(1.60706069897794,-1.,-0.951613284361248));
#24720=CARTESIAN_POINT('Ctrl Pts',(1.59810042045408,-1.,-0.946078063325796));
#24721=CARTESIAN_POINT('Ctrl Pts',(1.58744937489796,-1.,-0.939646377909319));
#24722=CARTESIAN_POINT('Ctrl Pts',(1.57499388385561,-1.,-0.932246680128849));
#24723=CARTESIAN_POINT('Ctrl Pts',(1.56065988582509,-1.,-0.923832188966322));
#24724=CARTESIAN_POINT('Ctrl Pts',(1.54440491152807,-1.,-0.91437591904658));
#24725=CARTESIAN_POINT('Ctrl Pts',(1.52984849890434,-1.,-0.905967409640499));
#24726=CARTESIAN_POINT('Ctrl Pts',(1.51805569591479,-1.,-0.89918504749193));
#24727=CARTESIAN_POINT('Ctrl Pts',(1.50980486807181,-1.,-0.894452006967538));
#24728=CARTESIAN_POINT('Ctrl Pts',(1.5055822144029,-1.,-0.892032620296855));
#24729=CARTESIAN_POINT('',(1.60662857109684,-1.,-0.693717979106306));
#24730=CARTESIAN_POINT('Origin',(0.,-1.,0.));
#24731=CARTESIAN_POINT('',(2.0698113262342,-1.,-0.745574324794401));
#24732=CARTESIAN_POINT('Ctrl Pts',(1.60662857109684,-1.,-0.693717979106306));
#24733=CARTESIAN_POINT('Ctrl Pts',(1.61106790957619,-1.,-0.69571209787897));
#24734=CARTESIAN_POINT('Ctrl Pts',(1.61974673471117,-1.,-0.699605146398837));
#24735=CARTESIAN_POINT('Ctrl Pts',(1.6321654166204,-1.,-0.705159151977294));
#24736=CARTESIAN_POINT('Ctrl Pts',(1.64752408828442,-1.,-0.711993139340448));
#24737=CARTESIAN_POINT('Ctrl Pts',(1.66472880551777,-1.,-0.71958543378795));
#24738=CARTESIAN_POINT('Ctrl Pts',(1.67996158451922,-1.,-0.726235967982445));
#24739=CARTESIAN_POINT('Ctrl Pts',(1.69326921972915,-1.,-0.731963238685357));
#24740=CARTESIAN_POINT('Ctrl Pts',(1.70473309004249,-1.,-0.736799665716932));
#24741=CARTESIAN_POINT('Ctrl Pts',(1.71447789751001,-1.,-0.74079516202821));
#24742=CARTESIAN_POINT('Ctrl Pts',(1.72268229916769,-1.,-0.744021445433094));
#24743=CARTESIAN_POINT('Ctrl Pts',(1.72958533647714,-1.,-0.746574710097752));
#24744=CARTESIAN_POINT('Ctrl Pts',(1.7355035168033,-1.,-0.74858246295687));
#24745=CARTESIAN_POINT('Ctrl Pts',(1.74080458267114,-1.,-0.75019343598125));
#24746=CARTESIAN_POINT('Ctrl Pts',(1.74585086852502,-1.,-0.751555614164483));
#24747=CARTESIAN_POINT('Ctrl Pts',(1.75095139468794,-1.,-0.752797683531314));
#24748=CARTESIAN_POINT('Ctrl Pts',(1.75631083600019,-1.,-0.754009254027829));
#24749=CARTESIAN_POINT('Ctrl Pts',(1.76197817240128,-1.,-0.755220979974462));
#24750=CARTESIAN_POINT('Ctrl Pts',(1.76789396002998,-1.,-0.75642189602781));
#24751=CARTESIAN_POINT('Ctrl Pts',(1.77394167108292,-1.,-0.757578264077029));
#24752=CARTESIAN_POINT('Ctrl Pts',(1.77999411220945,-1.,-0.758650626677519));
#24753=CARTESIAN_POINT('Ctrl Pts',(1.78596964884604,-1.,-0.75961440111019));
#24754=CARTESIAN_POINT('Ctrl Pts',(1.7918581561088,-1.,-0.760469555880749));
#24755=CARTESIAN_POINT('Ctrl Pts',(1.79768986997783,-1.,-0.761229695230558));
#24756=CARTESIAN_POINT('Ctrl Pts',(1.80351583877342,-1.,-0.761915336443547));
#24757=CARTESIAN_POINT('Ctrl Pts',(1.80938551463965,-1.,-0.762546129463938));
#24758=CARTESIAN_POINT('Ctrl Pts',(1.8153211840553,-1.,-0.763132003836634));
#24759=CARTESIAN_POINT('Ctrl Pts',(1.82131873145266,-1.,-0.763673465462727));
#24760=CARTESIAN_POINT('Ctrl Pts',(1.82735991200065,-1.,-0.764165902605995));
#24761=CARTESIAN_POINT('Ctrl Pts',(1.83342077227142,-1.,-0.764602549687853));
#24762=CARTESIAN_POINT('Ctrl Pts',(1.83948181064835,-1.,-0.764978057881738));
#24763=CARTESIAN_POINT('Ctrl Pts',(1.84553698875924,-1.,-0.765291664862029));
#24764=CARTESIAN_POINT('Ctrl Pts',(1.85158945130063,-1.,-0.765545710619063));
#24765=CARTESIAN_POINT('Ctrl Pts',(1.85764741390394,-1.,-0.765744212909319));
#24766=CARTESIAN_POINT('Ctrl Pts',(1.86372027063312,-1.,-0.765891519092547));
#24767=CARTESIAN_POINT('Ctrl Pts',(1.86981398314341,-1.,-0.765990708546091));
#24768=CARTESIAN_POINT('Ctrl Pts',(1.87592888967883,-1.,-0.766042837036744));
#24769=CARTESIAN_POINT('Ctrl Pts',(1.88206215302561,-1.,-0.766047794851865));
#24770=CARTESIAN_POINT('Ctrl Pts',(1.88820926433409,-1.,-0.766004837062091));
#24771=CARTESIAN_POINT('Ctrl Pts',(1.89436577771388,-1.,-0.765913193856978));
#24772=CARTESIAN_POINT('Ctrl Pts',(1.90052930393596,-1.,-0.765772772593386));
#24773=CARTESIAN_POINT('Ctrl Pts',(1.90669961402356,-1.,-0.765584196937919));
#24774=CARTESIAN_POINT('Ctrl Pts',(1.91287765805169,-1.,-0.765348465884722));
#24775=CARTESIAN_POINT('Ctrl Pts',(1.91906491634196,-1.,-0.765066729667089));
#24776=CARTESIAN_POINT('Ctrl Pts',(1.92526263537048,-1.,-0.764740025488212));
#24777=CARTESIAN_POINT('Ctrl Pts',(1.93147105496382,-1.,-0.764369010673941));
#24778=CARTESIAN_POINT('Ctrl Pts',(1.93768964875886,-1.,-0.763954049121459));
#24779=CARTESIAN_POINT('Ctrl Pts',(1.9439174661764,-1.,-0.763495333538629));
#24780=CARTESIAN_POINT('Ctrl Pts',(1.95015342590024,-1.,-0.762992990878769));
#24781=CARTESIAN_POINT('Ctrl Pts',(1.95639665309869,-1.,-0.762447203806179));
#24782=CARTESIAN_POINT('Ctrl Pts',(1.96264672744186,-1.,-0.761858300014424));
#24783=CARTESIAN_POINT('Ctrl Pts',(1.96890351582499,-1.,-0.761226690483821));
#24784=CARTESIAN_POINT('Ctrl Pts',(1.97516705321494,-1.,-0.760552825409757));
#24785=CARTESIAN_POINT('Ctrl Pts',(1.98143741418172,-1.,-0.75983714745219));
#24786=CARTESIAN_POINT('Ctrl Pts',(1.98771456680874,-1.,-0.759080037802488));
#24787=CARTESIAN_POINT('Ctrl Pts',(1.99399831098817,-1.,-0.758281796766761));
#24788=CARTESIAN_POINT('Ctrl Pts',(2.00028834739178,-1.,-0.757442676862724));
#24789=CARTESIAN_POINT('Ctrl Pts',(2.0065843158773,-1.,-0.756562904646671));
#24790=CARTESIAN_POINT('Ctrl Pts',(2.01288584328084,-1.,-0.755642704957865));
#24791=CARTESIAN_POINT('Ctrl Pts',(2.01919259405809,-1.,-0.754682330722816));
#24792=CARTESIAN_POINT('Ctrl Pts',(2.02550428623313,-1.,-0.753682061112768));
#24793=CARTESIAN_POINT('Ctrl Pts',(2.03182068456221,-1.,-0.752642180487211));
#24794=CARTESIAN_POINT('Ctrl Pts',(2.03814160092099,-1.,-0.751562963361115));
#24795=CARTESIAN_POINT('Ctrl Pts',(2.04446689147979,-1.,-0.750444657875576));
#24796=CARTESIAN_POINT('Ctrl Pts',(2.05079645592154,-1.,-0.749287468665046));
#24797=CARTESIAN_POINT('Ctrl Pts',(2.05713023031006,-1.,-0.748091554183803));
#24798=CARTESIAN_POINT('Ctrl Pts',(2.06220058927826,-1.,-0.74710393278792));
#24799=CARTESIAN_POINT('Ctrl Pts',(2.06600523016815,-1.,-0.746345871544201));
#24800=CARTESIAN_POINT('Ctrl Pts',(2.06854248895728,-1.,-0.745832791378367));
#24801=CARTESIAN_POINT('Ctrl Pts',(2.0698113262342,-1.,-0.745574324794401));
#24802=CARTESIAN_POINT('',(2.11275013067528,-1.,-0.61342227326009));
#24803=CARTESIAN_POINT('',(2.0698113262342,-1.,-0.745574324794401));
#24804=CARTESIAN_POINT('',(1.7075470150345,-1.,-0.383122945602004));
#24805=CARTESIAN_POINT('Ctrl Pts',(2.11275013067528,-1.,-0.61342227326009));
#24806=CARTESIAN_POINT('Ctrl Pts',(2.11187554259986,-1.,-0.6124673655618));
#24807=CARTESIAN_POINT('Ctrl Pts',(2.11012443807238,-1.,-0.610560911689899));
#24808=CARTESIAN_POINT('Ctrl Pts',(2.1074919961518,-1.,-0.607711315454876));
#24809=CARTESIAN_POINT('Ctrl Pts',(2.10397049886949,-1.,-0.60393203073603));
#24810=CARTESIAN_POINT('Ctrl Pts',(2.0995493086477,-1.,-0.599241616420534));
#24811=CARTESIAN_POINT('Ctrl Pts',(2.0951087622027,-1.,-0.594585006052162));
#24812=CARTESIAN_POINT('Ctrl Pts',(2.09064881812129,-1.,-0.589962365403406));
#24813=CARTESIAN_POINT('Ctrl Pts',(2.08616943727951,-1.,-0.585373918991617));
#24814=CARTESIAN_POINT('Ctrl Pts',(2.08167059018418,-1.,-0.580819952108064));
#24815=CARTESIAN_POINT('Ctrl Pts',(2.07715226767559,-1.,-0.576300797416845));
#24816=CARTESIAN_POINT('Ctrl Pts',(2.07261449292824,-1.,-0.571816823242603));
#24817=CARTESIAN_POINT('Ctrl Pts',(2.06805732997334,-1.,-0.567368421181087));
#24818=CARTESIAN_POINT('Ctrl Pts',(2.06348090160589,-1.,-0.562955993082262));
#24819=CARTESIAN_POINT('Ctrl Pts',(2.05888537756462,-1.,-0.558579940185152));
#24820=CARTESIAN_POINT('Ctrl Pts',(2.05427091604413,-1.,-0.554240657463906));
#24821=CARTESIAN_POINT('Ctrl Pts',(2.04963761077958,-1.,-0.549938525150295));
#24822=CARTESIAN_POINT('Ctrl Pts',(2.04498544714588,-1.,-0.54567390381743));
#24823=CARTESIAN_POINT('Ctrl Pts',(2.04031422690527,-1.,-0.541447120615659));
#24824=CARTESIAN_POINT('Ctrl Pts',(2.03562362954037,-1.,-0.537258489833262));
#24825=CARTESIAN_POINT('Ctrl Pts',(2.03091336214426,-1.,-0.533108355132977));
#24826=CARTESIAN_POINT('Ctrl Pts',(2.0261832908329,-1.,-0.528997127241914));
#24827=CARTESIAN_POINT('Ctrl Pts',(2.02143356304698,-1.,-0.524925318333476));
#24828=CARTESIAN_POINT('Ctrl Pts',(2.01666477917286,-1.,-0.520893590399371));
#24829=CARTESIAN_POINT('Ctrl Pts',(2.01187773939242,-1.,-0.516902681728687));
#24830=CARTESIAN_POINT('Ctrl Pts',(2.00707309946949,-1.,-0.512953306961793));
#24831=CARTESIAN_POINT('Ctrl Pts',(2.00225107134734,-1.,-0.509046069886157));
#24832=CARTESIAN_POINT('Ctrl Pts',(1.99741107463572,-1.,-0.505181361323026));
#24833=CARTESIAN_POINT('Ctrl Pts',(1.99255149126155,-1.,-0.501359287727146));
#24834=CARTESIAN_POINT('Ctrl Pts',(1.98767044752932,-1.,-0.497579909545574));
#24835=CARTESIAN_POINT('Ctrl Pts',(1.98276658761821,-1.,-0.493843476541495));
#24836=CARTESIAN_POINT('Ctrl Pts',(1.97783973019229,-1.,-0.490150627860953));
#24837=CARTESIAN_POINT('Ctrl Pts',(1.97289186263272,-1.,-0.486502692907659));
#24838=CARTESIAN_POINT('Ctrl Pts',(1.96792703422362,-1.,-0.482901662120691));
#24839=CARTESIAN_POINT('Ctrl Pts',(1.96294933055943,-1.,-0.479349583074855));
#24840=CARTESIAN_POINT('Ctrl Pts',(1.95796111148177,-1.,-0.475848034683176));
#24841=CARTESIAN_POINT('Ctrl Pts',(1.95296148278133,-1.,-0.472397672264072));
#24842=CARTESIAN_POINT('Ctrl Pts',(1.94794381136514,-1.,-0.468997482913135));
#24843=CARTESIAN_POINT('Ctrl Pts',(1.9428979419619,-1.,-0.46564546202603));
#24844=CARTESIAN_POINT('Ctrl Pts',(1.93781486640821,-1.,-0.462340031009057));
#24845=CARTESIAN_POINT('Ctrl Pts',(1.93269066517934,-1.,-0.459081234547926));
#24846=CARTESIAN_POINT('Ctrl Pts',(1.92753067150476,-1.,-0.455872005174371));
#24847=CARTESIAN_POINT('Ctrl Pts',(1.92235380648502,-1.,-0.452719478359433));
#24848=CARTESIAN_POINT('Ctrl Pts',(1.91718342555755,-1.,-0.449632260106662));
#24849=CARTESIAN_POINT('Ctrl Pts',(1.9120369998112,-1.,-0.446617343485711));
#24850=CARTESIAN_POINT('Ctrl Pts',(1.90691756144898,-1.,-0.443677556849151));
#24851=CARTESIAN_POINT('Ctrl Pts',(1.90180124389086,-1.,-0.440807833704038));
#24852=CARTESIAN_POINT('Ctrl Pts',(1.89663648956466,-1.,-0.437995003948244));
#24853=CARTESIAN_POINT('Ctrl Pts',(1.89136993975504,-1.,-0.435225660963383));
#24854=CARTESIAN_POINT('Ctrl Pts',(1.88596913666793,-1.,-0.432493038548748));
#24855=CARTESIAN_POINT('Ctrl Pts',(1.88044229001832,-1.,-0.429803062482345));
#24856=CARTESIAN_POINT('Ctrl Pts',(1.87486989291484,-1.,-0.427183828519102));
#24857=CARTESIAN_POINT('Ctrl Pts',(1.86937803944323,-1.,-0.424678177291359));
#24858=CARTESIAN_POINT('Ctrl Pts',(1.86408083334028,-1.,-0.422327307418275));
#24859=CARTESIAN_POINT('Ctrl Pts',(1.85903281096686,-1.,-0.42015728797562));
#24860=CARTESIAN_POINT('Ctrl Pts',(1.85417632856234,-1.,-0.418164129143534));
#24861=CARTESIAN_POINT('Ctrl Pts',(1.84929312929882,-1.,-0.416300022038864));
#24862=CARTESIAN_POINT('Ctrl Pts',(1.8440575707371,-1.,-0.41448743825434));
#24863=CARTESIAN_POINT('Ctrl Pts',(1.83808953475839,-1.,-0.412633125322162));
#24864=CARTESIAN_POINT('Ctrl Pts',(1.83100408895216,-1.,-0.410641256301675));
#24865=CARTESIAN_POINT('Ctrl Pts',(1.8224702267854,-1.,-0.408428948108534));
#24866=CARTESIAN_POINT('Ctrl Pts',(1.81223801813988,-1.,-0.405933518411838));
#24867=CARTESIAN_POINT('Ctrl Pts',(1.80012077176221,-1.,-0.403107976170441));
#24868=CARTESIAN_POINT('Ctrl Pts',(1.78598826347533,-1.,-0.399919403783081));
#24869=CARTESIAN_POINT('Ctrl Pts',(1.7697556004756,-1.,-0.39634619612042));
#24870=CARTESIAN_POINT('Ctrl Pts',(1.75137405313962,-1.,-0.392375812294307));
#24871=CARTESIAN_POINT('Ctrl Pts',(1.7349317097561,-1.,-0.388877023509192));
#24872=CARTESIAN_POINT('Ctrl Pts',(1.72162022246158,-1.,-0.38607079032701));
#24873=CARTESIAN_POINT('Ctrl Pts',(1.71231062891958,-1.,-0.384119047315542));
#24874=CARTESIAN_POINT('Ctrl Pts',(1.7075470150345,-1.,-0.383122945602004));
#24875=CARTESIAN_POINT('',(1.74236521665491,-1.,-0.163289472382896));
#24876=CARTESIAN_POINT('Origin',(0.,-1.,0.));
#24877=CARTESIAN_POINT('',(2.19890268624765,-1.,-0.0694764450219582));
#24878=CARTESIAN_POINT('Ctrl Pts',(1.74236521665491,-1.,-0.163289472382896));
#24879=CARTESIAN_POINT('Ctrl Pts',(1.7472034950333,-1.,-0.163814161002002));
#24880=CARTESIAN_POINT('Ctrl Pts',(1.75666056638427,-1.,-0.164834765707159));
#24881=CARTESIAN_POINT('Ctrl Pts',(1.77018771684844,-1.,-0.1662793551464));
#24882=CARTESIAN_POINT('Ctrl Pts',(1.7869064998507,-1.,-0.168032772805197));
#24883=CARTESIAN_POINT('Ctrl Pts',(1.80561530629706,-1.,-0.169936923904608));
#24884=CARTESIAN_POINT('Ctrl Pts',(1.82215766811545,-1.,-0.171554770204119));
#24885=CARTESIAN_POINT('Ctrl Pts',(1.83658380527692,-1.,-0.1728894428919));
#24886=CARTESIAN_POINT('Ctrl Pts',(1.8489811319852,-1.,-0.173946627587732));
#24887=CARTESIAN_POINT('Ctrl Pts',(1.85948367088837,-1.,-0.17473525927603));
#24888=CARTESIAN_POINT('Ctrl Pts',(1.86828349694799,-1.,-0.175268337590758));
#24889=CARTESIAN_POINT('Ctrl Pts',(1.87563767773588,-1.,-0.175563480746485));
#24890=CARTESIAN_POINT('Ctrl Pts',(1.88188663145367,-1.,-0.175644148889699));
#24891=CARTESIAN_POINT('Ctrl Pts',(1.88742606273259,-1.,-0.175538155840648));
#24892=CARTESIAN_POINT('Ctrl Pts',(1.892646301985,-1.,-0.175274276190844));
#24893=CARTESIAN_POINT('Ctrl Pts',(1.89788101117132,-1.,-0.174879405091263));
#24894=CARTESIAN_POINT('Ctrl Pts',(1.90335253862834,-1.,-0.174375518661085));
#24895=CARTESIAN_POINT('Ctrl Pts',(1.90911693975267,-1.,-0.173776635257817));
#24896=CARTESIAN_POINT('Ctrl Pts',(1.91511429159527,-1.,-0.173090695383496));
#24897=CARTESIAN_POINT('Ctrl Pts',(1.9212233439798,-1.,-0.172321621259514));
#24898=CARTESIAN_POINT('Ctrl Pts',(1.92731093582036,-1.,-0.171471191532988));
#24899=CARTESIAN_POINT('Ctrl Pts',(1.93329183155539,-1.,-0.170541253116202));
#24900=CARTESIAN_POINT('Ctrl Pts',(1.93915639211581,-1.,-0.169534904817491));
#24901=CARTESIAN_POINT('Ctrl Pts',(1.94493757756931,-1.,-0.168455741607556));
#24902=CARTESIAN_POINT('Ctrl Pts',(1.95069027794294,-1.,-0.167307501784476));
#24903=CARTESIAN_POINT('Ctrl Pts',(1.9564675971873,-1.,-0.166093592002813));
#24904=CARTESIAN_POINT('Ctrl Pts',(1.96229379940136,-1.,-0.164816568920269));
#24905=CARTESIAN_POINT('Ctrl Pts',(1.96816512677967,-1.,-0.163478185457734));
#24906=CARTESIAN_POINT('Ctrl Pts',(1.97406280235188,-1.,-0.162079693556289));
#24907=CARTESIAN_POINT('Ctrl Pts',(1.97996195437559,-1.,-0.160622060784611));
#24908=CARTESIAN_POINT('Ctrl Pts',(1.98584238283292,-1.,-0.159106226437299));
#24909=CARTESIAN_POINT('Ctrl Pts',(1.99169810931908,-1.,-0.157533331459227));
#24910=CARTESIAN_POINT('Ctrl Pts',(1.99753284771497,-1.,-0.155904629548784));
#24911=CARTESIAN_POINT('Ctrl Pts',(2.00335565310543,-1.,-0.154221403049722));
#24912=CARTESIAN_POINT('Ctrl Pts',(2.00917680318424,-1.,-0.15248488362145));
#24913=CARTESIAN_POINT('Ctrl Pts',(2.01500291940238,-1.,-0.150696157673078));
#24914=CARTESIAN_POINT('Ctrl Pts',(2.02083464969894,-1.,-0.148856124775337));
#24915=CARTESIAN_POINT('Ctrl Pts',(2.02666926182017,-1.,-0.146965557332583));
#24916=CARTESIAN_POINT('Ctrl Pts',(2.03250223739942,-1.,-0.145025140186058));
#24917=CARTESIAN_POINT('Ctrl Pts',(2.03832911025912,-1.,-0.143035515058209));
#24918=CARTESIAN_POINT('Ctrl Pts',(2.04414757947916,-1.,-0.140997332152546));
#24919=CARTESIAN_POINT('Ctrl Pts',(2.04995762001328,-1.,-0.138911255368966));
#24920=CARTESIAN_POINT('Ctrl Pts',(2.05576044414264,-1.,-0.136777941218044));
#24921=CARTESIAN_POINT('Ctrl Pts',(2.06155781517842,-1.,-0.134598026192106));
#24922=CARTESIAN_POINT('Ctrl Pts',(2.06735123910326,-1.,-0.132372111547711));
#24923=CARTESIAN_POINT('Ctrl Pts',(2.07314114713063,-1.,-0.130100748328404));
#24924=CARTESIAN_POINT('Ctrl Pts',(2.07892715110987,-1.,-0.12778444527612));
#24925=CARTESIAN_POINT('Ctrl Pts',(2.08470840653643,-1.,-0.125423679412062));
#24926=CARTESIAN_POINT('Ctrl Pts',(2.09048392424825,-1.,-0.123018905621083));
#24927=CARTESIAN_POINT('Ctrl Pts',(2.0962529286773,-1.,-0.120570567965122));
#24928=CARTESIAN_POINT('Ctrl Pts',(2.102015121329,-1.,-0.118079107988356));
#24929=CARTESIAN_POINT('Ctrl Pts',(2.10777050261309,-1.,-0.115544957687927));
#24930=CARTESIAN_POINT('Ctrl Pts',(2.11351924490306,-1.,-0.112968534419737));
#24931=CARTESIAN_POINT('Ctrl Pts',(2.11926155590865,-1.,-0.110350236135025));
#24932=CARTESIAN_POINT('Ctrl Pts',(2.12499752307,-1.,-0.10769043523109));
#24933=CARTESIAN_POINT('Ctrl Pts',(2.13072704887293,-1.,-0.10498947915274));
#24934=CARTESIAN_POINT('Ctrl Pts',(2.13644992667165,-1.,-0.102247700556101));
#24935=CARTESIAN_POINT('Ctrl Pts',(2.14216588396025,-1.,-0.0994654261990917));
#24936=CARTESIAN_POINT('Ctrl Pts',(2.14787463531795,-1.,-0.096642985230546));
#24937=CARTESIAN_POINT('Ctrl Pts',(2.1535759397817,-1.,-0.0937807218867645));
#24938=CARTESIAN_POINT('Ctrl Pts',(2.15926961544516,-1.,-0.0908789888107267));
#24939=CARTESIAN_POINT('Ctrl Pts',(2.16495552645014,-1.,-0.0879381291386924));
#24940=CARTESIAN_POINT('Ctrl Pts',(2.17063357870952,-1.,-0.0849584620835374));
#24941=CARTESIAN_POINT('Ctrl Pts',(2.176303712113,-1.,-0.0819402680872767));
#24942=CARTESIAN_POINT('Ctrl Pts',(2.18196589448887,-1.,-0.0788837727685244));
#24943=CARTESIAN_POINT('Ctrl Pts',(2.1876201139953,-1.,-0.0757891465836149));
#24944=CARTESIAN_POINT('Ctrl Pts',(2.19213712013662,-1.,-0.0732830357306726));
#24945=CARTESIAN_POINT('Ctrl Pts',(2.19552129484002,-1.,-0.0713863779526155));
#24946=CARTESIAN_POINT('Ctrl Pts',(2.19777582085423,-1.,-0.0701143536325491));
#24947=CARTESIAN_POINT('Ctrl Pts',(2.19890268624765,-1.,-0.0694764450219582));
#24948=CARTESIAN_POINT('',(2.19890268624765,-1.,0.0694764450219582));
#24949=CARTESIAN_POINT('',(2.19890268624765,-1.,-0.0694764450219582));
#24950=CARTESIAN_POINT('',(1.74236521665491,-1.,0.163289472382896));
#24951=CARTESIAN_POINT('Ctrl Pts',(2.19890268624765,-1.,0.0694764450219582));
#24952=CARTESIAN_POINT('Ctrl Pts',(2.19777582085261,-1.,0.0701143536324925));
#24953=CARTESIAN_POINT('Ctrl Pts',(2.19552129483562,-1.,0.0713863779524626));
#24954=CARTESIAN_POINT('Ctrl Pts',(2.19213712012956,-1.,0.0732830357304275));
#24955=CARTESIAN_POINT('Ctrl Pts',(2.1876201139874,-1.,0.075789146583341));
#24956=CARTESIAN_POINT('Ctrl Pts',(2.18196589448304,-1.,0.0788837727683226));
#24957=CARTESIAN_POINT('Ctrl Pts',(2.1763037121106,-1.,0.0819402680871938));
#24958=CARTESIAN_POINT('Ctrl Pts',(2.17063357871031,-1.,0.0849584620835642));
#24959=CARTESIAN_POINT('Ctrl Pts',(2.16495552645275,-1.,0.0879381291387821));
#24960=CARTESIAN_POINT('Ctrl Pts',(2.15926961544808,-1.,0.0908789888108265));
#24961=CARTESIAN_POINT('Ctrl Pts',(2.15357593978377,-1.,0.0937807218868344));
#24962=CARTESIAN_POINT('Ctrl Pts',(2.14787463531864,-1.,0.0966429852305688));
#24963=CARTESIAN_POINT('Ctrl Pts',(2.14216588395974,-1.,0.0994654261990741));
#24964=CARTESIAN_POINT('Ctrl Pts',(2.13644992667052,-1.,0.102247700556063));
#24965=CARTESIAN_POINT('Ctrl Pts',(2.1307270488718,-1.,0.104989479152703));
#24966=CARTESIAN_POINT('Ctrl Pts',(2.12499752306927,-1.,0.107690435231068));
#24967=CARTESIAN_POINT('Ctrl Pts',(2.11926155590849,-1.,0.11035023613502));
#24968=CARTESIAN_POINT('Ctrl Pts',(2.11351924490335,-1.,0.112968534419746));
#24969=CARTESIAN_POINT('Ctrl Pts',(2.10777050261359,-1.,0.11554495768794));
#24970=CARTESIAN_POINT('Ctrl Pts',(2.10201512132945,-1.,0.118079107988368));
#24971=CARTESIAN_POINT('Ctrl Pts',(2.09625292867756,-1.,0.120570567965129));
#24972=CARTESIAN_POINT('Ctrl Pts',(2.09048392424826,-1.,0.123018905621083));
#24973=CARTESIAN_POINT('Ctrl Pts',(2.08470840653628,-1.,0.125423679412058));
#24974=CARTESIAN_POINT('Ctrl Pts',(2.07892715110967,-1.,0.127784445276116));
#24975=CARTESIAN_POINT('Ctrl Pts',(2.07314114713047,-1.,0.1301007483284));
#24976=CARTESIAN_POINT('Ctrl Pts',(2.06735123910319,-1.,0.132372111547709));
#24977=CARTESIAN_POINT('Ctrl Pts',(2.06155781517844,-1.,0.134598026192107));
#24978=CARTESIAN_POINT('Ctrl Pts',(2.0557604441427,-1.,0.136777941218044));
#24979=CARTESIAN_POINT('Ctrl Pts',(2.04995762001333,-1.,0.138911255368966));
#24980=CARTESIAN_POINT('Ctrl Pts',(2.04414757947919,-1.,0.140997332152545));
#24981=CARTESIAN_POINT('Ctrl Pts',(2.03832911025913,-1.,0.143035515058208));
#24982=CARTESIAN_POINT('Ctrl Pts',(2.03250223739941,-1.,0.145025140186058));
#24983=CARTESIAN_POINT('Ctrl Pts',(2.02666926182017,-1.,0.146965557332586));
#24984=CARTESIAN_POINT('Ctrl Pts',(2.02083464969897,-1.,0.148856124775342));
#24985=CARTESIAN_POINT('Ctrl Pts',(2.01500291940243,-1.,0.150696157673084));
#24986=CARTESIAN_POINT('Ctrl Pts',(2.00917680318426,-1.,0.152484883621452));
#24987=CARTESIAN_POINT('Ctrl Pts',(2.00335565310539,-1.,0.154221403049719));
#24988=CARTESIAN_POINT('Ctrl Pts',(1.99753284771487,-1.,0.155904629548774));
#24989=CARTESIAN_POINT('Ctrl Pts',(1.99169810931893,-1.,0.157533331459215));
#24990=CARTESIAN_POINT('Ctrl Pts',(1.98584238283279,-1.,0.159106226437288));
#24991=CARTESIAN_POINT('Ctrl Pts',(1.97996195437557,-1.,0.16062206078461));
#24992=CARTESIAN_POINT('Ctrl Pts',(1.97406280235204,-1.,0.162079693556302));
#24993=CARTESIAN_POINT('Ctrl Pts',(1.96816512678,-1.,0.16347818545776));
#24994=CARTESIAN_POINT('Ctrl Pts',(1.96229379940174,-1.,0.1648165689203));
#24995=CARTESIAN_POINT('Ctrl Pts',(1.95646759718755,-1.,0.166093592002832));
#24996=CARTESIAN_POINT('Ctrl Pts',(1.95069027794286,-1.,0.167307501784469));
#24997=CARTESIAN_POINT('Ctrl Pts',(1.94493757756879,-1.,0.168455741607515));
#24998=CARTESIAN_POINT('Ctrl Pts',(1.93915639211497,-1.,0.169534904817425));
#24999=CARTESIAN_POINT('Ctrl Pts',(1.93329183155455,-1.,0.170541253116136));
#25000=CARTESIAN_POINT('Ctrl Pts',(1.92731093582,-1.,0.17147119153296));
#25001=CARTESIAN_POINT('Ctrl Pts',(1.92122334398034,-1.,0.172321621259556));
#25002=CARTESIAN_POINT('Ctrl Pts',(1.91511429159681,-1.,0.173090695383619));
#25003=CARTESIAN_POINT('Ctrl Pts',(1.90911693975475,-1.,0.173776635257983));
#25004=CARTESIAN_POINT('Ctrl Pts',(1.90335253863003,-1.,0.174375518661222));
#25005=CARTESIAN_POINT('Ctrl Pts',(1.89788101117148,-1.,0.174879405091277));
#25006=CARTESIAN_POINT('Ctrl Pts',(1.89264630198279,-1.,0.175274276190664));
#25007=CARTESIAN_POINT('Ctrl Pts',(1.88742606272818,-1.,0.175538155840286));
#25008=CARTESIAN_POINT('Ctrl Pts',(1.88188663144846,-1.,0.175644148889271));
#25009=CARTESIAN_POINT('Ctrl Pts',(1.87563767773249,-1.,0.175563480746205));
#25010=CARTESIAN_POINT('Ctrl Pts',(1.86828349694972,-1.,0.1752683375909));
#25011=CARTESIAN_POINT('Ctrl Pts',(1.85948367089838,-1.,0.174735259276856));
#25012=CARTESIAN_POINT('Ctrl Pts',(1.84898113200543,-1.,0.173946627589401));
#25013=CARTESIAN_POINT('Ctrl Pts',(1.83658380530747,-1.,0.17288944289442));
#25014=CARTESIAN_POINT('Ctrl Pts',(1.82215766815414,-1.,0.171554770207306));
#25015=CARTESIAN_POINT('Ctrl Pts',(1.80561530633924,-1.,0.169936923908078));
#25016=CARTESIAN_POINT('Ctrl Pts',(1.78690649988931,-1.,0.16803277280837));
#25017=CARTESIAN_POINT('Ctrl Pts',(1.77018771687692,-1.,0.166279355148738));
#25018=CARTESIAN_POINT('Ctrl Pts',(1.75666056640041,-1.,0.164834765708484));
#25019=CARTESIAN_POINT('Ctrl Pts',(1.74720349503904,-1.,0.163814161002474));
#25020=CARTESIAN_POINT('Ctrl Pts',(1.74236521665491,-1.,0.163289472382896));
#25021=CARTESIAN_POINT('',(1.7075470150345,-1.,0.383122945602004));
#25022=CARTESIAN_POINT('Origin',(0.,-1.,0.));
#25023=CARTESIAN_POINT('',(2.11275013067528,-1.,0.613422273260091));
#25024=CARTESIAN_POINT('Ctrl Pts',(1.7075470150345,-1.,0.383122945602004));
#25025=CARTESIAN_POINT('Ctrl Pts',(1.71231062891398,-1.,0.384119047314215));
#25026=CARTESIAN_POINT('Ctrl Pts',(1.72162022244582,-1.,0.386070790323281));
#25027=CARTESIAN_POINT('Ctrl Pts',(1.73493170972829,-1.,0.388877023502615));
#25028=CARTESIAN_POINT('Ctrl Pts',(1.75137405310193,-1.,0.392375812285396));
#25029=CARTESIAN_POINT('Ctrl Pts',(1.76975560043442,-1.,0.396346196110688));
#25030=CARTESIAN_POINT('Ctrl Pts',(1.78598826343754,-1.,0.399919403774156));
#25031=CARTESIAN_POINT('Ctrl Pts',(1.80012077173238,-1.,0.403107976163396));
#25032=CARTESIAN_POINT('Ctrl Pts',(1.81223801812013,-1.,0.405933518407176));
#25033=CARTESIAN_POINT('Ctrl Pts',(1.82247022677562,-1.,0.408428948106228));
#25034=CARTESIAN_POINT('Ctrl Pts',(1.83100408895047,-1.,0.410641256301276));
#25035=CARTESIAN_POINT('Ctrl Pts',(1.8380895347617,-1.,0.412633125322945));
#25036=CARTESIAN_POINT('Ctrl Pts',(1.84405757074218,-1.,0.414487438255542));
#25037=CARTESIAN_POINT('Ctrl Pts',(1.84929312930314,-1.,0.416300022039885));
#25038=CARTESIAN_POINT('Ctrl Pts',(1.8541763285645,-1.,0.418164129144046));
#25039=CARTESIAN_POINT('Ctrl Pts',(1.8590328109667,-1.,0.420157287975583));
#25040=CARTESIAN_POINT('Ctrl Pts',(1.86408083333863,-1.,0.422327307417885));
#25041=CARTESIAN_POINT('Ctrl Pts',(1.8693780394412,-1.,0.424678177290876));
#25042=CARTESIAN_POINT('Ctrl Pts',(1.87486989291333,-1.,0.427183828518743));
#25043=CARTESIAN_POINT('Ctrl Pts',(1.88044229001778,-1.,0.429803062482217));
#25044=CARTESIAN_POINT('Ctrl Pts',(1.88596913666828,-1.,0.432493038548833));
#25045=CARTESIAN_POINT('Ctrl Pts',(1.89136993975585,-1.,0.43522566096358));
#25046=CARTESIAN_POINT('Ctrl Pts',(1.89663648956549,-1.,0.437995003948443));
#25047=CARTESIAN_POINT('Ctrl Pts',(1.90180124389137,-1.,0.440807833704161));
#25048=CARTESIAN_POINT('Ctrl Pts',(1.90691756144906,-1.,0.443677556849171));
#25049=CARTESIAN_POINT('Ctrl Pts',(1.91203699981095,-1.,0.446617343485651));
#25050=CARTESIAN_POINT('Ctrl Pts',(1.91718342555717,-1.,0.449632260106572));
#25051=CARTESIAN_POINT('Ctrl Pts',(1.9223538064847,-1.,0.452719478359356));
#25052=CARTESIAN_POINT('Ctrl Pts',(1.92753067150461,-1.,0.455872005174336));
#25053=CARTESIAN_POINT('Ctrl Pts',(1.93269066517936,-1.,0.459081234547932));
#25054=CARTESIAN_POINT('Ctrl Pts',(1.93781486640834,-1.,0.462340031009087));
#25055=CARTESIAN_POINT('Ctrl Pts',(1.94289794196205,-1.,0.465645462026065));
#25056=CARTESIAN_POINT('Ctrl Pts',(1.94794381136524,-1.,0.468997482913158));
#25057=CARTESIAN_POINT('Ctrl Pts',(1.95296148278136,-1.,0.47239767226408));
#25058=CARTESIAN_POINT('Ctrl Pts',(1.95796111148175,-1.,0.475848034683172));
#25059=CARTESIAN_POINT('Ctrl Pts',(1.96294933055938,-1.,0.479349583074846));
#25060=CARTESIAN_POINT('Ctrl Pts',(1.96792703422358,-1.,0.482901662120687));
#25061=CARTESIAN_POINT('Ctrl Pts',(1.97289186263272,-1.,0.486502692907661));
#25062=CARTESIAN_POINT('Ctrl Pts',(1.97783973019229,-1.,0.490150627860955));
#25063=CARTESIAN_POINT('Ctrl Pts',(1.9827665876182,-1.,0.493843476541493));
#25064=CARTESIAN_POINT('Ctrl Pts',(1.98767044752929,-1.,0.497579909545564));
#25065=CARTESIAN_POINT('Ctrl Pts',(1.9925514912615,-1.,0.501359287727129));
#25066=CARTESIAN_POINT('Ctrl Pts',(1.99741107463567,-1.,0.505181361323011));
#25067=CARTESIAN_POINT('Ctrl Pts',(2.00225107134733,-1.,0.509046069886152));
#25068=CARTESIAN_POINT('Ctrl Pts',(2.00707309946955,-1.,0.512953306961814));
#25069=CARTESIAN_POINT('Ctrl Pts',(2.01187773939257,-1.,0.516902681728733));
#25070=CARTESIAN_POINT('Ctrl Pts',(2.01666477917305,-1.,0.520893590399429));
#25071=CARTESIAN_POINT('Ctrl Pts',(2.02143356304712,-1.,0.524925318333519));
#25072=CARTESIAN_POINT('Ctrl Pts',(2.02618329083289,-1.,0.528997127241911));
#25073=CARTESIAN_POINT('Ctrl Pts',(2.03091336214401,-1.,0.533108355132905));
#25074=CARTESIAN_POINT('Ctrl Pts',(2.03562362953993,-1.,0.537258489833135));
#25075=CARTESIAN_POINT('Ctrl Pts',(2.0403142269048,-1.,0.54144712061552));
#25076=CARTESIAN_POINT('Ctrl Pts',(2.0449854471456,-1.,0.545673903817349));
#25077=CARTESIAN_POINT('Ctrl Pts',(2.04963761077974,-1.,0.549938525150342));
#25078=CARTESIAN_POINT('Ctrl Pts',(2.05427091604482,-1.,0.55424065746411));
#25079=CARTESIAN_POINT('Ctrl Pts',(2.05888537756571,-1.,0.558579940185468));
#25080=CARTESIAN_POINT('Ctrl Pts',(2.06348090160697,-1.,0.562955993082574));
#25081=CARTESIAN_POINT('Ctrl Pts',(2.06805732997383,-1.,0.56736842118123));
#25082=CARTESIAN_POINT('Ctrl Pts',(2.07261449292757,-1.,0.571816823242411));
#25083=CARTESIAN_POINT('Ctrl Pts',(2.07715226767361,-1.,0.576300797416275));
#25084=CARTESIAN_POINT('Ctrl Pts',(2.08167059018138,-1.,0.580819952107257));
#25085=CARTESIAN_POINT('Ctrl Pts',(2.086169437277,-1.,0.585373918990895));
#25086=CARTESIAN_POINT('Ctrl Pts',(2.09064881812053,-1.,0.58996236540319));
#25087=CARTESIAN_POINT('Ctrl Pts',(2.09510876220501,-1.,0.594585006052824));
#25088=CARTESIAN_POINT('Ctrl Pts',(2.09954930865331,-1.,0.599241616422144));
#25089=CARTESIAN_POINT('Ctrl Pts',(2.10397049887709,-1.,0.603932030738212));
#25090=CARTESIAN_POINT('Ctrl Pts',(2.10749199615859,-1.,0.607711315456826));
#25091=CARTESIAN_POINT('Ctrl Pts',(2.11012443807661,-1.,0.610560911691114));
#25092=CARTESIAN_POINT('Ctrl Pts',(2.11187554260142,-1.,0.61246736556225));
#25093=CARTESIAN_POINT('Ctrl Pts',(2.11275013067528,-1.,0.613422273260091));
#25094=CARTESIAN_POINT('',(2.0698113262342,-1.,0.745574324794401));
#25095=CARTESIAN_POINT('',(2.11275013067528,-1.,0.613422273260091));
#25096=CARTESIAN_POINT('Ctrl Pts',(2.0698113262342,-1.,0.745574324794401));
#25097=CARTESIAN_POINT('Ctrl Pts',(2.06854248895575,-1.,0.74583279137781));
#25098=CARTESIAN_POINT('Ctrl Pts',(2.06600523016401,-1.,0.746345871542696));
#25099=CARTESIAN_POINT('Ctrl Pts',(2.06220058927162,-1.,0.747103932785504));
#25100=CARTESIAN_POINT('Ctrl Pts',(2.05713023030263,-1.,0.748091554181101));
#25101=CARTESIAN_POINT('Ctrl Pts',(2.05079645591606,-1.,0.749287468663053));
#25102=CARTESIAN_POINT('Ctrl Pts',(2.04446689147754,-1.,0.750444657874758));
#25103=CARTESIAN_POINT('Ctrl Pts',(2.03814160092173,-1.,0.751562963361384));
#25104=CARTESIAN_POINT('Ctrl Pts',(2.03182068456467,-1.,0.752642180488104));
#25105=CARTESIAN_POINT('Ctrl Pts',(2.02550428623587,-1.,0.753682061113766));
#25106=CARTESIAN_POINT('Ctrl Pts',(2.01919259406003,-1.,0.75468233072352));
#25107=CARTESIAN_POINT('Ctrl Pts',(2.01288584328149,-1.,0.755642704958101));
#25108=CARTESIAN_POINT('Ctrl Pts',(2.00658431587682,-1.,0.756562904646496));
#25109=CARTESIAN_POINT('Ctrl Pts',(2.00028834739072,-1.,0.757442676862342));
#25110=CARTESIAN_POINT('Ctrl Pts',(1.9939983109871,-1.,0.758281796766377));
#25111=CARTESIAN_POINT('Ctrl Pts',(1.98771456680806,-1.,0.759080037802243));
#25112=CARTESIAN_POINT('Ctrl Pts',(1.98143741418156,-1.,0.759837147452135));
#25113=CARTESIAN_POINT('Ctrl Pts',(1.97516705321521,-1.,0.760552825409856));
#25114=CARTESIAN_POINT('Ctrl Pts',(1.96890351582545,-1.,0.761226690483986));
#25115=CARTESIAN_POINT('Ctrl Pts',(1.96264672744229,-1.,0.761858300014575));
#25116=CARTESIAN_POINT('Ctrl Pts',(1.95639665309893,-1.,0.762447203806264));
#25117=CARTESIAN_POINT('Ctrl Pts',(1.95015342590025,-1.,0.762992990878774));
#25118=CARTESIAN_POINT('Ctrl Pts',(1.94391746617626,-1.,0.763495333538581));
#25119=CARTESIAN_POINT('Ctrl Pts',(1.93768964875867,-1.,0.763954049121394));
#25120=CARTESIAN_POINT('Ctrl Pts',(1.93147105496367,-1.,0.76436901067389));
#25121=CARTESIAN_POINT('Ctrl Pts',(1.92526263537041,-1.,0.764740025488189));
#25122=CARTESIAN_POINT('Ctrl Pts',(1.91906491634197,-1.,0.765066729667095));
#25123=CARTESIAN_POINT('Ctrl Pts',(1.91287765805174,-1.,0.765348465884739));
#25124=CARTESIAN_POINT('Ctrl Pts',(1.90669961402362,-1.,0.765584196937937));
#25125=CARTESIAN_POINT('Ctrl Pts',(1.90052930393599,-1.,0.765772772593395));
#25126=CARTESIAN_POINT('Ctrl Pts',(1.89436577771389,-1.,0.765913193856979));
#25127=CARTESIAN_POINT('Ctrl Pts',(1.88820926433409,-1.,0.76600483706209));
#25128=CARTESIAN_POINT('Ctrl Pts',(1.88206215302561,-1.,0.766047794851869));
#25129=CARTESIAN_POINT('Ctrl Pts',(1.87592888967886,-1.,0.766042837036759));
#25130=CARTESIAN_POINT('Ctrl Pts',(1.86981398314345,-1.,0.765990708546112));
#25131=CARTESIAN_POINT('Ctrl Pts',(1.86372027063314,-1.,0.765891519092557));
#25132=CARTESIAN_POINT('Ctrl Pts',(1.85764741390391,-1.,0.765744212909305));
#25133=CARTESIAN_POINT('Ctrl Pts',(1.85158945130054,-1.,0.765545710619023));
#25134=CARTESIAN_POINT('Ctrl Pts',(1.8455369887591,-1.,0.765291664861972));
#25135=CARTESIAN_POINT('Ctrl Pts',(1.83948181064823,-1.,0.764978057881688));
#25136=CARTESIAN_POINT('Ctrl Pts',(1.8334207722714,-1.,0.764602549687846));
#25137=CARTESIAN_POINT('Ctrl Pts',(1.8273599120008,-1.,0.764165902606056));
#25138=CARTESIAN_POINT('Ctrl Pts',(1.82131873145297,-1.,0.763673465462854));
#25139=CARTESIAN_POINT('Ctrl Pts',(1.81532118405566,-1.,0.763132003836783));
#25140=CARTESIAN_POINT('Ctrl Pts',(1.80938551463989,-1.,0.762546129464036));
#25141=CARTESIAN_POINT('Ctrl Pts',(1.80351583877334,-1.,0.761915336443516));
#25142=CARTESIAN_POINT('Ctrl Pts',(1.79768986997735,-1.,0.761229695230359));
#25143=CARTESIAN_POINT('Ctrl Pts',(1.79185815610802,-1.,0.760469555880425));
#25144=CARTESIAN_POINT('Ctrl Pts',(1.78596964884526,-1.,0.759614401109868));
#25145=CARTESIAN_POINT('Ctrl Pts',(1.77999411220912,-1.,0.75865062667738));
#25146=CARTESIAN_POINT('Ctrl Pts',(1.77394167108342,-1.,0.757578264077238));
#25147=CARTESIAN_POINT('Ctrl Pts',(1.76789396003141,-1.,0.756421896028403));
#25148=CARTESIAN_POINT('Ctrl Pts',(1.7619781724032,-1.,0.755220979975262));
#25149=CARTESIAN_POINT('Ctrl Pts',(1.75631083600175,-1.,0.75400925402848));
#25150=CARTESIAN_POINT('Ctrl Pts',(1.75095139468809,-1.,0.752797683531377));
#25151=CARTESIAN_POINT('Ctrl Pts',(1.74585086852298,-1.,0.751555614163629));
#25152=CARTESIAN_POINT('Ctrl Pts',(1.74080458266705,-1.,0.750193435979541));
#25153=CARTESIAN_POINT('Ctrl Pts',(1.73550351679848,-1.,0.748582462954855));
#25154=CARTESIAN_POINT('Ctrl Pts',(1.72958533647399,-1.,0.746574710096437));
#25155=CARTESIAN_POINT('Ctrl Pts',(1.7226822991693,-1.,0.744021445433765));
#25156=CARTESIAN_POINT('Ctrl Pts',(1.71447789751927,-1.,0.740795162032088));
#25157=CARTESIAN_POINT('Ctrl Pts',(1.70473309006121,-1.,0.736799665724771));
#25158=CARTESIAN_POINT('Ctrl Pts',(1.69326921975743,-1.,0.731963238697195));
#25159=CARTESIAN_POINT('Ctrl Pts',(1.67996158455503,-1.,0.726235967997433));
#25160=CARTESIAN_POINT('Ctrl Pts',(1.6647288055568,-1.,0.719585433804282));
#25161=CARTESIAN_POINT('Ctrl Pts',(1.64752408832016,-1.,0.711993139355394));
#25162=CARTESIAN_POINT('Ctrl Pts',(1.63216541664676,-1.,0.705159151988319));
#25163=CARTESIAN_POINT('Ctrl Pts',(1.61974673472612,-1.,0.699605146405088));
#25164=CARTESIAN_POINT('Ctrl Pts',(1.61106790958151,-1.,0.695712097881194));
#25165=CARTESIAN_POINT('Ctrl Pts',(1.60662857109684,-1.,0.693717979106306));
#25166=CARTESIAN_POINT('Origin',(0.,-1.,0.));
#25167=CARTESIAN_POINT('Origin',(0.,0.,0.));
#25168=CARTESIAN_POINT('Origin',(0.,2.2,0.));
#25169=CARTESIAN_POINT('Origin',(0.,1.,0.));
#25170=CARTESIAN_POINT('',(-1.4,2.2,1.71450551880629E-16));
#25171=CARTESIAN_POINT('Origin',(0.,2.2,0.));
#25172=CARTESIAN_POINT('',(-1.4,1.,1.71450551880629E-16));
#25173=CARTESIAN_POINT('',(-1.4,1.,1.71450551880629E-16));
#25174=CARTESIAN_POINT('Origin',(0.,1.,0.));
#25175=CARTESIAN_POINT('Origin',(0.,2.2,0.));
#25176=CARTESIAN_POINT('Ctrl Pts',(2.11275013067528,-1.,0.613422273260091));
#25177=CARTESIAN_POINT('Ctrl Pts',(2.11275013067528,1.,0.613422273260091));
#25178=CARTESIAN_POINT('Ctrl Pts',(2.11187554260142,-1.,0.61246736556225));
#25179=CARTESIAN_POINT('Ctrl Pts',(2.11187554260142,1.,0.61246736556225));
#25180=CARTESIAN_POINT('Ctrl Pts',(2.11012443807661,-1.,0.610560911691114));
#25181=CARTESIAN_POINT('Ctrl Pts',(2.11012443807661,1.,0.610560911691114));
#25182=CARTESIAN_POINT('Ctrl Pts',(2.10749199615859,-1.,0.607711315456826));
#25183=CARTESIAN_POINT('Ctrl Pts',(2.10749199615859,1.,0.607711315456826));
#25184=CARTESIAN_POINT('Ctrl Pts',(2.10397049887709,-1.,0.603932030738212));
#25185=CARTESIAN_POINT('Ctrl Pts',(2.10397049887709,1.,0.603932030738212));
#25186=CARTESIAN_POINT('Ctrl Pts',(2.09954930865331,-1.,0.599241616422144));
#25187=CARTESIAN_POINT('Ctrl Pts',(2.09954930865331,1.,0.599241616422144));
#25188=CARTESIAN_POINT('Ctrl Pts',(2.09510876220501,-1.,0.594585006052824));
#25189=CARTESIAN_POINT('Ctrl Pts',(2.09510876220501,1.,0.594585006052824));
#25190=CARTESIAN_POINT('Ctrl Pts',(2.09064881812053,-1.,0.58996236540319));
#25191=CARTESIAN_POINT('Ctrl Pts',(2.09064881812053,1.,0.58996236540319));
#25192=CARTESIAN_POINT('Ctrl Pts',(2.086169437277,-1.,0.585373918990895));
#25193=CARTESIAN_POINT('Ctrl Pts',(2.086169437277,1.,0.585373918990895));
#25194=CARTESIAN_POINT('Ctrl Pts',(2.08167059018138,-1.,0.580819952107257));
#25195=CARTESIAN_POINT('Ctrl Pts',(2.08167059018138,1.,0.580819952107257));
#25196=CARTESIAN_POINT('Ctrl Pts',(2.07715226767361,-1.,0.576300797416275));
#25197=CARTESIAN_POINT('Ctrl Pts',(2.07715226767361,1.,0.576300797416275));
#25198=CARTESIAN_POINT('Ctrl Pts',(2.07261449292757,-1.,0.571816823242411));
#25199=CARTESIAN_POINT('Ctrl Pts',(2.07261449292757,1.,0.571816823242411));
#25200=CARTESIAN_POINT('Ctrl Pts',(2.06805732997383,-1.,0.56736842118123));
#25201=CARTESIAN_POINT('Ctrl Pts',(2.06805732997383,1.,0.56736842118123));
#25202=CARTESIAN_POINT('Ctrl Pts',(2.06348090160697,-1.,0.562955993082574));
#25203=CARTESIAN_POINT('Ctrl Pts',(2.06348090160697,1.,0.562955993082574));
#25204=CARTESIAN_POINT('Ctrl Pts',(2.05888537756571,-1.,0.558579940185468));
#25205=CARTESIAN_POINT('Ctrl Pts',(2.05888537756571,1.,0.558579940185468));
#25206=CARTESIAN_POINT('Ctrl Pts',(2.05427091604482,-1.,0.55424065746411));
#25207=CARTESIAN_POINT('Ctrl Pts',(2.05427091604482,1.,0.55424065746411));
#25208=CARTESIAN_POINT('Ctrl Pts',(2.04963761077974,-1.,0.549938525150342));
#25209=CARTESIAN_POINT('Ctrl Pts',(2.04963761077974,1.,0.549938525150342));
#25210=CARTESIAN_POINT('Ctrl Pts',(2.0449854471456,-1.,0.545673903817349));
#25211=CARTESIAN_POINT('Ctrl Pts',(2.0449854471456,1.,0.545673903817349));
#25212=CARTESIAN_POINT('Ctrl Pts',(2.0403142269048,-1.,0.54144712061552));
#25213=CARTESIAN_POINT('Ctrl Pts',(2.0403142269048,1.,0.54144712061552));
#25214=CARTESIAN_POINT('Ctrl Pts',(2.03562362953993,-1.,0.537258489833135));
#25215=CARTESIAN_POINT('Ctrl Pts',(2.03562362953993,1.,0.537258489833135));
#25216=CARTESIAN_POINT('Ctrl Pts',(2.03091336214401,-1.,0.533108355132905));
#25217=CARTESIAN_POINT('Ctrl Pts',(2.03091336214401,1.,0.533108355132905));
#25218=CARTESIAN_POINT('Ctrl Pts',(2.02618329083289,-1.,0.528997127241911));
#25219=CARTESIAN_POINT('Ctrl Pts',(2.02618329083289,1.,0.528997127241911));
#25220=CARTESIAN_POINT('Ctrl Pts',(2.02143356304712,-1.,0.524925318333519));
#25221=CARTESIAN_POINT('Ctrl Pts',(2.02143356304712,1.,0.524925318333519));
#25222=CARTESIAN_POINT('Ctrl Pts',(2.01666477917305,-1.,0.520893590399429));
#25223=CARTESIAN_POINT('Ctrl Pts',(2.01666477917305,1.,0.520893590399429));
#25224=CARTESIAN_POINT('Ctrl Pts',(2.01187773939257,-1.,0.516902681728733));
#25225=CARTESIAN_POINT('Ctrl Pts',(2.01187773939257,1.,0.516902681728733));
#25226=CARTESIAN_POINT('Ctrl Pts',(2.00707309946955,-1.,0.512953306961814));
#25227=CARTESIAN_POINT('Ctrl Pts',(2.00707309946955,1.,0.512953306961814));
#25228=CARTESIAN_POINT('Ctrl Pts',(2.00225107134733,-1.,0.509046069886152));
#25229=CARTESIAN_POINT('Ctrl Pts',(2.00225107134733,1.,0.509046069886152));
#25230=CARTESIAN_POINT('Ctrl Pts',(1.99741107463567,-1.,0.505181361323011));
#25231=CARTESIAN_POINT('Ctrl Pts',(1.99741107463567,1.,0.505181361323011));
#25232=CARTESIAN_POINT('Ctrl Pts',(1.9925514912615,-1.,0.501359287727129));
#25233=CARTESIAN_POINT('Ctrl Pts',(1.9925514912615,1.,0.501359287727129));
#25234=CARTESIAN_POINT('Ctrl Pts',(1.98767044752929,-1.,0.497579909545564));
#25235=CARTESIAN_POINT('Ctrl Pts',(1.98767044752929,1.,0.497579909545564));
#25236=CARTESIAN_POINT('Ctrl Pts',(1.9827665876182,-1.,0.493843476541493));
#25237=CARTESIAN_POINT('Ctrl Pts',(1.9827665876182,1.,0.493843476541493));
#25238=CARTESIAN_POINT('Ctrl Pts',(1.97783973019229,-1.,0.490150627860955));
#25239=CARTESIAN_POINT('Ctrl Pts',(1.97783973019229,1.,0.490150627860955));
#25240=CARTESIAN_POINT('Ctrl Pts',(1.97289186263272,-1.,0.486502692907661));
#25241=CARTESIAN_POINT('Ctrl Pts',(1.97289186263272,1.,0.486502692907661));
#25242=CARTESIAN_POINT('Ctrl Pts',(1.96792703422358,-1.,0.482901662120687));
#25243=CARTESIAN_POINT('Ctrl Pts',(1.96792703422358,1.,0.482901662120687));
#25244=CARTESIAN_POINT('Ctrl Pts',(1.96294933055938,-1.,0.479349583074846));
#25245=CARTESIAN_POINT('Ctrl Pts',(1.96294933055938,1.,0.479349583074846));
#25246=CARTESIAN_POINT('Ctrl Pts',(1.95796111148175,-1.,0.475848034683172));
#25247=CARTESIAN_POINT('Ctrl Pts',(1.95796111148175,1.,0.475848034683172));
#25248=CARTESIAN_POINT('Ctrl Pts',(1.95296148278136,-1.,0.47239767226408));
#25249=CARTESIAN_POINT('Ctrl Pts',(1.95296148278136,1.,0.47239767226408));
#25250=CARTESIAN_POINT('Ctrl Pts',(1.94794381136524,-1.,0.468997482913158));
#25251=CARTESIAN_POINT('Ctrl Pts',(1.94794381136524,1.,0.468997482913158));
#25252=CARTESIAN_POINT('Ctrl Pts',(1.94289794196205,-1.,0.465645462026065));
#25253=CARTESIAN_POINT('Ctrl Pts',(1.94289794196205,1.,0.465645462026065));
#25254=CARTESIAN_POINT('Ctrl Pts',(1.93781486640834,-1.,0.462340031009087));
#25255=CARTESIAN_POINT('Ctrl Pts',(1.93781486640834,1.,0.462340031009087));
#25256=CARTESIAN_POINT('Ctrl Pts',(1.93269066517936,-1.,0.459081234547932));
#25257=CARTESIAN_POINT('Ctrl Pts',(1.93269066517936,1.,0.459081234547932));
#25258=CARTESIAN_POINT('Ctrl Pts',(1.92753067150461,-1.,0.455872005174336));
#25259=CARTESIAN_POINT('Ctrl Pts',(1.92753067150461,1.,0.455872005174336));
#25260=CARTESIAN_POINT('Ctrl Pts',(1.9223538064847,-1.,0.452719478359356));
#25261=CARTESIAN_POINT('Ctrl Pts',(1.9223538064847,1.,0.452719478359356));
#25262=CARTESIAN_POINT('Ctrl Pts',(1.91718342555717,-1.,0.449632260106572));
#25263=CARTESIAN_POINT('Ctrl Pts',(1.91718342555717,1.,0.449632260106572));
#25264=CARTESIAN_POINT('Ctrl Pts',(1.91203699981095,-1.,0.446617343485651));
#25265=CARTESIAN_POINT('Ctrl Pts',(1.91203699981095,1.,0.446617343485651));
#25266=CARTESIAN_POINT('Ctrl Pts',(1.90691756144906,-1.,0.443677556849171));
#25267=CARTESIAN_POINT('Ctrl Pts',(1.90691756144906,1.,0.443677556849171));
#25268=CARTESIAN_POINT('Ctrl Pts',(1.90180124389137,-1.,0.440807833704161));
#25269=CARTESIAN_POINT('Ctrl Pts',(1.90180124389137,1.,0.440807833704161));
#25270=CARTESIAN_POINT('Ctrl Pts',(1.89663648956549,-1.,0.437995003948443));
#25271=CARTESIAN_POINT('Ctrl Pts',(1.89663648956549,1.,0.437995003948443));
#25272=CARTESIAN_POINT('Ctrl Pts',(1.89136993975585,-1.,0.43522566096358));
#25273=CARTESIAN_POINT('Ctrl Pts',(1.89136993975585,1.,0.43522566096358));
#25274=CARTESIAN_POINT('Ctrl Pts',(1.88596913666828,-1.,0.432493038548833));
#25275=CARTESIAN_POINT('Ctrl Pts',(1.88596913666828,1.,0.432493038548833));
#25276=CARTESIAN_POINT('Ctrl Pts',(1.88044229001778,-1.,0.429803062482217));
#25277=CARTESIAN_POINT('Ctrl Pts',(1.88044229001778,1.,0.429803062482217));
#25278=CARTESIAN_POINT('Ctrl Pts',(1.87486989291333,-1.,0.427183828518743));
#25279=CARTESIAN_POINT('Ctrl Pts',(1.87486989291333,1.,0.427183828518743));
#25280=CARTESIAN_POINT('Ctrl Pts',(1.8693780394412,-1.,0.424678177290876));
#25281=CARTESIAN_POINT('Ctrl Pts',(1.8693780394412,1.,0.424678177290876));
#25282=CARTESIAN_POINT('Ctrl Pts',(1.86408083333863,-1.,0.422327307417885));
#25283=CARTESIAN_POINT('Ctrl Pts',(1.86408083333863,1.,0.422327307417885));
#25284=CARTESIAN_POINT('Ctrl Pts',(1.8590328109667,-1.,0.420157287975583));
#25285=CARTESIAN_POINT('Ctrl Pts',(1.8590328109667,1.,0.420157287975583));
#25286=CARTESIAN_POINT('Ctrl Pts',(1.8541763285645,-1.,0.418164129144046));
#25287=CARTESIAN_POINT('Ctrl Pts',(1.8541763285645,1.,0.418164129144046));
#25288=CARTESIAN_POINT('Ctrl Pts',(1.84929312930314,-1.,0.416300022039885));
#25289=CARTESIAN_POINT('Ctrl Pts',(1.84929312930314,1.,0.416300022039885));
#25290=CARTESIAN_POINT('Ctrl Pts',(1.84405757074218,-1.,0.414487438255542));
#25291=CARTESIAN_POINT('Ctrl Pts',(1.84405757074218,1.,0.414487438255542));
#25292=CARTESIAN_POINT('Ctrl Pts',(1.8380895347617,-1.,0.412633125322945));
#25293=CARTESIAN_POINT('Ctrl Pts',(1.8380895347617,1.,0.412633125322945));
#25294=CARTESIAN_POINT('Ctrl Pts',(1.83100408895047,-1.,0.410641256301276));
#25295=CARTESIAN_POINT('Ctrl Pts',(1.83100408895047,1.,0.410641256301276));
#25296=CARTESIAN_POINT('Ctrl Pts',(1.82247022677562,-1.,0.408428948106228));
#25297=CARTESIAN_POINT('Ctrl Pts',(1.82247022677562,1.,0.408428948106228));
#25298=CARTESIAN_POINT('Ctrl Pts',(1.81223801812013,-1.,0.405933518407176));
#25299=CARTESIAN_POINT('Ctrl Pts',(1.81223801812013,1.,0.405933518407176));
#25300=CARTESIAN_POINT('Ctrl Pts',(1.80012077173238,-1.,0.403107976163396));
#25301=CARTESIAN_POINT('Ctrl Pts',(1.80012077173238,1.,0.403107976163396));
#25302=CARTESIAN_POINT('Ctrl Pts',(1.78598826343754,-1.,0.399919403774156));
#25303=CARTESIAN_POINT('Ctrl Pts',(1.78598826343754,1.,0.399919403774156));
#25304=CARTESIAN_POINT('Ctrl Pts',(1.76975560043442,-1.,0.396346196110688));
#25305=CARTESIAN_POINT('Ctrl Pts',(1.76975560043442,1.,0.396346196110688));
#25306=CARTESIAN_POINT('Ctrl Pts',(1.75137405310193,-1.,0.392375812285396));
#25307=CARTESIAN_POINT('Ctrl Pts',(1.75137405310193,1.,0.392375812285396));
#25308=CARTESIAN_POINT('Ctrl Pts',(1.73493170972829,-1.,0.388877023502615));
#25309=CARTESIAN_POINT('Ctrl Pts',(1.73493170972829,1.,0.388877023502615));
#25310=CARTESIAN_POINT('Ctrl Pts',(1.72162022244582,-1.,0.386070790323281));
#25311=CARTESIAN_POINT('Ctrl Pts',(1.72162022244582,1.,0.386070790323281));
#25312=CARTESIAN_POINT('Ctrl Pts',(1.71231062891398,-1.,0.384119047314215));
#25313=CARTESIAN_POINT('Ctrl Pts',(1.71231062891398,1.,0.384119047314215));
#25314=CARTESIAN_POINT('Ctrl Pts',(1.7075470150345,-1.,0.383122945602004));
#25315=CARTESIAN_POINT('Ctrl Pts',(1.7075470150345,1.,0.383122945602004));
#25316=CARTESIAN_POINT('',(1.7075470150345,1.,0.383122945602004));
#25317=CARTESIAN_POINT('',(1.7075470150345,0.,0.383122945602005));
#25318=CARTESIAN_POINT('',(2.11275013067528,1.,0.613422273260091));
#25319=CARTESIAN_POINT('Ctrl Pts',(2.11275013067528,1.,0.613422273260091));
#25320=CARTESIAN_POINT('Ctrl Pts',(2.11187554260142,1.,0.61246736556225));
#25321=CARTESIAN_POINT('Ctrl Pts',(2.11012443807661,1.,0.610560911691114));
#25322=CARTESIAN_POINT('Ctrl Pts',(2.10749199615859,1.,0.607711315456826));
#25323=CARTESIAN_POINT('Ctrl Pts',(2.10397049887709,1.,0.603932030738212));
#25324=CARTESIAN_POINT('Ctrl Pts',(2.09954930865331,1.,0.599241616422144));
#25325=CARTESIAN_POINT('Ctrl Pts',(2.09510876220501,1.,0.594585006052824));
#25326=CARTESIAN_POINT('Ctrl Pts',(2.09064881812053,1.,0.58996236540319));
#25327=CARTESIAN_POINT('Ctrl Pts',(2.086169437277,1.,0.585373918990895));
#25328=CARTESIAN_POINT('Ctrl Pts',(2.08167059018138,1.,0.580819952107257));
#25329=CARTESIAN_POINT('Ctrl Pts',(2.07715226767361,1.,0.576300797416275));
#25330=CARTESIAN_POINT('Ctrl Pts',(2.07261449292757,1.,0.571816823242411));
#25331=CARTESIAN_POINT('Ctrl Pts',(2.06805732997383,1.,0.56736842118123));
#25332=CARTESIAN_POINT('Ctrl Pts',(2.06348090160697,1.,0.562955993082574));
#25333=CARTESIAN_POINT('Ctrl Pts',(2.05888537756571,1.,0.558579940185468));
#25334=CARTESIAN_POINT('Ctrl Pts',(2.05427091604482,1.,0.55424065746411));
#25335=CARTESIAN_POINT('Ctrl Pts',(2.04963761077974,1.,0.549938525150342));
#25336=CARTESIAN_POINT('Ctrl Pts',(2.0449854471456,1.,0.545673903817349));
#25337=CARTESIAN_POINT('Ctrl Pts',(2.0403142269048,1.,0.54144712061552));
#25338=CARTESIAN_POINT('Ctrl Pts',(2.03562362953993,1.,0.537258489833135));
#25339=CARTESIAN_POINT('Ctrl Pts',(2.03091336214401,1.,0.533108355132905));
#25340=CARTESIAN_POINT('Ctrl Pts',(2.02618329083289,1.,0.528997127241911));
#25341=CARTESIAN_POINT('Ctrl Pts',(2.02143356304712,1.,0.524925318333519));
#25342=CARTESIAN_POINT('Ctrl Pts',(2.01666477917305,1.,0.520893590399429));
#25343=CARTESIAN_POINT('Ctrl Pts',(2.01187773939257,1.,0.516902681728733));
#25344=CARTESIAN_POINT('Ctrl Pts',(2.00707309946955,1.,0.512953306961814));
#25345=CARTESIAN_POINT('Ctrl Pts',(2.00225107134733,1.,0.509046069886152));
#25346=CARTESIAN_POINT('Ctrl Pts',(1.99741107463567,1.,0.505181361323011));
#25347=CARTESIAN_POINT('Ctrl Pts',(1.9925514912615,1.,0.501359287727129));
#25348=CARTESIAN_POINT('Ctrl Pts',(1.98767044752929,1.,0.497579909545564));
#25349=CARTESIAN_POINT('Ctrl Pts',(1.9827665876182,1.,0.493843476541493));
#25350=CARTESIAN_POINT('Ctrl Pts',(1.97783973019229,1.,0.490150627860955));
#25351=CARTESIAN_POINT('Ctrl Pts',(1.97289186263272,1.,0.486502692907661));
#25352=CARTESIAN_POINT('Ctrl Pts',(1.96792703422358,1.,0.482901662120687));
#25353=CARTESIAN_POINT('Ctrl Pts',(1.96294933055938,1.,0.479349583074846));
#25354=CARTESIAN_POINT('Ctrl Pts',(1.95796111148175,1.,0.475848034683172));
#25355=CARTESIAN_POINT('Ctrl Pts',(1.95296148278136,1.,0.47239767226408));
#25356=CARTESIAN_POINT('Ctrl Pts',(1.94794381136524,1.,0.468997482913158));
#25357=CARTESIAN_POINT('Ctrl Pts',(1.94289794196205,1.,0.465645462026065));
#25358=CARTESIAN_POINT('Ctrl Pts',(1.93781486640834,1.,0.462340031009087));
#25359=CARTESIAN_POINT('Ctrl Pts',(1.93269066517936,1.,0.459081234547932));
#25360=CARTESIAN_POINT('Ctrl Pts',(1.92753067150461,1.,0.455872005174336));
#25361=CARTESIAN_POINT('Ctrl Pts',(1.9223538064847,1.,0.452719478359356));
#25362=CARTESIAN_POINT('Ctrl Pts',(1.91718342555717,1.,0.449632260106572));
#25363=CARTESIAN_POINT('Ctrl Pts',(1.91203699981095,1.,0.446617343485651));
#25364=CARTESIAN_POINT('Ctrl Pts',(1.90691756144906,1.,0.443677556849171));
#25365=CARTESIAN_POINT('Ctrl Pts',(1.90180124389137,1.,0.440807833704161));
#25366=CARTESIAN_POINT('Ctrl Pts',(1.89663648956549,1.,0.437995003948443));
#25367=CARTESIAN_POINT('Ctrl Pts',(1.89136993975585,1.,0.43522566096358));
#25368=CARTESIAN_POINT('Ctrl Pts',(1.88596913666828,1.,0.432493038548833));
#25369=CARTESIAN_POINT('Ctrl Pts',(1.88044229001778,1.,0.429803062482217));
#25370=CARTESIAN_POINT('Ctrl Pts',(1.87486989291333,1.,0.427183828518743));
#25371=CARTESIAN_POINT('Ctrl Pts',(1.8693780394412,1.,0.424678177290876));
#25372=CARTESIAN_POINT('Ctrl Pts',(1.86408083333863,1.,0.422327307417885));
#25373=CARTESIAN_POINT('Ctrl Pts',(1.8590328109667,1.,0.420157287975583));
#25374=CARTESIAN_POINT('Ctrl Pts',(1.8541763285645,1.,0.418164129144046));
#25375=CARTESIAN_POINT('Ctrl Pts',(1.84929312930314,1.,0.416300022039885));
#25376=CARTESIAN_POINT('Ctrl Pts',(1.84405757074218,1.,0.414487438255542));
#25377=CARTESIAN_POINT('Ctrl Pts',(1.8380895347617,1.,0.412633125322945));
#25378=CARTESIAN_POINT('Ctrl Pts',(1.83100408895047,1.,0.410641256301276));
#25379=CARTESIAN_POINT('Ctrl Pts',(1.82247022677562,1.,0.408428948106228));
#25380=CARTESIAN_POINT('Ctrl Pts',(1.81223801812013,1.,0.405933518407176));
#25381=CARTESIAN_POINT('Ctrl Pts',(1.80012077173238,1.,0.403107976163396));
#25382=CARTESIAN_POINT('Ctrl Pts',(1.78598826343754,1.,0.399919403774156));
#25383=CARTESIAN_POINT('Ctrl Pts',(1.76975560043442,1.,0.396346196110688));
#25384=CARTESIAN_POINT('Ctrl Pts',(1.75137405310193,1.,0.392375812285396));
#25385=CARTESIAN_POINT('Ctrl Pts',(1.73493170972829,1.,0.388877023502615));
#25386=CARTESIAN_POINT('Ctrl Pts',(1.72162022244582,1.,0.386070790323281));
#25387=CARTESIAN_POINT('Ctrl Pts',(1.71231062891398,1.,0.384119047314215));
#25388=CARTESIAN_POINT('Ctrl Pts',(1.7075470150345,1.,0.383122945602004));
#25389=CARTESIAN_POINT('',(2.11275013067528,0.,0.613422273260091));
#25390=CARTESIAN_POINT('Origin',(2.0698113262342,0.,0.745574324794401));
#25391=CARTESIAN_POINT('',(2.0698113262342,1.,0.745574324794401));
#25392=CARTESIAN_POINT('',(2.11275013067528,1.,0.613422273260091));
#25393=CARTESIAN_POINT('',(2.0698113262342,0.,0.745574324794401));
#25394=CARTESIAN_POINT('Ctrl Pts',(1.60662857109684,-1.,0.693717979106306));
#25395=CARTESIAN_POINT('Ctrl Pts',(1.60662857109684,1.,0.693717979106306));
#25396=CARTESIAN_POINT('Ctrl Pts',(1.61106790958151,-1.,0.695712097881194));
#25397=CARTESIAN_POINT('Ctrl Pts',(1.61106790958151,1.,0.695712097881194));
#25398=CARTESIAN_POINT('Ctrl Pts',(1.61974673472612,-1.,0.699605146405088));
#25399=CARTESIAN_POINT('Ctrl Pts',(1.61974673472612,1.,0.699605146405088));
#25400=CARTESIAN_POINT('Ctrl Pts',(1.63216541664676,-1.,0.705159151988319));
#25401=CARTESIAN_POINT('Ctrl Pts',(1.63216541664676,1.,0.705159151988319));
#25402=CARTESIAN_POINT('Ctrl Pts',(1.64752408832016,-1.,0.711993139355394));
#25403=CARTESIAN_POINT('Ctrl Pts',(1.64752408832016,1.,0.711993139355394));
#25404=CARTESIAN_POINT('Ctrl Pts',(1.6647288055568,-1.,0.719585433804282));
#25405=CARTESIAN_POINT('Ctrl Pts',(1.6647288055568,1.,0.719585433804282));
#25406=CARTESIAN_POINT('Ctrl Pts',(1.67996158455503,-1.,0.726235967997433));
#25407=CARTESIAN_POINT('Ctrl Pts',(1.67996158455503,1.,0.726235967997433));
#25408=CARTESIAN_POINT('Ctrl Pts',(1.69326921975743,-1.,0.731963238697195));
#25409=CARTESIAN_POINT('Ctrl Pts',(1.69326921975743,1.,0.731963238697195));
#25410=CARTESIAN_POINT('Ctrl Pts',(1.70473309006121,-1.,0.736799665724771));
#25411=CARTESIAN_POINT('Ctrl Pts',(1.70473309006121,1.,0.736799665724771));
#25412=CARTESIAN_POINT('Ctrl Pts',(1.71447789751927,-1.,0.740795162032088));
#25413=CARTESIAN_POINT('Ctrl Pts',(1.71447789751927,1.,0.740795162032088));
#25414=CARTESIAN_POINT('Ctrl Pts',(1.7226822991693,-1.,0.744021445433765));
#25415=CARTESIAN_POINT('Ctrl Pts',(1.7226822991693,1.,0.744021445433765));
#25416=CARTESIAN_POINT('Ctrl Pts',(1.72958533647399,-1.,0.746574710096437));
#25417=CARTESIAN_POINT('Ctrl Pts',(1.72958533647399,1.,0.746574710096437));
#25418=CARTESIAN_POINT('Ctrl Pts',(1.73550351679848,-1.,0.748582462954855));
#25419=CARTESIAN_POINT('Ctrl Pts',(1.73550351679848,1.,0.748582462954855));
#25420=CARTESIAN_POINT('Ctrl Pts',(1.74080458266705,-1.,0.750193435979541));
#25421=CARTESIAN_POINT('Ctrl Pts',(1.74080458266705,1.,0.750193435979541));
#25422=CARTESIAN_POINT('Ctrl Pts',(1.74585086852298,-1.,0.751555614163629));
#25423=CARTESIAN_POINT('Ctrl Pts',(1.74585086852298,1.,0.751555614163629));
#25424=CARTESIAN_POINT('Ctrl Pts',(1.75095139468809,-1.,0.752797683531377));
#25425=CARTESIAN_POINT('Ctrl Pts',(1.75095139468809,1.,0.752797683531377));
#25426=CARTESIAN_POINT('Ctrl Pts',(1.75631083600175,-1.,0.75400925402848));
#25427=CARTESIAN_POINT('Ctrl Pts',(1.75631083600175,1.,0.75400925402848));
#25428=CARTESIAN_POINT('Ctrl Pts',(1.7619781724032,-1.,0.755220979975262));
#25429=CARTESIAN_POINT('Ctrl Pts',(1.7619781724032,1.,0.755220979975262));
#25430=CARTESIAN_POINT('Ctrl Pts',(1.76789396003141,-1.,0.756421896028403));
#25431=CARTESIAN_POINT('Ctrl Pts',(1.76789396003141,1.,0.756421896028403));
#25432=CARTESIAN_POINT('Ctrl Pts',(1.77394167108342,-1.,0.757578264077238));
#25433=CARTESIAN_POINT('Ctrl Pts',(1.77394167108342,1.,0.757578264077238));
#25434=CARTESIAN_POINT('Ctrl Pts',(1.77999411220912,-1.,0.75865062667738));
#25435=CARTESIAN_POINT('Ctrl Pts',(1.77999411220912,1.,0.75865062667738));
#25436=CARTESIAN_POINT('Ctrl Pts',(1.78596964884526,-1.,0.759614401109868));
#25437=CARTESIAN_POINT('Ctrl Pts',(1.78596964884526,1.,0.759614401109868));
#25438=CARTESIAN_POINT('Ctrl Pts',(1.79185815610802,-1.,0.760469555880425));
#25439=CARTESIAN_POINT('Ctrl Pts',(1.79185815610802,1.,0.760469555880425));
#25440=CARTESIAN_POINT('Ctrl Pts',(1.79768986997735,-1.,0.761229695230359));
#25441=CARTESIAN_POINT('Ctrl Pts',(1.79768986997735,1.,0.761229695230359));
#25442=CARTESIAN_POINT('Ctrl Pts',(1.80351583877334,-1.,0.761915336443516));
#25443=CARTESIAN_POINT('Ctrl Pts',(1.80351583877334,1.,0.761915336443516));
#25444=CARTESIAN_POINT('Ctrl Pts',(1.80938551463989,-1.,0.762546129464036));
#25445=CARTESIAN_POINT('Ctrl Pts',(1.80938551463989,1.,0.762546129464036));
#25446=CARTESIAN_POINT('Ctrl Pts',(1.81532118405566,-1.,0.763132003836783));
#25447=CARTESIAN_POINT('Ctrl Pts',(1.81532118405566,1.,0.763132003836783));
#25448=CARTESIAN_POINT('Ctrl Pts',(1.82131873145297,-1.,0.763673465462854));
#25449=CARTESIAN_POINT('Ctrl Pts',(1.82131873145297,1.,0.763673465462854));
#25450=CARTESIAN_POINT('Ctrl Pts',(1.8273599120008,-1.,0.764165902606056));
#25451=CARTESIAN_POINT('Ctrl Pts',(1.8273599120008,1.,0.764165902606056));
#25452=CARTESIAN_POINT('Ctrl Pts',(1.8334207722714,-1.,0.764602549687846));
#25453=CARTESIAN_POINT('Ctrl Pts',(1.8334207722714,1.,0.764602549687846));
#25454=CARTESIAN_POINT('Ctrl Pts',(1.83948181064823,-1.,0.764978057881688));
#25455=CARTESIAN_POINT('Ctrl Pts',(1.83948181064823,1.,0.764978057881688));
#25456=CARTESIAN_POINT('Ctrl Pts',(1.8455369887591,-1.,0.765291664861972));
#25457=CARTESIAN_POINT('Ctrl Pts',(1.8455369887591,1.,0.765291664861972));
#25458=CARTESIAN_POINT('Ctrl Pts',(1.85158945130054,-1.,0.765545710619023));
#25459=CARTESIAN_POINT('Ctrl Pts',(1.85158945130054,1.,0.765545710619023));
#25460=CARTESIAN_POINT('Ctrl Pts',(1.85764741390391,-1.,0.765744212909305));
#25461=CARTESIAN_POINT('Ctrl Pts',(1.85764741390391,1.,0.765744212909305));
#25462=CARTESIAN_POINT('Ctrl Pts',(1.86372027063314,-1.,0.765891519092557));
#25463=CARTESIAN_POINT('Ctrl Pts',(1.86372027063314,1.,0.765891519092557));
#25464=CARTESIAN_POINT('Ctrl Pts',(1.86981398314345,-1.,0.765990708546112));
#25465=CARTESIAN_POINT('Ctrl Pts',(1.86981398314345,1.,0.765990708546112));
#25466=CARTESIAN_POINT('Ctrl Pts',(1.87592888967886,-1.,0.766042837036759));
#25467=CARTESIAN_POINT('Ctrl Pts',(1.87592888967886,1.,0.766042837036759));
#25468=CARTESIAN_POINT('Ctrl Pts',(1.88206215302561,-1.,0.766047794851869));
#25469=CARTESIAN_POINT('Ctrl Pts',(1.88206215302561,1.,0.766047794851869));
#25470=CARTESIAN_POINT('Ctrl Pts',(1.88820926433409,-1.,0.76600483706209));
#25471=CARTESIAN_POINT('Ctrl Pts',(1.88820926433409,1.,0.76600483706209));
#25472=CARTESIAN_POINT('Ctrl Pts',(1.89436577771389,-1.,0.765913193856979));
#25473=CARTESIAN_POINT('Ctrl Pts',(1.89436577771389,1.,0.765913193856979));
#25474=CARTESIAN_POINT('Ctrl Pts',(1.90052930393599,-1.,0.765772772593395));
#25475=CARTESIAN_POINT('Ctrl Pts',(1.90052930393599,1.,0.765772772593395));
#25476=CARTESIAN_POINT('Ctrl Pts',(1.90669961402362,-1.,0.765584196937937));
#25477=CARTESIAN_POINT('Ctrl Pts',(1.90669961402362,1.,0.765584196937937));
#25478=CARTESIAN_POINT('Ctrl Pts',(1.91287765805174,-1.,0.765348465884739));
#25479=CARTESIAN_POINT('Ctrl Pts',(1.91287765805174,1.,0.765348465884739));
#25480=CARTESIAN_POINT('Ctrl Pts',(1.91906491634197,-1.,0.765066729667095));
#25481=CARTESIAN_POINT('Ctrl Pts',(1.91906491634197,1.,0.765066729667095));
#25482=CARTESIAN_POINT('Ctrl Pts',(1.92526263537041,-1.,0.764740025488189));
#25483=CARTESIAN_POINT('Ctrl Pts',(1.92526263537041,1.,0.764740025488189));
#25484=CARTESIAN_POINT('Ctrl Pts',(1.93147105496367,-1.,0.76436901067389));
#25485=CARTESIAN_POINT('Ctrl Pts',(1.93147105496367,1.,0.76436901067389));
#25486=CARTESIAN_POINT('Ctrl Pts',(1.93768964875867,-1.,0.763954049121394));
#25487=CARTESIAN_POINT('Ctrl Pts',(1.93768964875867,1.,0.763954049121394));
#25488=CARTESIAN_POINT('Ctrl Pts',(1.94391746617626,-1.,0.763495333538581));
#25489=CARTESIAN_POINT('Ctrl Pts',(1.94391746617626,1.,0.763495333538581));
#25490=CARTESIAN_POINT('Ctrl Pts',(1.95015342590025,-1.,0.762992990878774));
#25491=CARTESIAN_POINT('Ctrl Pts',(1.95015342590025,1.,0.762992990878774));
#25492=CARTESIAN_POINT('Ctrl Pts',(1.95639665309893,-1.,0.762447203806264));
#25493=CARTESIAN_POINT('Ctrl Pts',(1.95639665309893,1.,0.762447203806264));
#25494=CARTESIAN_POINT('Ctrl Pts',(1.96264672744229,-1.,0.761858300014575));
#25495=CARTESIAN_POINT('Ctrl Pts',(1.96264672744229,1.,0.761858300014575));
#25496=CARTESIAN_POINT('Ctrl Pts',(1.96890351582545,-1.,0.761226690483986));
#25497=CARTESIAN_POINT('Ctrl Pts',(1.96890351582545,1.,0.761226690483986));
#25498=CARTESIAN_POINT('Ctrl Pts',(1.97516705321521,-1.,0.760552825409856));
#25499=CARTESIAN_POINT('Ctrl Pts',(1.97516705321521,1.,0.760552825409856));
#25500=CARTESIAN_POINT('Ctrl Pts',(1.98143741418156,-1.,0.759837147452135));
#25501=CARTESIAN_POINT('Ctrl Pts',(1.98143741418156,1.,0.759837147452135));
#25502=CARTESIAN_POINT('Ctrl Pts',(1.98771456680806,-1.,0.759080037802243));
#25503=CARTESIAN_POINT('Ctrl Pts',(1.98771456680806,1.,0.759080037802243));
#25504=CARTESIAN_POINT('Ctrl Pts',(1.9939983109871,-1.,0.758281796766377));
#25505=CARTESIAN_POINT('Ctrl Pts',(1.9939983109871,1.,0.758281796766377));
#25506=CARTESIAN_POINT('Ctrl Pts',(2.00028834739072,-1.,0.757442676862342));
#25507=CARTESIAN_POINT('Ctrl Pts',(2.00028834739072,1.,0.757442676862342));
#25508=CARTESIAN_POINT('Ctrl Pts',(2.00658431587682,-1.,0.756562904646496));
#25509=CARTESIAN_POINT('Ctrl Pts',(2.00658431587682,1.,0.756562904646496));
#25510=CARTESIAN_POINT('Ctrl Pts',(2.01288584328149,-1.,0.755642704958101));
#25511=CARTESIAN_POINT('Ctrl Pts',(2.01288584328149,1.,0.755642704958101));
#25512=CARTESIAN_POINT('Ctrl Pts',(2.01919259406003,-1.,0.75468233072352));
#25513=CARTESIAN_POINT('Ctrl Pts',(2.01919259406003,1.,0.75468233072352));
#25514=CARTESIAN_POINT('Ctrl Pts',(2.02550428623587,-1.,0.753682061113766));
#25515=CARTESIAN_POINT('Ctrl Pts',(2.02550428623587,1.,0.753682061113766));
#25516=CARTESIAN_POINT('Ctrl Pts',(2.03182068456467,-1.,0.752642180488104));
#25517=CARTESIAN_POINT('Ctrl Pts',(2.03182068456467,1.,0.752642180488104));
#25518=CARTESIAN_POINT('Ctrl Pts',(2.03814160092173,-1.,0.751562963361384));
#25519=CARTESIAN_POINT('Ctrl Pts',(2.03814160092173,1.,0.751562963361384));
#25520=CARTESIAN_POINT('Ctrl Pts',(2.04446689147754,-1.,0.750444657874758));
#25521=CARTESIAN_POINT('Ctrl Pts',(2.04446689147754,1.,0.750444657874758));
#25522=CARTESIAN_POINT('Ctrl Pts',(2.05079645591606,-1.,0.749287468663053));
#25523=CARTESIAN_POINT('Ctrl Pts',(2.05079645591606,1.,0.749287468663053));
#25524=CARTESIAN_POINT('Ctrl Pts',(2.05713023030263,-1.,0.748091554181101));
#25525=CARTESIAN_POINT('Ctrl Pts',(2.05713023030263,1.,0.748091554181101));
#25526=CARTESIAN_POINT('Ctrl Pts',(2.06220058927162,-1.,0.747103932785504));
#25527=CARTESIAN_POINT('Ctrl Pts',(2.06220058927162,1.,0.747103932785504));
#25528=CARTESIAN_POINT('Ctrl Pts',(2.06600523016401,-1.,0.746345871542696));
#25529=CARTESIAN_POINT('Ctrl Pts',(2.06600523016401,1.,0.746345871542696));
#25530=CARTESIAN_POINT('Ctrl Pts',(2.06854248895575,-1.,0.74583279137781));
#25531=CARTESIAN_POINT('Ctrl Pts',(2.06854248895575,1.,0.74583279137781));
#25532=CARTESIAN_POINT('Ctrl Pts',(2.0698113262342,-1.,0.745574324794401));
#25533=CARTESIAN_POINT('Ctrl Pts',(2.0698113262342,1.,0.745574324794401));
#25534=CARTESIAN_POINT('',(1.60662857109684,1.,0.693717979106306));
#25535=CARTESIAN_POINT('Ctrl Pts',(1.60662857109684,1.,0.693717979106306));
#25536=CARTESIAN_POINT('Ctrl Pts',(1.61106790958151,1.,0.695712097881194));
#25537=CARTESIAN_POINT('Ctrl Pts',(1.61974673472612,1.,0.699605146405088));
#25538=CARTESIAN_POINT('Ctrl Pts',(1.63216541664676,1.,0.705159151988319));
#25539=CARTESIAN_POINT('Ctrl Pts',(1.64752408832016,1.,0.711993139355394));
#25540=CARTESIAN_POINT('Ctrl Pts',(1.6647288055568,1.,0.719585433804282));
#25541=CARTESIAN_POINT('Ctrl Pts',(1.67996158455503,1.,0.726235967997433));
#25542=CARTESIAN_POINT('Ctrl Pts',(1.69326921975743,1.,0.731963238697195));
#25543=CARTESIAN_POINT('Ctrl Pts',(1.70473309006121,1.,0.736799665724771));
#25544=CARTESIAN_POINT('Ctrl Pts',(1.71447789751927,1.,0.740795162032088));
#25545=CARTESIAN_POINT('Ctrl Pts',(1.7226822991693,1.,0.744021445433765));
#25546=CARTESIAN_POINT('Ctrl Pts',(1.72958533647399,1.,0.746574710096437));
#25547=CARTESIAN_POINT('Ctrl Pts',(1.73550351679848,1.,0.748582462954855));
#25548=CARTESIAN_POINT('Ctrl Pts',(1.74080458266705,1.,0.750193435979541));
#25549=CARTESIAN_POINT('Ctrl Pts',(1.74585086852298,1.,0.751555614163629));
#25550=CARTESIAN_POINT('Ctrl Pts',(1.75095139468809,1.,0.752797683531377));
#25551=CARTESIAN_POINT('Ctrl Pts',(1.75631083600175,1.,0.75400925402848));
#25552=CARTESIAN_POINT('Ctrl Pts',(1.7619781724032,1.,0.755220979975262));
#25553=CARTESIAN_POINT('Ctrl Pts',(1.76789396003141,1.,0.756421896028403));
#25554=CARTESIAN_POINT('Ctrl Pts',(1.77394167108342,1.,0.757578264077238));
#25555=CARTESIAN_POINT('Ctrl Pts',(1.77999411220912,1.,0.75865062667738));
#25556=CARTESIAN_POINT('Ctrl Pts',(1.78596964884526,1.,0.759614401109868));
#25557=CARTESIAN_POINT('Ctrl Pts',(1.79185815610802,1.,0.760469555880425));
#25558=CARTESIAN_POINT('Ctrl Pts',(1.79768986997735,1.,0.761229695230359));
#25559=CARTESIAN_POINT('Ctrl Pts',(1.80351583877334,1.,0.761915336443516));
#25560=CARTESIAN_POINT('Ctrl Pts',(1.80938551463989,1.,0.762546129464036));
#25561=CARTESIAN_POINT('Ctrl Pts',(1.81532118405566,1.,0.763132003836783));
#25562=CARTESIAN_POINT('Ctrl Pts',(1.82131873145297,1.,0.763673465462854));
#25563=CARTESIAN_POINT('Ctrl Pts',(1.8273599120008,1.,0.764165902606056));
#25564=CARTESIAN_POINT('Ctrl Pts',(1.8334207722714,1.,0.764602549687846));
#25565=CARTESIAN_POINT('Ctrl Pts',(1.83948181064823,1.,0.764978057881688));
#25566=CARTESIAN_POINT('Ctrl Pts',(1.8455369887591,1.,0.765291664861972));
#25567=CARTESIAN_POINT('Ctrl Pts',(1.85158945130054,1.,0.765545710619023));
#25568=CARTESIAN_POINT('Ctrl Pts',(1.85764741390391,1.,0.765744212909305));
#25569=CARTESIAN_POINT('Ctrl Pts',(1.86372027063314,1.,0.765891519092557));
#25570=CARTESIAN_POINT('Ctrl Pts',(1.86981398314345,1.,0.765990708546112));
#25571=CARTESIAN_POINT('Ctrl Pts',(1.87592888967886,1.,0.766042837036759));
#25572=CARTESIAN_POINT('Ctrl Pts',(1.88206215302561,1.,0.766047794851869));
#25573=CARTESIAN_POINT('Ctrl Pts',(1.88820926433409,1.,0.76600483706209));
#25574=CARTESIAN_POINT('Ctrl Pts',(1.89436577771389,1.,0.765913193856979));
#25575=CARTESIAN_POINT('Ctrl Pts',(1.90052930393599,1.,0.765772772593395));
#25576=CARTESIAN_POINT('Ctrl Pts',(1.90669961402362,1.,0.765584196937937));
#25577=CARTESIAN_POINT('Ctrl Pts',(1.91287765805174,1.,0.765348465884739));
#25578=CARTESIAN_POINT('Ctrl Pts',(1.91906491634197,1.,0.765066729667095));
#25579=CARTESIAN_POINT('Ctrl Pts',(1.92526263537041,1.,0.764740025488189));
#25580=CARTESIAN_POINT('Ctrl Pts',(1.93147105496367,1.,0.76436901067389));
#25581=CARTESIAN_POINT('Ctrl Pts',(1.93768964875867,1.,0.763954049121394));
#25582=CARTESIAN_POINT('Ctrl Pts',(1.94391746617626,1.,0.763495333538581));
#25583=CARTESIAN_POINT('Ctrl Pts',(1.95015342590025,1.,0.762992990878774));
#25584=CARTESIAN_POINT('Ctrl Pts',(1.95639665309893,1.,0.762447203806264));
#25585=CARTESIAN_POINT('Ctrl Pts',(1.96264672744229,1.,0.761858300014575));
#25586=CARTESIAN_POINT('Ctrl Pts',(1.96890351582545,1.,0.761226690483986));
#25587=CARTESIAN_POINT('Ctrl Pts',(1.97516705321521,1.,0.760552825409856));
#25588=CARTESIAN_POINT('Ctrl Pts',(1.98143741418156,1.,0.759837147452135));
#25589=CARTESIAN_POINT('Ctrl Pts',(1.98771456680806,1.,0.759080037802243));
#25590=CARTESIAN_POINT('Ctrl Pts',(1.9939983109871,1.,0.758281796766377));
#25591=CARTESIAN_POINT('Ctrl Pts',(2.00028834739072,1.,0.757442676862342));
#25592=CARTESIAN_POINT('Ctrl Pts',(2.00658431587682,1.,0.756562904646496));
#25593=CARTESIAN_POINT('Ctrl Pts',(2.01288584328149,1.,0.755642704958101));
#25594=CARTESIAN_POINT('Ctrl Pts',(2.01919259406003,1.,0.75468233072352));
#25595=CARTESIAN_POINT('Ctrl Pts',(2.02550428623587,1.,0.753682061113766));
#25596=CARTESIAN_POINT('Ctrl Pts',(2.03182068456467,1.,0.752642180488104));
#25597=CARTESIAN_POINT('Ctrl Pts',(2.03814160092173,1.,0.751562963361384));
#25598=CARTESIAN_POINT('Ctrl Pts',(2.04446689147754,1.,0.750444657874758));
#25599=CARTESIAN_POINT('Ctrl Pts',(2.05079645591606,1.,0.749287468663053));
#25600=CARTESIAN_POINT('Ctrl Pts',(2.05713023030263,1.,0.748091554181101));
#25601=CARTESIAN_POINT('Ctrl Pts',(2.06220058927162,1.,0.747103932785504));
#25602=CARTESIAN_POINT('Ctrl Pts',(2.06600523016401,1.,0.746345871542696));
#25603=CARTESIAN_POINT('Ctrl Pts',(2.06854248895575,1.,0.74583279137781));
#25604=CARTESIAN_POINT('Ctrl Pts',(2.0698113262342,1.,0.745574324794401));
#25605=CARTESIAN_POINT('',(1.60662857109684,0.,0.693717979106305));
#25606=CARTESIAN_POINT('Origin',(0.,0.,0.));
#25607=CARTESIAN_POINT('',(1.5055822144029,1.,0.892032620296856));
#25608=CARTESIAN_POINT('Origin',(0.,1.,0.));
#25609=CARTESIAN_POINT('',(1.5055822144029,0.,0.892032620296855));
#25610=CARTESIAN_POINT('Ctrl Pts',(1.81978687191668,-1.,1.23627494547115));
#25611=CARTESIAN_POINT('Ctrl Pts',(1.81978687191668,1.,1.23627494547115));
#25612=CARTESIAN_POINT('Ctrl Pts',(1.81925017193666,-1.,1.23509651170476));
#25613=CARTESIAN_POINT('Ctrl Pts',(1.81925017193666,1.,1.23509651170476));
#25614=CARTESIAN_POINT('Ctrl Pts',(1.81817389921279,-1.,1.2327422452705));
#25615=CARTESIAN_POINT('Ctrl Pts',(1.81817389921279,1.,1.2327422452705));
#25616=CARTESIAN_POINT('Ctrl Pts',(1.8165508718364,-1.,1.2292186489137));
#25617=CARTESIAN_POINT('Ctrl Pts',(1.8165508718364,1.,1.2292186489137));
#25618=CARTESIAN_POINT('Ctrl Pts',(1.81436959210434,-1.,1.2245361330495));
#25619=CARTESIAN_POINT('Ctrl Pts',(1.81436959210434,1.,1.2245361330495));
#25620=CARTESIAN_POINT('Ctrl Pts',(1.81161420806656,-1.,1.21870906103557));
#25621=CARTESIAN_POINT('Ctrl Pts',(1.81161420806656,1.,1.21870906103557));
#25622=CARTESIAN_POINT('Ctrl Pts',(1.80882996917129,-1.,1.21290815708314));
#25623=CARTESIAN_POINT('Ctrl Pts',(1.80882996917129,1.,1.21290815708314));
#25624=CARTESIAN_POINT('Ctrl Pts',(1.80601678480707,-1.,1.20713356605475));
#25625=CARTESIAN_POINT('Ctrl Pts',(1.80601678480707,1.,1.20713356605475));
#25626=CARTESIAN_POINT('Ctrl Pts',(1.80317454838603,-1.,1.20138548938974));
#25627=CARTESIAN_POINT('Ctrl Pts',(1.80317454838603,1.,1.20138548938974));
#25628=CARTESIAN_POINT('Ctrl Pts',(1.80030314369879,-1.,1.19566418930242));
#25629=CARTESIAN_POINT('Ctrl Pts',(1.80030314369879,1.,1.19566418930242));
#25630=CARTESIAN_POINT('Ctrl Pts',(1.79740245923478,-1.,1.18996997934445));
#25631=CARTESIAN_POINT('Ctrl Pts',(1.79740245923478,1.,1.18996997934445));
#25632=CARTESIAN_POINT('Ctrl Pts',(1.79447240321515,-1.,1.18430321697432));
#25633=CARTESIAN_POINT('Ctrl Pts',(1.79447240321515,1.,1.18430321697432));
#25634=CARTESIAN_POINT('Ctrl Pts',(1.79151291552689,-1.,1.17866429440809));
#25635=CARTESIAN_POINT('Ctrl Pts',(1.79151291552689,1.,1.17866429440809));
#25636=CARTESIAN_POINT('Ctrl Pts',(1.78852398877616,-1.,1.17305363177328));
#25637=CARTESIAN_POINT('Ctrl Pts',(1.78852398877616,1.,1.17305363177328));
#25638=CARTESIAN_POINT('Ctrl Pts',(1.78550566040443,-1.,1.16747166312303));
#25639=CARTESIAN_POINT('Ctrl Pts',(1.78550566040443,1.,1.16747166312303));
#25640=CARTESIAN_POINT('Ctrl Pts',(1.78245795881009,-1.,1.16191881298499));
#25641=CARTESIAN_POINT('Ctrl Pts',(1.78245795881009,1.,1.16191881298499));
#25642=CARTESIAN_POINT('Ctrl Pts',(1.77938085564275,-1.,1.15639547194698));
#25643=CARTESIAN_POINT('Ctrl Pts',(1.77938085564275,1.,1.15639547194698));
#25644=CARTESIAN_POINT('Ctrl Pts',(1.7762742255701,-1.,1.15090197841515));
#25645=CARTESIAN_POINT('Ctrl Pts',(1.7762742255701,1.,1.15090197841515));
#25646=CARTESIAN_POINT('Ctrl Pts',(1.77313777896194,-1.,1.1454385822692));
#25647=CARTESIAN_POINT('Ctrl Pts',(1.77313777896194,1.,1.1454385822692));
#25648=CARTESIAN_POINT('Ctrl Pts',(1.76997111386769,-1.,1.14000548336975));
#25649=CARTESIAN_POINT('Ctrl Pts',(1.76997111386769,1.,1.14000548336975));
#25650=CARTESIAN_POINT('Ctrl Pts',(1.76677384551862,-1.,1.1346029180462));
#25651=CARTESIAN_POINT('Ctrl Pts',(1.76677384551862,1.,1.1346029180462));
#25652=CARTESIAN_POINT('Ctrl Pts',(1.7635457196617,-1.,1.12923123555075));
#25653=CARTESIAN_POINT('Ctrl Pts',(1.7635457196617,1.,1.12923123555075));
#25654=CARTESIAN_POINT('Ctrl Pts',(1.76028671825096,-1.,1.12389096855086));
#25655=CARTESIAN_POINT('Ctrl Pts',(1.76028671825096,1.,1.12389096855086));
#25656=CARTESIAN_POINT('Ctrl Pts',(1.75699720772105,-1.,1.11858293216763));
#25657=CARTESIAN_POINT('Ctrl Pts',(1.75699720772105,1.,1.11858293216763));
#25658=CARTESIAN_POINT('Ctrl Pts',(1.7536777209463,-1.,1.11330807582551));
#25659=CARTESIAN_POINT('Ctrl Pts',(1.7536777209463,1.,1.11330807582551));
#25660=CARTESIAN_POINT('Ctrl Pts',(1.7503286607592,-1.,1.10806728183007));
#25661=CARTESIAN_POINT('Ctrl Pts',(1.7503286607592,1.,1.10806728183007));
#25662=CARTESIAN_POINT('Ctrl Pts',(1.74695004214923,-1.,1.10286118991143));
#25663=CARTESIAN_POINT('Ctrl Pts',(1.74695004214923,1.,1.10286118991143));
#25664=CARTESIAN_POINT('Ctrl Pts',(1.74354119236208,-1.,1.09768999241226));
#25665=CARTESIAN_POINT('Ctrl Pts',(1.74354119236208,1.,1.09768999241226));
#25666=CARTESIAN_POINT('Ctrl Pts',(1.74010053962247,-1.,1.09255329056493));
#25667=CARTESIAN_POINT('Ctrl Pts',(1.74010053962247,1.,1.09255329056493));
#25668=CARTESIAN_POINT('Ctrl Pts',(1.73662628326091,-1.,1.08745056285427));
#25669=CARTESIAN_POINT('Ctrl Pts',(1.73662628326091,1.,1.08745056285427));
#25670=CARTESIAN_POINT('Ctrl Pts',(1.73311705663407,-1.,1.08238162784749));
#25671=CARTESIAN_POINT('Ctrl Pts',(1.73311705663407,1.,1.08238162784749));
#25672=CARTESIAN_POINT('Ctrl Pts',(1.72957248977424,-1.,1.0773470373727));
#25673=CARTESIAN_POINT('Ctrl Pts',(1.72957248977424,1.,1.0773470373727));
#25674=CARTESIAN_POINT('Ctrl Pts',(1.72599406198488,-1.,1.07234866990252));
#25675=CARTESIAN_POINT('Ctrl Pts',(1.72599406198488,1.,1.07234866990252));
#25676=CARTESIAN_POINT('Ctrl Pts',(1.72238500928453,-1.,1.06738966975462));
#25677=CARTESIAN_POINT('Ctrl Pts',(1.72238500928453,1.,1.06738966975462));
#25678=CARTESIAN_POINT('Ctrl Pts',(1.71874858456904,-1.,1.06247324680647));
#25679=CARTESIAN_POINT('Ctrl Pts',(1.71874858456904,1.,1.06247324680647));
#25680=CARTESIAN_POINT('Ctrl Pts',(1.7150865442702,-1.,1.05760163192479));
#25681=CARTESIAN_POINT('Ctrl Pts',(1.7150865442702,1.,1.05760163192479));
#25682=CARTESIAN_POINT('Ctrl Pts',(1.71139783543989,-1.,1.05277517202855));
#25683=CARTESIAN_POINT('Ctrl Pts',(1.71139783543989,1.,1.05277517202855));
#25684=CARTESIAN_POINT('Ctrl Pts',(1.70767646263649,-1.,1.04799085404995));
#25685=CARTESIAN_POINT('Ctrl Pts',(1.70767646263649,1.,1.04799085404995));
#25686=CARTESIAN_POINT('Ctrl Pts',(1.70391338707982,-1.,1.04324363334554));
#25687=CARTESIAN_POINT('Ctrl Pts',(1.70391338707982,1.,1.04324363334554));
#25688=CARTESIAN_POINT('Ctrl Pts',(1.70010052930962,-1.,1.03852922490789));
#25689=CARTESIAN_POINT('Ctrl Pts',(1.70010052930962,1.,1.03852922490789));
#25690=CARTESIAN_POINT('Ctrl Pts',(1.69623414782771,-1.,1.03384646003588));
#25691=CARTESIAN_POINT('Ctrl Pts',(1.69623414782771,1.,1.03384646003588));
#25692=CARTESIAN_POINT('Ctrl Pts',(1.69231840863458,-1.,1.02919977579147));
#25693=CARTESIAN_POINT('Ctrl Pts',(1.69231840863458,1.,1.02919977579147));
#25694=CARTESIAN_POINT('Ctrl Pts',(1.68836910178447,-1.,1.02460180535255));
#25695=CARTESIAN_POINT('Ctrl Pts',(1.68836910178447,1.,1.02460180535255));
#25696=CARTESIAN_POINT('Ctrl Pts',(1.68440578021706,-1.,1.02006795074201));
#25697=CARTESIAN_POINT('Ctrl Pts',(1.68440578021706,1.,1.02006795074201));
#25698=CARTESIAN_POINT('Ctrl Pts',(1.68044289894798,-1.,1.01561026162773));
#25699=CARTESIAN_POINT('Ctrl Pts',(1.68044289894798,1.,1.01561026162773));
#25700=CARTESIAN_POINT('Ctrl Pts',(1.67648246776464,-1.,1.01123236493511));
#25701=CARTESIAN_POINT('Ctrl Pts',(1.67648246776464,1.,1.01123236493511));
#25702=CARTESIAN_POINT('Ctrl Pts',(1.67250335383293,-1.,1.00692206696414));
#25703=CARTESIAN_POINT('Ctrl Pts',(1.67250335383293,1.,1.00692206696414));
#25704=CARTESIAN_POINT('Ctrl Pts',(1.66846059277303,-1.,1.00265091003727));
#25705=CARTESIAN_POINT('Ctrl Pts',(1.66846059277303,1.,1.00265091003727));
#25706=CARTESIAN_POINT('Ctrl Pts',(1.66430758030376,-1.,0.998389654952758));
#25707=CARTESIAN_POINT('Ctrl Pts',(1.66430758030376,1.,0.998389654952758));
#25708=CARTESIAN_POINT('Ctrl Pts',(1.66001553809947,-1.,0.994121836661306));
#25709=CARTESIAN_POINT('Ctrl Pts',(1.66001553809947,1.,0.994121836661306));
#25710=CARTESIAN_POINT('Ctrl Pts',(1.65559044289699,-1.,0.989855627854165));
#25711=CARTESIAN_POINT('Ctrl Pts',(1.65559044289699,1.,0.989855627854165));
#25712=CARTESIAN_POINT('Ctrl Pts',(1.65110016612638,-1.,0.985642622920821));
#25713=CARTESIAN_POINT('Ctrl Pts',(1.65110016612638,1.,0.985642622920821));
#25714=CARTESIAN_POINT('Ctrl Pts',(1.64665139190656,-1.,0.981562530939489));
#25715=CARTESIAN_POINT('Ctrl Pts',(1.64665139190656,1.,0.981562530939489));
#25716=CARTESIAN_POINT('Ctrl Pts',(1.64233990826687,-1.,0.977689794119417));
#25717=CARTESIAN_POINT('Ctrl Pts',(1.64233990826687,1.,0.977689794119417));
#25718=CARTESIAN_POINT('Ctrl Pts',(1.63820952658144,-1.,0.974066058287419));
#25719=CARTESIAN_POINT('Ctrl Pts',(1.63820952658144,1.,0.974066058287419));
#25720=CARTESIAN_POINT('Ctrl Pts',(1.63420665729798,-1.,0.970669715997509));
#25721=CARTESIAN_POINT('Ctrl Pts',(1.63420665729798,1.,0.970669715997509));
#25722=CARTESIAN_POINT('Ctrl Pts',(1.63013849959461,-1.,0.967387853230345));
#25723=CARTESIAN_POINT('Ctrl Pts',(1.63013849959461,1.,0.967387853230345));
#25724=CARTESIAN_POINT('Ctrl Pts',(1.62571930670187,-1.,0.964046107040536));
#25725=CARTESIAN_POINT('Ctrl Pts',(1.62571930670187,1.,0.964046107040536));
#25726=CARTESIAN_POINT('Ctrl Pts',(1.62061638140221,-1.,0.960438326101729));
#25727=CARTESIAN_POINT('Ctrl Pts',(1.62061638140221,1.,0.960438326101729));
#25728=CARTESIAN_POINT('Ctrl Pts',(1.61449324337085,-1.,0.956354422920671));
#25729=CARTESIAN_POINT('Ctrl Pts',(1.61449324337085,1.,0.956354422920671));
#25730=CARTESIAN_POINT('Ctrl Pts',(1.60706069896936,-1.,0.951613284356035));
#25731=CARTESIAN_POINT('Ctrl Pts',(1.60706069896936,1.,0.951613284356035));
#25732=CARTESIAN_POINT('Ctrl Pts',(1.59810042043673,-1.,0.946078063315257));
#25733=CARTESIAN_POINT('Ctrl Pts',(1.59810042043673,1.,0.946078063315257));
#25734=CARTESIAN_POINT('Ctrl Pts',(1.58744937487176,-1.,0.939646377893399));
#25735=CARTESIAN_POINT('Ctrl Pts',(1.58744937487176,1.,0.939646377893399));
#25736=CARTESIAN_POINT('Ctrl Pts',(1.57499388382243,-1.,0.932246680108685));
#25737=CARTESIAN_POINT('Ctrl Pts',(1.57499388382243,1.,0.932246680108685));
#25738=CARTESIAN_POINT('Ctrl Pts',(1.56065988578893,-1.,0.923832188944341));
#25739=CARTESIAN_POINT('Ctrl Pts',(1.56065988578893,1.,0.923832188944341));
#25740=CARTESIAN_POINT('Ctrl Pts',(1.54440491149498,-1.,0.914375919026456));
#25741=CARTESIAN_POINT('Ctrl Pts',(1.54440491149498,1.,0.914375919026456));
#25742=CARTESIAN_POINT('Ctrl Pts',(1.52984849887993,-1.,0.905967409625651));
#25743=CARTESIAN_POINT('Ctrl Pts',(1.52984849887993,1.,0.905967409625651));
#25744=CARTESIAN_POINT('Ctrl Pts',(1.51805569590094,-1.,0.899185047483511));
#25745=CARTESIAN_POINT('Ctrl Pts',(1.51805569590094,1.,0.899185047483511));
#25746=CARTESIAN_POINT('Ctrl Pts',(1.50980486806688,-1.,0.894452006964544));
#25747=CARTESIAN_POINT('Ctrl Pts',(1.50980486806688,1.,0.894452006964544));
#25748=CARTESIAN_POINT('Ctrl Pts',(1.5055822144029,-1.,0.892032620296856));
#25749=CARTESIAN_POINT('Ctrl Pts',(1.5055822144029,1.,0.892032620296856));
#25750=CARTESIAN_POINT('',(1.81978687191668,1.,1.23627494547115));
#25751=CARTESIAN_POINT('Ctrl Pts',(1.81978687191668,1.,1.23627494547115));
#25752=CARTESIAN_POINT('Ctrl Pts',(1.81925017193666,1.,1.23509651170476));
#25753=CARTESIAN_POINT('Ctrl Pts',(1.81817389921279,1.,1.2327422452705));
#25754=CARTESIAN_POINT('Ctrl Pts',(1.8165508718364,1.,1.2292186489137));
#25755=CARTESIAN_POINT('Ctrl Pts',(1.81436959210434,1.,1.2245361330495));
#25756=CARTESIAN_POINT('Ctrl Pts',(1.81161420806656,1.,1.21870906103557));
#25757=CARTESIAN_POINT('Ctrl Pts',(1.80882996917129,1.,1.21290815708314));
#25758=CARTESIAN_POINT('Ctrl Pts',(1.80601678480707,1.,1.20713356605475));
#25759=CARTESIAN_POINT('Ctrl Pts',(1.80317454838603,1.,1.20138548938974));
#25760=CARTESIAN_POINT('Ctrl Pts',(1.80030314369879,1.,1.19566418930242));
#25761=CARTESIAN_POINT('Ctrl Pts',(1.79740245923478,1.,1.18996997934445));
#25762=CARTESIAN_POINT('Ctrl Pts',(1.79447240321515,1.,1.18430321697432));
#25763=CARTESIAN_POINT('Ctrl Pts',(1.79151291552689,1.,1.17866429440809));
#25764=CARTESIAN_POINT('Ctrl Pts',(1.78852398877616,1.,1.17305363177328));
#25765=CARTESIAN_POINT('Ctrl Pts',(1.78550566040443,1.,1.16747166312303));
#25766=CARTESIAN_POINT('Ctrl Pts',(1.78245795881009,1.,1.16191881298499));
#25767=CARTESIAN_POINT('Ctrl Pts',(1.77938085564275,1.,1.15639547194698));
#25768=CARTESIAN_POINT('Ctrl Pts',(1.7762742255701,1.,1.15090197841515));
#25769=CARTESIAN_POINT('Ctrl Pts',(1.77313777896194,1.,1.1454385822692));
#25770=CARTESIAN_POINT('Ctrl Pts',(1.76997111386769,1.,1.14000548336975));
#25771=CARTESIAN_POINT('Ctrl Pts',(1.76677384551862,1.,1.1346029180462));
#25772=CARTESIAN_POINT('Ctrl Pts',(1.7635457196617,1.,1.12923123555075));
#25773=CARTESIAN_POINT('Ctrl Pts',(1.76028671825096,1.,1.12389096855086));
#25774=CARTESIAN_POINT('Ctrl Pts',(1.75699720772105,1.,1.11858293216763));
#25775=CARTESIAN_POINT('Ctrl Pts',(1.7536777209463,1.,1.11330807582551));
#25776=CARTESIAN_POINT('Ctrl Pts',(1.7503286607592,1.,1.10806728183007));
#25777=CARTESIAN_POINT('Ctrl Pts',(1.74695004214923,1.,1.10286118991143));
#25778=CARTESIAN_POINT('Ctrl Pts',(1.74354119236208,1.,1.09768999241226));
#25779=CARTESIAN_POINT('Ctrl Pts',(1.74010053962247,1.,1.09255329056493));
#25780=CARTESIAN_POINT('Ctrl Pts',(1.73662628326091,1.,1.08745056285427));
#25781=CARTESIAN_POINT('Ctrl Pts',(1.73311705663407,1.,1.08238162784749));
#25782=CARTESIAN_POINT('Ctrl Pts',(1.72957248977424,1.,1.0773470373727));
#25783=CARTESIAN_POINT('Ctrl Pts',(1.72599406198488,1.,1.07234866990252));
#25784=CARTESIAN_POINT('Ctrl Pts',(1.72238500928453,1.,1.06738966975462));
#25785=CARTESIAN_POINT('Ctrl Pts',(1.71874858456904,1.,1.06247324680647));
#25786=CARTESIAN_POINT('Ctrl Pts',(1.7150865442702,1.,1.05760163192479));
#25787=CARTESIAN_POINT('Ctrl Pts',(1.71139783543989,1.,1.05277517202855));
#25788=CARTESIAN_POINT('Ctrl Pts',(1.70767646263649,1.,1.04799085404995));
#25789=CARTESIAN_POINT('Ctrl Pts',(1.70391338707982,1.,1.04324363334554));
#25790=CARTESIAN_POINT('Ctrl Pts',(1.70010052930962,1.,1.03852922490789));
#25791=CARTESIAN_POINT('Ctrl Pts',(1.69623414782771,1.,1.03384646003588));
#25792=CARTESIAN_POINT('Ctrl Pts',(1.69231840863458,1.,1.02919977579147));
#25793=CARTESIAN_POINT('Ctrl Pts',(1.68836910178447,1.,1.02460180535255));
#25794=CARTESIAN_POINT('Ctrl Pts',(1.68440578021706,1.,1.02006795074201));
#25795=CARTESIAN_POINT('Ctrl Pts',(1.68044289894798,1.,1.01561026162773));
#25796=CARTESIAN_POINT('Ctrl Pts',(1.67648246776464,1.,1.01123236493511));
#25797=CARTESIAN_POINT('Ctrl Pts',(1.67250335383293,1.,1.00692206696414));
#25798=CARTESIAN_POINT('Ctrl Pts',(1.66846059277303,1.,1.00265091003727));
#25799=CARTESIAN_POINT('Ctrl Pts',(1.66430758030376,1.,0.998389654952758));
#25800=CARTESIAN_POINT('Ctrl Pts',(1.66001553809947,1.,0.994121836661306));
#25801=CARTESIAN_POINT('Ctrl Pts',(1.65559044289699,1.,0.989855627854165));
#25802=CARTESIAN_POINT('Ctrl Pts',(1.65110016612638,1.,0.985642622920821));
#25803=CARTESIAN_POINT('Ctrl Pts',(1.64665139190656,1.,0.981562530939489));
#25804=CARTESIAN_POINT('Ctrl Pts',(1.64233990826687,1.,0.977689794119417));
#25805=CARTESIAN_POINT('Ctrl Pts',(1.63820952658144,1.,0.974066058287419));
#25806=CARTESIAN_POINT('Ctrl Pts',(1.63420665729798,1.,0.970669715997509));
#25807=CARTESIAN_POINT('Ctrl Pts',(1.63013849959461,1.,0.967387853230345));
#25808=CARTESIAN_POINT('Ctrl Pts',(1.62571930670187,1.,0.964046107040536));
#25809=CARTESIAN_POINT('Ctrl Pts',(1.62061638140221,1.,0.960438326101729));
#25810=CARTESIAN_POINT('Ctrl Pts',(1.61449324337085,1.,0.956354422920671));
#25811=CARTESIAN_POINT('Ctrl Pts',(1.60706069896936,1.,0.951613284356035));
#25812=CARTESIAN_POINT('Ctrl Pts',(1.59810042043673,1.,0.946078063315257));
#25813=CARTESIAN_POINT('Ctrl Pts',(1.58744937487176,1.,0.939646377893399));
#25814=CARTESIAN_POINT('Ctrl Pts',(1.57499388382243,1.,0.932246680108685));
#25815=CARTESIAN_POINT('Ctrl Pts',(1.56065988578893,1.,0.923832188944341));
#25816=CARTESIAN_POINT('Ctrl Pts',(1.54440491149498,1.,0.914375919026456));
#25817=CARTESIAN_POINT('Ctrl Pts',(1.52984849887993,1.,0.905967409625651));
#25818=CARTESIAN_POINT('Ctrl Pts',(1.51805569590094,1.,0.899185047483511));
#25819=CARTESIAN_POINT('Ctrl Pts',(1.50980486806688,1.,0.894452006964544));
#25820=CARTESIAN_POINT('Ctrl Pts',(1.5055822144029,1.,0.892032620296856));
#25821=CARTESIAN_POINT('',(1.81978687191668,0.,1.23627494547115));
#25822=CARTESIAN_POINT('Origin',(1.73811241238545,0.,1.34869019493419));
#25823=CARTESIAN_POINT('',(1.73811241238545,1.,1.34869019493419));
#25824=CARTESIAN_POINT('',(1.81978687191668,1.,1.23627494547115));
#25825=CARTESIAN_POINT('',(1.73811241238545,0.,1.34869019493419));
#25826=CARTESIAN_POINT('Ctrl Pts',(1.31362392696032,-1.,1.15624053661742));
#25827=CARTESIAN_POINT('Ctrl Pts',(1.31362392696032,1.,1.15624053661742));
#25828=CARTESIAN_POINT('Ctrl Pts',(1.31722977216397,-1.,1.15950888730809));
#25829=CARTESIAN_POINT('Ctrl Pts',(1.31722977216397,1.,1.15950888730809));
#25830=CARTESIAN_POINT('Ctrl Pts',(1.32428080721772,-1.,1.16589330093588));
#25831=CARTESIAN_POINT('Ctrl Pts',(1.32428080721772,1.,1.16589330093588));
#25832=CARTESIAN_POINT('Ctrl Pts',(1.33437539347008,-1.,1.17501305789857));
#25833=CARTESIAN_POINT('Ctrl Pts',(1.33437539347008,1.,1.17501305789857));
#25834=CARTESIAN_POINT('Ctrl Pts',(1.34687054001093,-1.,1.18625865667441));
#25835=CARTESIAN_POINT('Ctrl Pts',(1.34687054001093,1.,1.18625865667441));
#25836=CARTESIAN_POINT('Ctrl Pts',(1.36088705043885,-1.,1.1987959077932));
#25837=CARTESIAN_POINT('Ctrl Pts',(1.36088705043885,1.,1.1987959077932));
#25838=CARTESIAN_POINT('Ctrl Pts',(1.37331915607905,-1.,1.20982812925645));
#25839=CARTESIAN_POINT('Ctrl Pts',(1.37331915607905,1.,1.20982812925645));
#25840=CARTESIAN_POINT('Ctrl Pts',(1.38420564527715,-1.,1.21938737280852));
#25841=CARTESIAN_POINT('Ctrl Pts',(1.38420564527715,1.,1.21938737280852));
#25842=CARTESIAN_POINT('Ctrl Pts',(1.39361389568796,-1.,1.22752961899387));
#25843=CARTESIAN_POINT('Ctrl Pts',(1.39361389568796,1.,1.22752961899387));
#25844=CARTESIAN_POINT('Ctrl Pts',(1.40164708206106,-1.,1.23434087290423));
#25845=CARTESIAN_POINT('Ctrl Pts',(1.40164708206106,1.,1.23434087290423));
#25846=CARTESIAN_POINT('Ctrl Pts',(1.40845295531283,-1.,1.23994455029534));
#25847=CARTESIAN_POINT('Ctrl Pts',(1.40845295531283,1.,1.23994455029534));
#25848=CARTESIAN_POINT('Ctrl Pts',(1.41422913175179,-1.,1.24450600513056));
#25849=CARTESIAN_POINT('Ctrl Pts',(1.41422913175179,1.,1.24450600513056));
#25850=CARTESIAN_POINT('Ctrl Pts',(1.41923722596025,-1.,1.24824430986571));
#25851=CARTESIAN_POINT('Ctrl Pts',(1.41923722596025,1.,1.24824430986571));
#25852=CARTESIAN_POINT('Ctrl Pts',(1.42378102115575,-1.,1.2514145557001));
#25853=CARTESIAN_POINT('Ctrl Pts',(1.42378102115575,1.,1.2514145557001));
#25854=CARTESIAN_POINT('Ctrl Pts',(1.42815938799387,-1.,1.25426945222639));
#25855=CARTESIAN_POINT('Ctrl Pts',(1.42815938799387,1.,1.25426945222639));
#25856=CARTESIAN_POINT('Ctrl Pts',(1.43262645609691,-1.,1.25702687965755));
#25857=CARTESIAN_POINT('Ctrl Pts',(1.43262645609691,1.,1.25702687965755));
#25858=CARTESIAN_POINT('Ctrl Pts',(1.43734919180847,-1.,1.25983531012005));
#25859=CARTESIAN_POINT('Ctrl Pts',(1.43734919180847,1.,1.25983531012005));
#25860=CARTESIAN_POINT('Ctrl Pts',(1.44236470511303,-1.,1.26273903323859));
#25861=CARTESIAN_POINT('Ctrl Pts',(1.44236470511303,1.,1.26273903323859));
#25862=CARTESIAN_POINT('Ctrl Pts',(1.44761985001662,-1.,1.26570925118868));
#25863=CARTESIAN_POINT('Ctrl Pts',(1.44761985001662,1.,1.26570925118868));
#25864=CARTESIAN_POINT('Ctrl Pts',(1.45301422764247,-1.,1.2686778680489));
#25865=CARTESIAN_POINT('Ctrl Pts',(1.45301422764247,1.,1.2686778680489));
#25866=CARTESIAN_POINT('Ctrl Pts',(1.45843906294697,-1.,1.27156805265289));
#25867=CARTESIAN_POINT('Ctrl Pts',(1.45843906294697,1.,1.27156805265289));
#25868=CARTESIAN_POINT('Ctrl Pts',(1.46382431332476,-1.,1.27433119897822));
#25869=CARTESIAN_POINT('Ctrl Pts',(1.46382431332476,1.,1.27433119897822));
#25870=CARTESIAN_POINT('Ctrl Pts',(1.46916035917133,-1.,1.2769641483109));
#25871=CARTESIAN_POINT('Ctrl Pts',(1.46916035917133,1.,1.2769641483109));
#25872=CARTESIAN_POINT('Ctrl Pts',(1.4744717526707,-1.,1.2794891824849));
#25873=CARTESIAN_POINT('Ctrl Pts',(1.4744717526707,1.,1.2794891824849));
#25874=CARTESIAN_POINT('Ctrl Pts',(1.47980070347095,-1.,1.28194158939517));
#25875=CARTESIAN_POINT('Ctrl Pts',(1.47980070347095,1.,1.28194158939517));
#25876=CARTESIAN_POINT('Ctrl Pts',(1.4851881711891,-1.,1.28435533880201));
#25877=CARTESIAN_POINT('Ctrl Pts',(1.4851881711891,1.,1.28435533880201));
#25878=CARTESIAN_POINT('Ctrl Pts',(1.4906522831278,-1.,1.2867467611644));
#25879=CARTESIAN_POINT('Ctrl Pts',(1.4906522831278,1.,1.2867467611644));
#25880=CARTESIAN_POINT('Ctrl Pts',(1.49618896881754,-1.,1.28911506584254));
#25881=CARTESIAN_POINT('Ctrl Pts',(1.49618896881754,1.,1.28911506584254));
#25882=CARTESIAN_POINT('Ctrl Pts',(1.50178230149776,-1.,1.29145022885181));
#25883=CARTESIAN_POINT('Ctrl Pts',(1.50178230149776,1.,1.29145022885181));
#25884=CARTESIAN_POINT('Ctrl Pts',(1.50741159078365,-1.,1.29373841372842));
#25885=CARTESIAN_POINT('Ctrl Pts',(1.50741159078365,1.,1.29373841372842));
#25886=CARTESIAN_POINT('Ctrl Pts',(1.51305994241402,-1.,1.29596850710509));
#25887=CARTESIAN_POINT('Ctrl Pts',(1.51305994241402,1.,1.29596850710509));
#25888=CARTESIAN_POINT('Ctrl Pts',(1.51872184912724,-1.,1.29813791800747));
#25889=CARTESIAN_POINT('Ctrl Pts',(1.51872184912724,1.,1.29813791800747));
#25890=CARTESIAN_POINT('Ctrl Pts',(1.52439957861062,-1.,1.30024984366328));
#25891=CARTESIAN_POINT('Ctrl Pts',(1.52439957861062,1.,1.30024984366328));
#25892=CARTESIAN_POINT('Ctrl Pts',(1.53009970283891,-1.,1.30231064395568));
#25893=CARTESIAN_POINT('Ctrl Pts',(1.53009970283891,1.,1.30231064395568));
#25894=CARTESIAN_POINT('Ctrl Pts',(1.53582981268977,-1.,1.30432735639489));
#25895=CARTESIAN_POINT('Ctrl Pts',(1.53582981268977,1.,1.30432735639489));
#25896=CARTESIAN_POINT('Ctrl Pts',(1.54159462645432,-1.,1.30630475189556));
#25897=CARTESIAN_POINT('Ctrl Pts',(1.54159462645432,1.,1.30630475189556));
#25898=CARTESIAN_POINT('Ctrl Pts',(1.54739413957185,-1.,1.30824393907473));
#25899=CARTESIAN_POINT('Ctrl Pts',(1.54739413957185,1.,1.30824393907473));
#25900=CARTESIAN_POINT('Ctrl Pts',(1.55322568759481,-1.,1.31014393684222));
#25901=CARTESIAN_POINT('Ctrl Pts',(1.55322568759481,1.,1.31014393684222));
#25902=CARTESIAN_POINT('Ctrl Pts',(1.55908521254821,-1.,1.31200264341696));
#25903=CARTESIAN_POINT('Ctrl Pts',(1.55908521254821,1.,1.31200264341696));
#25904=CARTESIAN_POINT('Ctrl Pts',(1.56496872402353,-1.,1.31381795281002));
#25905=CARTESIAN_POINT('Ctrl Pts',(1.56496872402353,1.,1.31381795281002));
#25906=CARTESIAN_POINT('Ctrl Pts',(1.57087397835723,-1.,1.31558903860016));
#25907=CARTESIAN_POINT('Ctrl Pts',(1.57087397835723,1.,1.31558903860016));
#25908=CARTESIAN_POINT('Ctrl Pts',(1.5768005650559,-1.,1.31731642317187));
#25909=CARTESIAN_POINT('Ctrl Pts',(1.5768005650559,1.,1.31731642317187));
#25910=CARTESIAN_POINT('Ctrl Pts',(1.58274907898834,-1.,1.31900135021432));
#25911=CARTESIAN_POINT('Ctrl Pts',(1.58274907898834,1.,1.31900135021432));
#25912=CARTESIAN_POINT('Ctrl Pts',(1.58872057258245,-1.,1.32064537110892));
#25913=CARTESIAN_POINT('Ctrl Pts',(1.58872057258245,1.,1.32064537110892));
#25914=CARTESIAN_POINT('Ctrl Pts',(1.59471591079403,-1.,1.32224985747682));
#25915=CARTESIAN_POINT('Ctrl Pts',(1.59471591079403,1.,1.32224985747682));
#25916=CARTESIAN_POINT('Ctrl Pts',(1.60073511858687,-1.,1.32381550858256));
#25917=CARTESIAN_POINT('Ctrl Pts',(1.60073511858687,1.,1.32381550858256));
#25918=CARTESIAN_POINT('Ctrl Pts',(1.60677758290954,-1.,1.32534250785782));
#25919=CARTESIAN_POINT('Ctrl Pts',(1.60677758290954,1.,1.32534250785782));
#25920=CARTESIAN_POINT('Ctrl Pts',(1.6128423401575,-1.,1.32683074483356));
#25921=CARTESIAN_POINT('Ctrl Pts',(1.6128423401575,1.,1.32683074483356));
#25922=CARTESIAN_POINT('Ctrl Pts',(1.61892832270724,-1.,1.32828000610449));
#25923=CARTESIAN_POINT('Ctrl Pts',(1.61892832270724,1.,1.32828000610449));
#25924=CARTESIAN_POINT('Ctrl Pts',(1.62503464209797,-1.,1.3296901950568));
#25925=CARTESIAN_POINT('Ctrl Pts',(1.62503464209797,1.,1.3296901950568));
#25926=CARTESIAN_POINT('Ctrl Pts',(1.63116079730923,-1.,1.33106149345645));
#25927=CARTESIAN_POINT('Ctrl Pts',(1.63116079730923,1.,1.33106149345645));
#25928=CARTESIAN_POINT('Ctrl Pts',(1.63730653475089,-1.,1.33239425103724));
#25929=CARTESIAN_POINT('Ctrl Pts',(1.63730653475089,1.,1.33239425103724));
#25930=CARTESIAN_POINT('Ctrl Pts',(1.6434717485603,-1.,1.33368890676572));
#25931=CARTESIAN_POINT('Ctrl Pts',(1.6434717485603,1.,1.33368890676572));
#25932=CARTESIAN_POINT('Ctrl Pts',(1.6496563728683,-1.,1.33494590467993));
#25933=CARTESIAN_POINT('Ctrl Pts',(1.6496563728683,1.,1.33494590467993));
#25934=CARTESIAN_POINT('Ctrl Pts',(1.65586025952593,-1.,1.33616559745172));
#25935=CARTESIAN_POINT('Ctrl Pts',(1.65586025952593,1.,1.33616559745172));
#25936=CARTESIAN_POINT('Ctrl Pts',(1.66208312541983,-1.,1.33734820885262));
#25937=CARTESIAN_POINT('Ctrl Pts',(1.66208312541983,1.,1.33734820885262));
#25938=CARTESIAN_POINT('Ctrl Pts',(1.66832460783989,-1.,1.33849388654388));
#25939=CARTESIAN_POINT('Ctrl Pts',(1.66832460783989,1.,1.33849388654388));
#25940=CARTESIAN_POINT('Ctrl Pts',(1.67458429426086,-1.,1.3396027347034));
#25941=CARTESIAN_POINT('Ctrl Pts',(1.67458429426086,1.,1.3396027347034));
#25942=CARTESIAN_POINT('Ctrl Pts',(1.68086176030362,-1.,1.34067485185203));
#25943=CARTESIAN_POINT('Ctrl Pts',(1.68086176030362,1.,1.34067485185203));
#25944=CARTESIAN_POINT('Ctrl Pts',(1.68715660868764,-1.,1.341710374848));
#25945=CARTESIAN_POINT('Ctrl Pts',(1.68715660868764,1.,1.341710374848));
#25946=CARTESIAN_POINT('Ctrl Pts',(1.6934684849687,-1.,1.34270948206319));
#25947=CARTESIAN_POINT('Ctrl Pts',(1.6934684849687,1.,1.34270948206319));
#25948=CARTESIAN_POINT('Ctrl Pts',(1.69979707754427,-1.,1.34367237124483));
#25949=CARTESIAN_POINT('Ctrl Pts',(1.69979707754427,1.,1.34367237124483));
#25950=CARTESIAN_POINT('Ctrl Pts',(1.70614212266738,-1.,1.34459924533831));
#25951=CARTESIAN_POINT('Ctrl Pts',(1.70614212266738,1.,1.34459924533831));
#25952=CARTESIAN_POINT('Ctrl Pts',(1.71250340686822,-1.,1.34549029589416));
#25953=CARTESIAN_POINT('Ctrl Pts',(1.71250340686822,1.,1.34549029589416));
#25954=CARTESIAN_POINT('Ctrl Pts',(1.7188807715049,-1.,1.34634568653227));
#25955=CARTESIAN_POINT('Ctrl Pts',(1.7188807715049,1.,1.34634568653227));
#25956=CARTESIAN_POINT('Ctrl Pts',(1.72527410680674,-1.,1.34716554819527));
#25957=CARTESIAN_POINT('Ctrl Pts',(1.72527410680674,1.,1.34716554819527));
#25958=CARTESIAN_POINT('Ctrl Pts',(1.7304014965394,-1.,1.34779309152035));
#25959=CARTESIAN_POINT('Ctrl Pts',(1.7304014965394,1.,1.34779309152035));
#25960=CARTESIAN_POINT('Ctrl Pts',(1.73425417885907,-1.,1.34824783112887));
#25961=CARTESIAN_POINT('Ctrl Pts',(1.73425417885907,1.,1.34824783112887));
#25962=CARTESIAN_POINT('Ctrl Pts',(1.73682580585691,-1.,1.34854391898045));
#25963=CARTESIAN_POINT('Ctrl Pts',(1.73682580585691,1.,1.34854391898045));
#25964=CARTESIAN_POINT('Ctrl Pts',(1.73811241238545,-1.,1.34869019493419));
#25965=CARTESIAN_POINT('Ctrl Pts',(1.73811241238545,1.,1.34869019493419));
#25966=CARTESIAN_POINT('',(1.31362392696032,1.,1.15624053661742));
#25967=CARTESIAN_POINT('Ctrl Pts',(1.31362392696032,1.,1.15624053661742));
#25968=CARTESIAN_POINT('Ctrl Pts',(1.31722977216397,1.,1.15950888730809));
#25969=CARTESIAN_POINT('Ctrl Pts',(1.32428080721772,1.,1.16589330093588));
#25970=CARTESIAN_POINT('Ctrl Pts',(1.33437539347008,1.,1.17501305789857));
#25971=CARTESIAN_POINT('Ctrl Pts',(1.34687054001093,1.,1.18625865667441));
#25972=CARTESIAN_POINT('Ctrl Pts',(1.36088705043885,1.,1.1987959077932));
#25973=CARTESIAN_POINT('Ctrl Pts',(1.37331915607905,1.,1.20982812925645));
#25974=CARTESIAN_POINT('Ctrl Pts',(1.38420564527715,1.,1.21938737280852));
#25975=CARTESIAN_POINT('Ctrl Pts',(1.39361389568796,1.,1.22752961899387));
#25976=CARTESIAN_POINT('Ctrl Pts',(1.40164708206106,1.,1.23434087290423));
#25977=CARTESIAN_POINT('Ctrl Pts',(1.40845295531283,1.,1.23994455029534));
#25978=CARTESIAN_POINT('Ctrl Pts',(1.41422913175179,1.,1.24450600513056));
#25979=CARTESIAN_POINT('Ctrl Pts',(1.41923722596025,1.,1.24824430986571));
#25980=CARTESIAN_POINT('Ctrl Pts',(1.42378102115575,1.,1.2514145557001));
#25981=CARTESIAN_POINT('Ctrl Pts',(1.42815938799387,1.,1.25426945222639));
#25982=CARTESIAN_POINT('Ctrl Pts',(1.43262645609691,1.,1.25702687965755));
#25983=CARTESIAN_POINT('Ctrl Pts',(1.43734919180847,1.,1.25983531012005));
#25984=CARTESIAN_POINT('Ctrl Pts',(1.44236470511303,1.,1.26273903323859));
#25985=CARTESIAN_POINT('Ctrl Pts',(1.44761985001662,1.,1.26570925118868));
#25986=CARTESIAN_POINT('Ctrl Pts',(1.45301422764247,1.,1.2686778680489));
#25987=CARTESIAN_POINT('Ctrl Pts',(1.45843906294697,1.,1.27156805265289));
#25988=CARTESIAN_POINT('Ctrl Pts',(1.46382431332476,1.,1.27433119897822));
#25989=CARTESIAN_POINT('Ctrl Pts',(1.46916035917133,1.,1.2769641483109));
#25990=CARTESIAN_POINT('Ctrl Pts',(1.4744717526707,1.,1.2794891824849));
#25991=CARTESIAN_POINT('Ctrl Pts',(1.47980070347095,1.,1.28194158939517));
#25992=CARTESIAN_POINT('Ctrl Pts',(1.4851881711891,1.,1.28435533880201));
#25993=CARTESIAN_POINT('Ctrl Pts',(1.4906522831278,1.,1.2867467611644));
#25994=CARTESIAN_POINT('Ctrl Pts',(1.49618896881754,1.,1.28911506584254));
#25995=CARTESIAN_POINT('Ctrl Pts',(1.50178230149776,1.,1.29145022885181));
#25996=CARTESIAN_POINT('Ctrl Pts',(1.50741159078365,1.,1.29373841372842));
#25997=CARTESIAN_POINT('Ctrl Pts',(1.51305994241402,1.,1.29596850710509));
#25998=CARTESIAN_POINT('Ctrl Pts',(1.51872184912724,1.,1.29813791800747));
#25999=CARTESIAN_POINT('Ctrl Pts',(1.52439957861062,1.,1.30024984366328));
#26000=CARTESIAN_POINT('Ctrl Pts',(1.53009970283891,1.,1.30231064395568));
#26001=CARTESIAN_POINT('Ctrl Pts',(1.53582981268977,1.,1.30432735639489));
#26002=CARTESIAN_POINT('Ctrl Pts',(1.54159462645432,1.,1.30630475189556));
#26003=CARTESIAN_POINT('Ctrl Pts',(1.54739413957185,1.,1.30824393907473));
#26004=CARTESIAN_POINT('Ctrl Pts',(1.55322568759481,1.,1.31014393684222));
#26005=CARTESIAN_POINT('Ctrl Pts',(1.55908521254821,1.,1.31200264341696));
#26006=CARTESIAN_POINT('Ctrl Pts',(1.56496872402353,1.,1.31381795281002));
#26007=CARTESIAN_POINT('Ctrl Pts',(1.57087397835723,1.,1.31558903860016));
#26008=CARTESIAN_POINT('Ctrl Pts',(1.5768005650559,1.,1.31731642317187));
#26009=CARTESIAN_POINT('Ctrl Pts',(1.58274907898834,1.,1.31900135021432));
#26010=CARTESIAN_POINT('Ctrl Pts',(1.58872057258245,1.,1.32064537110892));
#26011=CARTESIAN_POINT('Ctrl Pts',(1.59471591079403,1.,1.32224985747682));
#26012=CARTESIAN_POINT('Ctrl Pts',(1.60073511858687,1.,1.32381550858256));
#26013=CARTESIAN_POINT('Ctrl Pts',(1.60677758290954,1.,1.32534250785782));
#26014=CARTESIAN_POINT('Ctrl Pts',(1.6128423401575,1.,1.32683074483356));
#26015=CARTESIAN_POINT('Ctrl Pts',(1.61892832270724,1.,1.32828000610449));
#26016=CARTESIAN_POINT('Ctrl Pts',(1.62503464209797,1.,1.3296901950568));
#26017=CARTESIAN_POINT('Ctrl Pts',(1.63116079730923,1.,1.33106149345645));
#26018=CARTESIAN_POINT('Ctrl Pts',(1.63730653475089,1.,1.33239425103724));
#26019=CARTESIAN_POINT('Ctrl Pts',(1.6434717485603,1.,1.33368890676572));
#26020=CARTESIAN_POINT('Ctrl Pts',(1.6496563728683,1.,1.33494590467993));
#26021=CARTESIAN_POINT('Ctrl Pts',(1.65586025952593,1.,1.33616559745172));
#26022=CARTESIAN_POINT('Ctrl Pts',(1.66208312541983,1.,1.33734820885262));
#26023=CARTESIAN_POINT('Ctrl Pts',(1.66832460783989,1.,1.33849388654388));
#26024=CARTESIAN_POINT('Ctrl Pts',(1.67458429426086,1.,1.3396027347034));
#26025=CARTESIAN_POINT('Ctrl Pts',(1.68086176030362,1.,1.34067485185203));
#26026=CARTESIAN_POINT('Ctrl Pts',(1.68715660868764,1.,1.341710374848));
#26027=CARTESIAN_POINT('Ctrl Pts',(1.6934684849687,1.,1.34270948206319));
#26028=CARTESIAN_POINT('Ctrl Pts',(1.69979707754427,1.,1.34367237124483));
#26029=CARTESIAN_POINT('Ctrl Pts',(1.70614212266738,1.,1.34459924533831));
#26030=CARTESIAN_POINT('Ctrl Pts',(1.71250340686822,1.,1.34549029589416));
#26031=CARTESIAN_POINT('Ctrl Pts',(1.7188807715049,1.,1.34634568653227));
#26032=CARTESIAN_POINT('Ctrl Pts',(1.72527410680674,1.,1.34716554819527));
#26033=CARTESIAN_POINT('Ctrl Pts',(1.7304014965394,1.,1.34779309152035));
#26034=CARTESIAN_POINT('Ctrl Pts',(1.73425417885907,1.,1.34824783112887));
#26035=CARTESIAN_POINT('Ctrl Pts',(1.73682580585691,1.,1.34854391898045));
#26036=CARTESIAN_POINT('Ctrl Pts',(1.73811241238545,1.,1.34869019493419));
#26037=CARTESIAN_POINT('',(1.31362392696032,0.,1.15624053661742));
#26038=CARTESIAN_POINT('Origin',(0.,0.,0.));
#26039=CARTESIAN_POINT('',(1.15624053661742,1.,1.31362392696033));
#26040=CARTESIAN_POINT('Origin',(0.,1.,0.));
#26041=CARTESIAN_POINT('',(1.15624053661742,0.,1.31362392696032));
#26042=CARTESIAN_POINT('Ctrl Pts',(1.34869019493419,-1.,1.73811241238545));
#26043=CARTESIAN_POINT('Ctrl Pts',(1.34869019493419,1.,1.73811241238545));
#26044=CARTESIAN_POINT('Ctrl Pts',(1.34854391898145,-1.,1.73682580585819));
#26045=CARTESIAN_POINT('Ctrl Pts',(1.34854391898145,1.,1.73682580585819));
#26046=CARTESIAN_POINT('Ctrl Pts',(1.34824783113158,-1.,1.73425417886255));
#26047=CARTESIAN_POINT('Ctrl Pts',(1.34824783113158,1.,1.73425417886255));
#26048=CARTESIAN_POINT('Ctrl Pts',(1.3477930915247,-1.,1.73040149654497));
#26049=CARTESIAN_POINT('Ctrl Pts',(1.3477930915247,1.,1.73040149654497));
#26050=CARTESIAN_POINT('Ctrl Pts',(1.34716554820013,-1.,1.72527410681298));
#26051=CARTESIAN_POINT('Ctrl Pts',(1.34716554820013,1.,1.72527410681298));
#26052=CARTESIAN_POINT('Ctrl Pts',(1.34634568653586,-1.,1.7188807715095));
#26053=CARTESIAN_POINT('Ctrl Pts',(1.34634568653586,1.,1.7188807715095));
#26054=CARTESIAN_POINT('Ctrl Pts',(1.34549029589563,-1.,1.71250340687011));
#26055=CARTESIAN_POINT('Ctrl Pts',(1.34549029589563,1.,1.71250340687011));
#26056=CARTESIAN_POINT('Ctrl Pts',(1.34459924533783,-1.,1.70614212266676));
#26057=CARTESIAN_POINT('Ctrl Pts',(1.34459924533783,1.,1.70614212266676));
#26058=CARTESIAN_POINT('Ctrl Pts',(1.34367237124322,-1.,1.69979707754221));
#26059=CARTESIAN_POINT('Ctrl Pts',(1.34367237124322,1.,1.69979707754221));
#26060=CARTESIAN_POINT('Ctrl Pts',(1.34270948206139,-1.,1.6934684849664));
#26061=CARTESIAN_POINT('Ctrl Pts',(1.34270948206139,1.,1.6934684849664));
#26062=CARTESIAN_POINT('Ctrl Pts',(1.34171037484673,-1.,1.68715660868602));
#26063=CARTESIAN_POINT('Ctrl Pts',(1.34171037484673,1.,1.68715660868602));
#26064=CARTESIAN_POINT('Ctrl Pts',(1.3406748518516,-1.,1.68086176030308));
#26065=CARTESIAN_POINT('Ctrl Pts',(1.3406748518516,1.,1.68086176030308));
#26066=CARTESIAN_POINT('Ctrl Pts',(1.33960273470372,-1.,1.67458429426126));
#26067=CARTESIAN_POINT('Ctrl Pts',(1.33960273470372,1.,1.67458429426126));
#26068=CARTESIAN_POINT('Ctrl Pts',(1.33849388654458,-1.,1.66832460784078));
#26069=CARTESIAN_POINT('Ctrl Pts',(1.33849388654458,1.,1.66832460784078));
#26070=CARTESIAN_POINT('Ctrl Pts',(1.33734820885331,-1.,1.66208312542073));
#26071=CARTESIAN_POINT('Ctrl Pts',(1.33734820885331,1.,1.66208312542073));
#26072=CARTESIAN_POINT('Ctrl Pts',(1.33616559745217,-1.,1.65586025952651));
#26073=CARTESIAN_POINT('Ctrl Pts',(1.33616559745217,1.,1.65586025952651));
#26074=CARTESIAN_POINT('Ctrl Pts',(1.33494590468003,-1.,1.64965637286843));
#26075=CARTESIAN_POINT('Ctrl Pts',(1.33494590468003,1.,1.64965637286843));
#26076=CARTESIAN_POINT('Ctrl Pts',(1.33368890676554,-1.,1.64347174856007));
#26077=CARTESIAN_POINT('Ctrl Pts',(1.33368890676554,1.,1.64347174856007));
#26078=CARTESIAN_POINT('Ctrl Pts',(1.33239425103694,-1.,1.6373065347505));
#26079=CARTESIAN_POINT('Ctrl Pts',(1.33239425103694,1.,1.6373065347505));
#26080=CARTESIAN_POINT('Ctrl Pts',(1.33106149345618,-1.,1.63116079730887));
#26081=CARTESIAN_POINT('Ctrl Pts',(1.33106149345618,1.,1.63116079730887));
#26082=CARTESIAN_POINT('Ctrl Pts',(1.32969019505665,-1.,1.62503464209777));
#26083=CARTESIAN_POINT('Ctrl Pts',(1.32969019505665,1.,1.62503464209777));
#26084=CARTESIAN_POINT('Ctrl Pts',(1.32828000610448,-1.,1.61892832270723));
#26085=CARTESIAN_POINT('Ctrl Pts',(1.32828000610448,1.,1.61892832270723));
#26086=CARTESIAN_POINT('Ctrl Pts',(1.32683074483365,-1.,1.61284234015762));
#26087=CARTESIAN_POINT('Ctrl Pts',(1.32683074483365,1.,1.61284234015762));
#26088=CARTESIAN_POINT('Ctrl Pts',(1.32534250785794,-1.,1.6067775829097));
#26089=CARTESIAN_POINT('Ctrl Pts',(1.32534250785794,1.,1.6067775829097));
#26090=CARTESIAN_POINT('Ctrl Pts',(1.32381550858266,-1.,1.600735118587));
#26091=CARTESIAN_POINT('Ctrl Pts',(1.32381550858266,1.,1.600735118587));
#26092=CARTESIAN_POINT('Ctrl Pts',(1.32224985747686,-1.,1.59471591079408));
#26093=CARTESIAN_POINT('Ctrl Pts',(1.32224985747686,1.,1.59471591079408));
#26094=CARTESIAN_POINT('Ctrl Pts',(1.32064537110891,-1.,1.58872057258244));
#26095=CARTESIAN_POINT('Ctrl Pts',(1.32064537110891,1.,1.58872057258244));
#26096=CARTESIAN_POINT('Ctrl Pts',(1.31900135021428,-1.,1.58274907898829));
#26097=CARTESIAN_POINT('Ctrl Pts',(1.31900135021428,1.,1.58274907898829));
#26098=CARTESIAN_POINT('Ctrl Pts',(1.31731642317183,-1.,1.57680056505585));
#26099=CARTESIAN_POINT('Ctrl Pts',(1.31731642317183,1.,1.57680056505585));
#26100=CARTESIAN_POINT('Ctrl Pts',(1.31558903860015,-1.,1.57087397835721));
#26101=CARTESIAN_POINT('Ctrl Pts',(1.31558903860015,1.,1.57087397835721));
#26102=CARTESIAN_POINT('Ctrl Pts',(1.31381795281002,-1.,1.56496872402352));
#26103=CARTESIAN_POINT('Ctrl Pts',(1.31381795281002,1.,1.56496872402352));
#26104=CARTESIAN_POINT('Ctrl Pts',(1.31200264341696,-1.,1.55908521254822));
#26105=CARTESIAN_POINT('Ctrl Pts',(1.31200264341696,1.,1.55908521254822));
#26106=CARTESIAN_POINT('Ctrl Pts',(1.31014393684221,-1.,1.55322568759481));
#26107=CARTESIAN_POINT('Ctrl Pts',(1.31014393684221,1.,1.55322568759481));
#26108=CARTESIAN_POINT('Ctrl Pts',(1.30824393907471,-1.,1.54739413957183));
#26109=CARTESIAN_POINT('Ctrl Pts',(1.30824393907471,1.,1.54739413957183));
#26110=CARTESIAN_POINT('Ctrl Pts',(1.30630475189553,-1.,1.54159462645428));
#26111=CARTESIAN_POINT('Ctrl Pts',(1.30630475189553,1.,1.54159462645428));
#26112=CARTESIAN_POINT('Ctrl Pts',(1.30432735639487,-1.,1.53582981268976));
#26113=CARTESIAN_POINT('Ctrl Pts',(1.30432735639487,1.,1.53582981268976));
#26114=CARTESIAN_POINT('Ctrl Pts',(1.3023106439557,-1.,1.53009970283893));
#26115=CARTESIAN_POINT('Ctrl Pts',(1.3023106439557,1.,1.53009970283893));
#26116=CARTESIAN_POINT('Ctrl Pts',(1.30024984366334,-1.,1.5243995786107));
#26117=CARTESIAN_POINT('Ctrl Pts',(1.30024984366334,1.,1.5243995786107));
#26118=CARTESIAN_POINT('Ctrl Pts',(1.29813791800757,-1.,1.51872184912735));
#26119=CARTESIAN_POINT('Ctrl Pts',(1.29813791800757,1.,1.51872184912735));
#26120=CARTESIAN_POINT('Ctrl Pts',(1.29596850710518,-1.,1.51305994241412));
#26121=CARTESIAN_POINT('Ctrl Pts',(1.29596850710518,1.,1.51305994241412));
#26122=CARTESIAN_POINT('Ctrl Pts',(1.29373841372843,-1.,1.50741159078367));
#26123=CARTESIAN_POINT('Ctrl Pts',(1.29373841372843,1.,1.50741159078367));
#26124=CARTESIAN_POINT('Ctrl Pts',(1.29145022885171,-1.,1.50178230149764));
#26125=CARTESIAN_POINT('Ctrl Pts',(1.29145022885171,1.,1.50178230149764));
#26126=CARTESIAN_POINT('Ctrl Pts',(1.28911506584232,-1.,1.49618896881729));
#26127=CARTESIAN_POINT('Ctrl Pts',(1.28911506584232,1.,1.49618896881729));
#26128=CARTESIAN_POINT('Ctrl Pts',(1.28674676116415,-1.,1.4906522831275));
#26129=CARTESIAN_POINT('Ctrl Pts',(1.28674676116415,1.,1.4906522831275));
#26130=CARTESIAN_POINT('Ctrl Pts',(1.28435533880184,-1.,1.48518817118891));
#26131=CARTESIAN_POINT('Ctrl Pts',(1.28435533880184,1.,1.48518817118891));
#26132=CARTESIAN_POINT('Ctrl Pts',(1.28194158939522,-1.,1.47980070347102));
#26133=CARTESIAN_POINT('Ctrl Pts',(1.28194158939522,1.,1.47980070347102));
#26134=CARTESIAN_POINT('Ctrl Pts',(1.27948918248524,-1.,1.4744717526711));
#26135=CARTESIAN_POINT('Ctrl Pts',(1.27948918248524,1.,1.4744717526711));
#26136=CARTESIAN_POINT('Ctrl Pts',(1.27696414831144,-1.,1.46916035917197));
#26137=CARTESIAN_POINT('Ctrl Pts',(1.27696414831144,1.,1.46916035917197));
#26138=CARTESIAN_POINT('Ctrl Pts',(1.27433119897877,-1.,1.4638243133254));
#26139=CARTESIAN_POINT('Ctrl Pts',(1.27433119897877,1.,1.4638243133254));
#26140=CARTESIAN_POINT('Ctrl Pts',(1.27156805265312,-1.,1.45843906294725));
#26141=CARTESIAN_POINT('Ctrl Pts',(1.27156805265312,1.,1.45843906294725));
#26142=CARTESIAN_POINT('Ctrl Pts',(1.26867786804854,-1.,1.45301422764205));
#26143=CARTESIAN_POINT('Ctrl Pts',(1.26867786804854,1.,1.45301422764205));
#26144=CARTESIAN_POINT('Ctrl Pts',(1.26570925118767,-1.,1.44761985001544));
#26145=CARTESIAN_POINT('Ctrl Pts',(1.26570925118767,1.,1.44761985001544));
#26146=CARTESIAN_POINT('Ctrl Pts',(1.26273903323723,-1.,1.44236470511145));
#26147=CARTESIAN_POINT('Ctrl Pts',(1.26273903323723,1.,1.44236470511145));
#26148=CARTESIAN_POINT('Ctrl Pts',(1.25983531011894,-1.,1.43734919180719));
#26149=CARTESIAN_POINT('Ctrl Pts',(1.25983531011894,1.,1.43734919180719));
#26150=CARTESIAN_POINT('Ctrl Pts',(1.25702687965744,-1.,1.43262645609679));
#26151=CARTESIAN_POINT('Ctrl Pts',(1.25702687965744,1.,1.43262645609679));
#26152=CARTESIAN_POINT('Ctrl Pts',(1.25426945222783,-1.,1.42815938799555));
#26153=CARTESIAN_POINT('Ctrl Pts',(1.25426945222783,1.,1.42815938799555));
#26154=CARTESIAN_POINT('Ctrl Pts',(1.25141455570299,-1.,1.42378102115911));
#26155=CARTESIAN_POINT('Ctrl Pts',(1.25141455570299,1.,1.42378102115911));
#26156=CARTESIAN_POINT('Ctrl Pts',(1.24824430986911,-1.,1.41923722596421));
#26157=CARTESIAN_POINT('Ctrl Pts',(1.24824430986911,1.,1.41923722596421));
#26158=CARTESIAN_POINT('Ctrl Pts',(1.24450600513278,-1.,1.41422913175437));
#26159=CARTESIAN_POINT('Ctrl Pts',(1.24450600513278,1.,1.41422913175437));
#26160=CARTESIAN_POINT('Ctrl Pts',(1.23994455029421,-1.,1.40845295531151));
#26161=CARTESIAN_POINT('Ctrl Pts',(1.23994455029421,1.,1.40845295531151));
#26162=CARTESIAN_POINT('Ctrl Pts',(1.23434087289768,-1.,1.40164708205345));
#26163=CARTESIAN_POINT('Ctrl Pts',(1.23434087289768,1.,1.40164708205345));
#26164=CARTESIAN_POINT('Ctrl Pts',(1.22752961898063,-1.,1.39361389567257));
#26165=CARTESIAN_POINT('Ctrl Pts',(1.22752961898063,1.,1.39361389567257));
#26166=CARTESIAN_POINT('Ctrl Pts',(1.21938737278853,-1.,1.38420564525391));
#26167=CARTESIAN_POINT('Ctrl Pts',(1.21938737278853,1.,1.38420564525391));
#26168=CARTESIAN_POINT('Ctrl Pts',(1.20982812923113,-1.,1.37331915604962));
#26169=CARTESIAN_POINT('Ctrl Pts',(1.20982812923113,1.,1.37331915604962));
#26170=CARTESIAN_POINT('Ctrl Pts',(1.1987959077656,-1.,1.36088705040677));
#26171=CARTESIAN_POINT('Ctrl Pts',(1.1987959077656,1.,1.36088705040677));
#26172=CARTESIAN_POINT('Ctrl Pts',(1.18625865664915,-1.,1.34687053998157));
#26173=CARTESIAN_POINT('Ctrl Pts',(1.18625865664915,1.,1.34687053998157));
#26174=CARTESIAN_POINT('Ctrl Pts',(1.17501305787994,-1.,1.33437539344842));
#26175=CARTESIAN_POINT('Ctrl Pts',(1.17501305787994,1.,1.33437539344842));
#26176=CARTESIAN_POINT('Ctrl Pts',(1.16589330092532,-1.,1.32428080720544));
#26177=CARTESIAN_POINT('Ctrl Pts',(1.16589330092532,1.,1.32428080720544));
#26178=CARTESIAN_POINT('Ctrl Pts',(1.15950888730433,-1.,1.3172297721596));
#26179=CARTESIAN_POINT('Ctrl Pts',(1.15950888730433,1.,1.3172297721596));
#26180=CARTESIAN_POINT('Ctrl Pts',(1.15624053661742,-1.,1.31362392696033));
#26181=CARTESIAN_POINT('Ctrl Pts',(1.15624053661742,1.,1.31362392696033));
#26182=CARTESIAN_POINT('',(1.34869019493419,1.,1.73811241238545));
#26183=CARTESIAN_POINT('Ctrl Pts',(1.34869019493419,1.,1.73811241238545));
#26184=CARTESIAN_POINT('Ctrl Pts',(1.34854391898145,1.,1.73682580585819));
#26185=CARTESIAN_POINT('Ctrl Pts',(1.34824783113158,1.,1.73425417886255));
#26186=CARTESIAN_POINT('Ctrl Pts',(1.3477930915247,1.,1.73040149654497));
#26187=CARTESIAN_POINT('Ctrl Pts',(1.34716554820013,1.,1.72527410681298));
#26188=CARTESIAN_POINT('Ctrl Pts',(1.34634568653586,1.,1.7188807715095));
#26189=CARTESIAN_POINT('Ctrl Pts',(1.34549029589563,1.,1.71250340687011));
#26190=CARTESIAN_POINT('Ctrl Pts',(1.34459924533783,1.,1.70614212266676));
#26191=CARTESIAN_POINT('Ctrl Pts',(1.34367237124322,1.,1.69979707754221));
#26192=CARTESIAN_POINT('Ctrl Pts',(1.34270948206139,1.,1.6934684849664));
#26193=CARTESIAN_POINT('Ctrl Pts',(1.34171037484673,1.,1.68715660868602));
#26194=CARTESIAN_POINT('Ctrl Pts',(1.3406748518516,1.,1.68086176030308));
#26195=CARTESIAN_POINT('Ctrl Pts',(1.33960273470372,1.,1.67458429426126));
#26196=CARTESIAN_POINT('Ctrl Pts',(1.33849388654458,1.,1.66832460784078));
#26197=CARTESIAN_POINT('Ctrl Pts',(1.33734820885331,1.,1.66208312542073));
#26198=CARTESIAN_POINT('Ctrl Pts',(1.33616559745217,1.,1.65586025952651));
#26199=CARTESIAN_POINT('Ctrl Pts',(1.33494590468003,1.,1.64965637286843));
#26200=CARTESIAN_POINT('Ctrl Pts',(1.33368890676554,1.,1.64347174856007));
#26201=CARTESIAN_POINT('Ctrl Pts',(1.33239425103694,1.,1.6373065347505));
#26202=CARTESIAN_POINT('Ctrl Pts',(1.33106149345618,1.,1.63116079730887));
#26203=CARTESIAN_POINT('Ctrl Pts',(1.32969019505665,1.,1.62503464209777));
#26204=CARTESIAN_POINT('Ctrl Pts',(1.32828000610448,1.,1.61892832270723));
#26205=CARTESIAN_POINT('Ctrl Pts',(1.32683074483365,1.,1.61284234015762));
#26206=CARTESIAN_POINT('Ctrl Pts',(1.32534250785794,1.,1.6067775829097));
#26207=CARTESIAN_POINT('Ctrl Pts',(1.32381550858266,1.,1.600735118587));
#26208=CARTESIAN_POINT('Ctrl Pts',(1.32224985747686,1.,1.59471591079408));
#26209=CARTESIAN_POINT('Ctrl Pts',(1.32064537110891,1.,1.58872057258244));
#26210=CARTESIAN_POINT('Ctrl Pts',(1.31900135021428,1.,1.58274907898829));
#26211=CARTESIAN_POINT('Ctrl Pts',(1.31731642317183,1.,1.57680056505585));
#26212=CARTESIAN_POINT('Ctrl Pts',(1.31558903860015,1.,1.57087397835721));
#26213=CARTESIAN_POINT('Ctrl Pts',(1.31381795281002,1.,1.56496872402352));
#26214=CARTESIAN_POINT('Ctrl Pts',(1.31200264341696,1.,1.55908521254822));
#26215=CARTESIAN_POINT('Ctrl Pts',(1.31014393684221,1.,1.55322568759481));
#26216=CARTESIAN_POINT('Ctrl Pts',(1.30824393907471,1.,1.54739413957183));
#26217=CARTESIAN_POINT('Ctrl Pts',(1.30630475189553,1.,1.54159462645428));
#26218=CARTESIAN_POINT('Ctrl Pts',(1.30432735639487,1.,1.53582981268976));
#26219=CARTESIAN_POINT('Ctrl Pts',(1.3023106439557,1.,1.53009970283893));
#26220=CARTESIAN_POINT('Ctrl Pts',(1.30024984366334,1.,1.5243995786107));
#26221=CARTESIAN_POINT('Ctrl Pts',(1.29813791800757,1.,1.51872184912735));
#26222=CARTESIAN_POINT('Ctrl Pts',(1.29596850710518,1.,1.51305994241412));
#26223=CARTESIAN_POINT('Ctrl Pts',(1.29373841372843,1.,1.50741159078367));
#26224=CARTESIAN_POINT('Ctrl Pts',(1.29145022885171,1.,1.50178230149764));
#26225=CARTESIAN_POINT('Ctrl Pts',(1.28911506584232,1.,1.49618896881729));
#26226=CARTESIAN_POINT('Ctrl Pts',(1.28674676116415,1.,1.4906522831275));
#26227=CARTESIAN_POINT('Ctrl Pts',(1.28435533880184,1.,1.48518817118891));
#26228=CARTESIAN_POINT('Ctrl Pts',(1.28194158939522,1.,1.47980070347102));
#26229=CARTESIAN_POINT('Ctrl Pts',(1.27948918248524,1.,1.4744717526711));
#26230=CARTESIAN_POINT('Ctrl Pts',(1.27696414831144,1.,1.46916035917197));
#26231=CARTESIAN_POINT('Ctrl Pts',(1.27433119897877,1.,1.4638243133254));
#26232=CARTESIAN_POINT('Ctrl Pts',(1.27156805265312,1.,1.45843906294725));
#26233=CARTESIAN_POINT('Ctrl Pts',(1.26867786804854,1.,1.45301422764205));
#26234=CARTESIAN_POINT('Ctrl Pts',(1.26570925118767,1.,1.44761985001544));
#26235=CARTESIAN_POINT('Ctrl Pts',(1.26273903323723,1.,1.44236470511145));
#26236=CARTESIAN_POINT('Ctrl Pts',(1.25983531011894,1.,1.43734919180719));
#26237=CARTESIAN_POINT('Ctrl Pts',(1.25702687965744,1.,1.43262645609679));
#26238=CARTESIAN_POINT('Ctrl Pts',(1.25426945222783,1.,1.42815938799555));
#26239=CARTESIAN_POINT('Ctrl Pts',(1.25141455570299,1.,1.42378102115911));
#26240=CARTESIAN_POINT('Ctrl Pts',(1.24824430986911,1.,1.41923722596421));
#26241=CARTESIAN_POINT('Ctrl Pts',(1.24450600513278,1.,1.41422913175437));
#26242=CARTESIAN_POINT('Ctrl Pts',(1.23994455029421,1.,1.40845295531151));
#26243=CARTESIAN_POINT('Ctrl Pts',(1.23434087289768,1.,1.40164708205345));
#26244=CARTESIAN_POINT('Ctrl Pts',(1.22752961898063,1.,1.39361389567257));
#26245=CARTESIAN_POINT('Ctrl Pts',(1.21938737278853,1.,1.38420564525391));
#26246=CARTESIAN_POINT('Ctrl Pts',(1.20982812923113,1.,1.37331915604962));
#26247=CARTESIAN_POINT('Ctrl Pts',(1.1987959077656,1.,1.36088705040677));
#26248=CARTESIAN_POINT('Ctrl Pts',(1.18625865664915,1.,1.34687053998157));
#26249=CARTESIAN_POINT('Ctrl Pts',(1.17501305787994,1.,1.33437539344842));
#26250=CARTESIAN_POINT('Ctrl Pts',(1.16589330092532,1.,1.32428080720544));
#26251=CARTESIAN_POINT('Ctrl Pts',(1.15950888730433,1.,1.3172297721596));
#26252=CARTESIAN_POINT('Ctrl Pts',(1.15624053661742,1.,1.31362392696033));
#26253=CARTESIAN_POINT('',(1.34869019493419,0.,1.73811241238545));
#26254=CARTESIAN_POINT('Origin',(1.23627494547115,0.,1.81978687191668));
#26255=CARTESIAN_POINT('',(1.23627494547115,1.,1.81978687191668));
#26256=CARTESIAN_POINT('',(1.34869019493419,1.,1.73811241238545));
#26257=CARTESIAN_POINT('',(1.23627494547115,0.,1.81978687191668));
#26258=CARTESIAN_POINT('Ctrl Pts',(0.892032620296855,-1.,1.5055822144029));
#26259=CARTESIAN_POINT('Ctrl Pts',(0.892032620296855,1.,1.5055822144029));
#26260=CARTESIAN_POINT('Ctrl Pts',(0.894452006967538,-1.,1.50980486807181));
#26261=CARTESIAN_POINT('Ctrl Pts',(0.894452006967538,1.,1.50980486807181));
#26262=CARTESIAN_POINT('Ctrl Pts',(0.89918504749193,-1.,1.51805569591479));
#26263=CARTESIAN_POINT('Ctrl Pts',(0.89918504749193,1.,1.51805569591479));
#26264=CARTESIAN_POINT('Ctrl Pts',(0.905967409640498,-1.,1.52984849890434));
#26265=CARTESIAN_POINT('Ctrl Pts',(0.905967409640498,1.,1.52984849890434));
#26266=CARTESIAN_POINT('Ctrl Pts',(0.914375919046579,-1.,1.54440491152808));
#26267=CARTESIAN_POINT('Ctrl Pts',(0.914375919046579,1.,1.54440491152808));
#26268=CARTESIAN_POINT('Ctrl Pts',(0.923832188966322,-1.,1.56065988582509));
#26269=CARTESIAN_POINT('Ctrl Pts',(0.923832188966322,1.,1.56065988582509));
#26270=CARTESIAN_POINT('Ctrl Pts',(0.932246680128848,-1.,1.57499388385561));
#26271=CARTESIAN_POINT('Ctrl Pts',(0.932246680128848,1.,1.57499388385561));
#26272=CARTESIAN_POINT('Ctrl Pts',(0.939646377909319,-1.,1.58744937489796));
#26273=CARTESIAN_POINT('Ctrl Pts',(0.939646377909319,1.,1.58744937489796));
#26274=CARTESIAN_POINT('Ctrl Pts',(0.946078063325795,-1.,1.59810042045408));
#26275=CARTESIAN_POINT('Ctrl Pts',(0.946078063325795,1.,1.59810042045408));
#26276=CARTESIAN_POINT('Ctrl Pts',(0.951613284361247,-1.,1.60706069897794));
#26277=CARTESIAN_POINT('Ctrl Pts',(0.951613284361247,1.,1.60706069897794));
#26278=CARTESIAN_POINT('Ctrl Pts',(0.956354422921572,-1.,1.61449324337233));
#26279=CARTESIAN_POINT('Ctrl Pts',(0.956354422921572,1.,1.61449324337233));
#26280=CARTESIAN_POINT('Ctrl Pts',(0.960438326099958,-1.,1.62061638139929));
#26281=CARTESIAN_POINT('Ctrl Pts',(0.960438326099958,1.,1.62061638139929));
#26282=CARTESIAN_POINT('Ctrl Pts',(0.964046107037821,-1.,1.6257193066974));
#26283=CARTESIAN_POINT('Ctrl Pts',(0.964046107037821,1.,1.6257193066974));
#26284=CARTESIAN_POINT('Ctrl Pts',(0.967387853228041,-1.,1.63013849959083));
#26285=CARTESIAN_POINT('Ctrl Pts',(0.967387853228041,1.,1.63013849959083));
#26286=CARTESIAN_POINT('Ctrl Pts',(0.970669715996356,-1.,1.63420665729609));
#26287=CARTESIAN_POINT('Ctrl Pts',(0.970669715996356,1.,1.63420665729609));
#26288=CARTESIAN_POINT('Ctrl Pts',(0.974066058287501,-1.,1.63820952658157));
#26289=CARTESIAN_POINT('Ctrl Pts',(0.974066058287501,1.,1.63820952658157));
#26290=CARTESIAN_POINT('Ctrl Pts',(0.977689794120296,-1.,1.64233990826831));
#26291=CARTESIAN_POINT('Ctrl Pts',(0.977689794120296,1.,1.64233990826831));
#26292=CARTESIAN_POINT('Ctrl Pts',(0.981562530940574,-1.,1.64665139190834));
#26293=CARTESIAN_POINT('Ctrl Pts',(0.981562530940574,1.,1.64665139190834));
#26294=CARTESIAN_POINT('Ctrl Pts',(0.985642622921626,-1.,1.6511001661277));
#26295=CARTESIAN_POINT('Ctrl Pts',(0.985642622921626,1.,1.6511001661277));
#26296=CARTESIAN_POINT('Ctrl Pts',(0.98985562785445,-1.,1.65559044289746));
#26297=CARTESIAN_POINT('Ctrl Pts',(0.98985562785445,1.,1.65559044289746));
#26298=CARTESIAN_POINT('Ctrl Pts',(0.994121836661115,-1.,1.66001553809916));
#26299=CARTESIAN_POINT('Ctrl Pts',(0.994121836661115,1.,1.66001553809916));
#26300=CARTESIAN_POINT('Ctrl Pts',(0.998389654952317,-1.,1.66430758030304));
#26301=CARTESIAN_POINT('Ctrl Pts',(0.998389654952317,1.,1.66430758030304));
#26302=CARTESIAN_POINT('Ctrl Pts',(1.00265091003682,-1.,1.66846059277231));
#26303=CARTESIAN_POINT('Ctrl Pts',(1.00265091003682,1.,1.66846059277231));
#26304=CARTESIAN_POINT('Ctrl Pts',(1.00692206696387,-1.,1.67250335383248));
#26305=CARTESIAN_POINT('Ctrl Pts',(1.00692206696387,1.,1.67250335383248));
#26306=CARTESIAN_POINT('Ctrl Pts',(1.01123236493507,-1.,1.67648246776457));
#26307=CARTESIAN_POINT('Ctrl Pts',(1.01123236493507,1.,1.67648246776457));
#26308=CARTESIAN_POINT('Ctrl Pts',(1.01561026162786,-1.,1.6804428989482));
#26309=CARTESIAN_POINT('Ctrl Pts',(1.01561026162786,1.,1.6804428989482));
#26310=CARTESIAN_POINT('Ctrl Pts',(1.02006795074222,-1.,1.68440578021739));
#26311=CARTESIAN_POINT('Ctrl Pts',(1.02006795074222,1.,1.68440578021739));
#26312=CARTESIAN_POINT('Ctrl Pts',(1.02460180535272,-1.,1.68836910178475));
#26313=CARTESIAN_POINT('Ctrl Pts',(1.02460180535272,1.,1.68836910178475));
#26314=CARTESIAN_POINT('Ctrl Pts',(1.02919977579155,-1.,1.69231840863471));
#26315=CARTESIAN_POINT('Ctrl Pts',(1.02919977579155,1.,1.69231840863471));
#26316=CARTESIAN_POINT('Ctrl Pts',(1.03384646003587,-1.,1.69623414782769));
#26317=CARTESIAN_POINT('Ctrl Pts',(1.03384646003587,1.,1.69623414782769));
#26318=CARTESIAN_POINT('Ctrl Pts',(1.03852922490782,-1.,1.70010052930951));
#26319=CARTESIAN_POINT('Ctrl Pts',(1.03852922490782,1.,1.70010052930951));
#26320=CARTESIAN_POINT('Ctrl Pts',(1.04324363334546,-1.,1.70391338707969));
#26321=CARTESIAN_POINT('Ctrl Pts',(1.04324363334546,1.,1.70391338707969));
#26322=CARTESIAN_POINT('Ctrl Pts',(1.0479908540499,-1.,1.70767646263641));
#26323=CARTESIAN_POINT('Ctrl Pts',(1.0479908540499,1.,1.70767646263641));
#26324=CARTESIAN_POINT('Ctrl Pts',(1.05277517202853,-1.,1.71139783543986));
#26325=CARTESIAN_POINT('Ctrl Pts',(1.05277517202853,1.,1.71139783543986));
#26326=CARTESIAN_POINT('Ctrl Pts',(1.05760163192481,-1.,1.71508654427022));
#26327=CARTESIAN_POINT('Ctrl Pts',(1.05760163192481,1.,1.71508654427022));
#26328=CARTESIAN_POINT('Ctrl Pts',(1.06247324680649,-1.,1.71874858456908));
#26329=CARTESIAN_POINT('Ctrl Pts',(1.06247324680649,1.,1.71874858456908));
#26330=CARTESIAN_POINT('Ctrl Pts',(1.06738966975463,-1.,1.72238500928456));
#26331=CARTESIAN_POINT('Ctrl Pts',(1.06738966975463,1.,1.72238500928456));
#26332=CARTESIAN_POINT('Ctrl Pts',(1.07234866990252,-1.,1.72599406198489));
#26333=CARTESIAN_POINT('Ctrl Pts',(1.07234866990252,1.,1.72599406198489));
#26334=CARTESIAN_POINT('Ctrl Pts',(1.0773470373727,-1.,1.72957248977424));
#26335=CARTESIAN_POINT('Ctrl Pts',(1.0773470373727,1.,1.72957248977424));
#26336=CARTESIAN_POINT('Ctrl Pts',(1.08238162784749,-1.,1.73311705663407));
#26337=CARTESIAN_POINT('Ctrl Pts',(1.08238162784749,1.,1.73311705663407));
#26338=CARTESIAN_POINT('Ctrl Pts',(1.08745056285429,-1.,1.73662628326093));
#26339=CARTESIAN_POINT('Ctrl Pts',(1.08745056285429,1.,1.73662628326093));
#26340=CARTESIAN_POINT('Ctrl Pts',(1.09255329056496,-1.,1.74010053962252));
#26341=CARTESIAN_POINT('Ctrl Pts',(1.09255329056496,1.,1.74010053962252));
#26342=CARTESIAN_POINT('Ctrl Pts',(1.09768999241229,-1.,1.74354119236212));
#26343=CARTESIAN_POINT('Ctrl Pts',(1.09768999241229,1.,1.74354119236212));
#26344=CARTESIAN_POINT('Ctrl Pts',(1.10286118991144,-1.,1.74695004214924));
#26345=CARTESIAN_POINT('Ctrl Pts',(1.10286118991144,1.,1.74695004214924));
#26346=CARTESIAN_POINT('Ctrl Pts',(1.10806728183003,-1.,1.75032866075914));
#26347=CARTESIAN_POINT('Ctrl Pts',(1.10806728183003,1.,1.75032866075914));
#26348=CARTESIAN_POINT('Ctrl Pts',(1.11330807582542,-1.,1.75367772094617));
#26349=CARTESIAN_POINT('Ctrl Pts',(1.11330807582542,1.,1.75367772094617));
#26350=CARTESIAN_POINT('Ctrl Pts',(1.11858293216752,-1.,1.75699720772089));
#26351=CARTESIAN_POINT('Ctrl Pts',(1.11858293216752,1.,1.75699720772089));
#26352=CARTESIAN_POINT('Ctrl Pts',(1.12389096855078,-1.,1.76028671825084));
#26353=CARTESIAN_POINT('Ctrl Pts',(1.12389096855078,1.,1.76028671825084));
#26354=CARTESIAN_POINT('Ctrl Pts',(1.12923123555076,-1.,1.76354571966171));
#26355=CARTESIAN_POINT('Ctrl Pts',(1.12923123555076,1.,1.76354571966171));
#26356=CARTESIAN_POINT('Ctrl Pts',(1.13460291804634,-1.,1.76677384551883));
#26357=CARTESIAN_POINT('Ctrl Pts',(1.13460291804634,1.,1.76677384551883));
#26358=CARTESIAN_POINT('Ctrl Pts',(1.14000548337,-1.,1.76997111386806));
#26359=CARTESIAN_POINT('Ctrl Pts',(1.14000548337,1.,1.76997111386806));
#26360=CARTESIAN_POINT('Ctrl Pts',(1.14543858226948,-1.,1.77313777896234));
#26361=CARTESIAN_POINT('Ctrl Pts',(1.14543858226948,1.,1.77313777896234));
#26362=CARTESIAN_POINT('Ctrl Pts',(1.15090197841531,-1.,1.77627422557034));
#26363=CARTESIAN_POINT('Ctrl Pts',(1.15090197841531,1.,1.77627422557034));
#26364=CARTESIAN_POINT('Ctrl Pts',(1.15639547194689,-1.,1.77938085564261));
#26365=CARTESIAN_POINT('Ctrl Pts',(1.15639547194689,1.,1.77938085564261));
#26366=CARTESIAN_POINT('Ctrl Pts',(1.16191881298458,-1.,1.78245795880949));
#26367=CARTESIAN_POINT('Ctrl Pts',(1.16191881298458,1.,1.78245795880949));
#26368=CARTESIAN_POINT('Ctrl Pts',(1.16747166312239,-1.,1.78550566040349));
#26369=CARTESIAN_POINT('Ctrl Pts',(1.16747166312239,1.,1.78550566040349));
#26370=CARTESIAN_POINT('Ctrl Pts',(1.17305363177265,-1.,1.78852398877523));
#26371=CARTESIAN_POINT('Ctrl Pts',(1.17305363177265,1.,1.78852398877523));
#26372=CARTESIAN_POINT('Ctrl Pts',(1.17866429440781,-1.,1.79151291552646));
#26373=CARTESIAN_POINT('Ctrl Pts',(1.17866429440781,1.,1.79151291552646));
#26374=CARTESIAN_POINT('Ctrl Pts',(1.18430321697471,-1.,1.79447240321572));
#26375=CARTESIAN_POINT('Ctrl Pts',(1.18430321697471,1.,1.79447240321572));
#26376=CARTESIAN_POINT('Ctrl Pts',(1.1899699793456,-1.,1.79740245923649));
#26377=CARTESIAN_POINT('Ctrl Pts',(1.1899699793456,1.,1.79740245923649));
#26378=CARTESIAN_POINT('Ctrl Pts',(1.19566418930405,-1.,1.80030314370121));
#26379=CARTESIAN_POINT('Ctrl Pts',(1.19566418930405,1.,1.80030314370121));
#26380=CARTESIAN_POINT('Ctrl Pts',(1.2013854893912,-1.,1.8031745483882));
#26381=CARTESIAN_POINT('Ctrl Pts',(1.2013854893912,1.,1.8031745483882));
#26382=CARTESIAN_POINT('Ctrl Pts',(1.20713356605519,-1.,1.80601678480772));
#26383=CARTESIAN_POINT('Ctrl Pts',(1.20713356605519,1.,1.80601678480772));
#26384=CARTESIAN_POINT('Ctrl Pts',(1.2129081570818,-1.,1.80882996916931));
#26385=CARTESIAN_POINT('Ctrl Pts',(1.2129081570818,1.,1.80882996916931));
#26386=CARTESIAN_POINT('Ctrl Pts',(1.2187090610323,-1.,1.81161420806172));
#26387=CARTESIAN_POINT('Ctrl Pts',(1.2187090610323,1.,1.81161420806172));
#26388=CARTESIAN_POINT('Ctrl Pts',(1.22453613304507,-1.,1.81436959209778));
#26389=CARTESIAN_POINT('Ctrl Pts',(1.22453613304507,1.,1.81436959209778));
#26390=CARTESIAN_POINT('Ctrl Pts',(1.22921864890975,-1.,1.81655087183054));
#26391=CARTESIAN_POINT('Ctrl Pts',(1.22921864890975,1.,1.81655087183054));
#26392=CARTESIAN_POINT('Ctrl Pts',(1.23274224526804,-1.,1.81817389920914));
#26393=CARTESIAN_POINT('Ctrl Pts',(1.23274224526804,1.,1.81817389920914));
#26394=CARTESIAN_POINT('Ctrl Pts',(1.23509651170384,-1.,1.81925017193531));
#26395=CARTESIAN_POINT('Ctrl Pts',(1.23509651170384,1.,1.81925017193531));
#26396=CARTESIAN_POINT('Ctrl Pts',(1.23627494547115,-1.,1.81978687191668));
#26397=CARTESIAN_POINT('Ctrl Pts',(1.23627494547115,1.,1.81978687191668));
#26398=CARTESIAN_POINT('',(0.892032620296855,1.,1.5055822144029));
#26399=CARTESIAN_POINT('Ctrl Pts',(0.892032620296855,1.,1.5055822144029));
#26400=CARTESIAN_POINT('Ctrl Pts',(0.894452006967538,1.,1.50980486807181));
#26401=CARTESIAN_POINT('Ctrl Pts',(0.89918504749193,1.,1.51805569591479));
#26402=CARTESIAN_POINT('Ctrl Pts',(0.905967409640498,1.,1.52984849890434));
#26403=CARTESIAN_POINT('Ctrl Pts',(0.914375919046579,1.,1.54440491152808));
#26404=CARTESIAN_POINT('Ctrl Pts',(0.923832188966322,1.,1.56065988582509));
#26405=CARTESIAN_POINT('Ctrl Pts',(0.932246680128848,1.,1.57499388385561));
#26406=CARTESIAN_POINT('Ctrl Pts',(0.939646377909319,1.,1.58744937489796));
#26407=CARTESIAN_POINT('Ctrl Pts',(0.946078063325795,1.,1.59810042045408));
#26408=CARTESIAN_POINT('Ctrl Pts',(0.951613284361247,1.,1.60706069897794));
#26409=CARTESIAN_POINT('Ctrl Pts',(0.956354422921572,1.,1.61449324337233));
#26410=CARTESIAN_POINT('Ctrl Pts',(0.960438326099958,1.,1.62061638139929));
#26411=CARTESIAN_POINT('Ctrl Pts',(0.964046107037821,1.,1.6257193066974));
#26412=CARTESIAN_POINT('Ctrl Pts',(0.967387853228041,1.,1.63013849959083));
#26413=CARTESIAN_POINT('Ctrl Pts',(0.970669715996356,1.,1.63420665729609));
#26414=CARTESIAN_POINT('Ctrl Pts',(0.974066058287501,1.,1.63820952658157));
#26415=CARTESIAN_POINT('Ctrl Pts',(0.977689794120296,1.,1.64233990826831));
#26416=CARTESIAN_POINT('Ctrl Pts',(0.981562530940574,1.,1.64665139190834));
#26417=CARTESIAN_POINT('Ctrl Pts',(0.985642622921626,1.,1.6511001661277));
#26418=CARTESIAN_POINT('Ctrl Pts',(0.98985562785445,1.,1.65559044289746));
#26419=CARTESIAN_POINT('Ctrl Pts',(0.994121836661115,1.,1.66001553809916));
#26420=CARTESIAN_POINT('Ctrl Pts',(0.998389654952317,1.,1.66430758030304));
#26421=CARTESIAN_POINT('Ctrl Pts',(1.00265091003682,1.,1.66846059277231));
#26422=CARTESIAN_POINT('Ctrl Pts',(1.00692206696387,1.,1.67250335383248));
#26423=CARTESIAN_POINT('Ctrl Pts',(1.01123236493507,1.,1.67648246776457));
#26424=CARTESIAN_POINT('Ctrl Pts',(1.01561026162786,1.,1.6804428989482));
#26425=CARTESIAN_POINT('Ctrl Pts',(1.02006795074222,1.,1.68440578021739));
#26426=CARTESIAN_POINT('Ctrl Pts',(1.02460180535272,1.,1.68836910178475));
#26427=CARTESIAN_POINT('Ctrl Pts',(1.02919977579155,1.,1.69231840863471));
#26428=CARTESIAN_POINT('Ctrl Pts',(1.03384646003587,1.,1.69623414782769));
#26429=CARTESIAN_POINT('Ctrl Pts',(1.03852922490782,1.,1.70010052930951));
#26430=CARTESIAN_POINT('Ctrl Pts',(1.04324363334546,1.,1.70391338707969));
#26431=CARTESIAN_POINT('Ctrl Pts',(1.0479908540499,1.,1.70767646263641));
#26432=CARTESIAN_POINT('Ctrl Pts',(1.05277517202853,1.,1.71139783543986));
#26433=CARTESIAN_POINT('Ctrl Pts',(1.05760163192481,1.,1.71508654427022));
#26434=CARTESIAN_POINT('Ctrl Pts',(1.06247324680649,1.,1.71874858456908));
#26435=CARTESIAN_POINT('Ctrl Pts',(1.06738966975463,1.,1.72238500928456));
#26436=CARTESIAN_POINT('Ctrl Pts',(1.07234866990252,1.,1.72599406198489));
#26437=CARTESIAN_POINT('Ctrl Pts',(1.0773470373727,1.,1.72957248977424));
#26438=CARTESIAN_POINT('Ctrl Pts',(1.08238162784749,1.,1.73311705663407));
#26439=CARTESIAN_POINT('Ctrl Pts',(1.08745056285429,1.,1.73662628326093));
#26440=CARTESIAN_POINT('Ctrl Pts',(1.09255329056496,1.,1.74010053962252));
#26441=CARTESIAN_POINT('Ctrl Pts',(1.09768999241229,1.,1.74354119236212));
#26442=CARTESIAN_POINT('Ctrl Pts',(1.10286118991144,1.,1.74695004214924));
#26443=CARTESIAN_POINT('Ctrl Pts',(1.10806728183003,1.,1.75032866075914));
#26444=CARTESIAN_POINT('Ctrl Pts',(1.11330807582542,1.,1.75367772094617));
#26445=CARTESIAN_POINT('Ctrl Pts',(1.11858293216752,1.,1.75699720772089));
#26446=CARTESIAN_POINT('Ctrl Pts',(1.12389096855078,1.,1.76028671825084));
#26447=CARTESIAN_POINT('Ctrl Pts',(1.12923123555076,1.,1.76354571966171));
#26448=CARTESIAN_POINT('Ctrl Pts',(1.13460291804634,1.,1.76677384551883));
#26449=CARTESIAN_POINT('Ctrl Pts',(1.14000548337,1.,1.76997111386806));
#26450=CARTESIAN_POINT('Ctrl Pts',(1.14543858226948,1.,1.77313777896234));
#26451=CARTESIAN_POINT('Ctrl Pts',(1.15090197841531,1.,1.77627422557034));
#26452=CARTESIAN_POINT('Ctrl Pts',(1.15639547194689,1.,1.77938085564261));
#26453=CARTESIAN_POINT('Ctrl Pts',(1.16191881298458,1.,1.78245795880949));
#26454=CARTESIAN_POINT('Ctrl Pts',(1.16747166312239,1.,1.78550566040349));
#26455=CARTESIAN_POINT('Ctrl Pts',(1.17305363177265,1.,1.78852398877523));
#26456=CARTESIAN_POINT('Ctrl Pts',(1.17866429440781,1.,1.79151291552646));
#26457=CARTESIAN_POINT('Ctrl Pts',(1.18430321697471,1.,1.79447240321572));
#26458=CARTESIAN_POINT('Ctrl Pts',(1.1899699793456,1.,1.79740245923649));
#26459=CARTESIAN_POINT('Ctrl Pts',(1.19566418930405,1.,1.80030314370121));
#26460=CARTESIAN_POINT('Ctrl Pts',(1.2013854893912,1.,1.8031745483882));
#26461=CARTESIAN_POINT('Ctrl Pts',(1.20713356605519,1.,1.80601678480772));
#26462=CARTESIAN_POINT('Ctrl Pts',(1.2129081570818,1.,1.80882996916931));
#26463=CARTESIAN_POINT('Ctrl Pts',(1.2187090610323,1.,1.81161420806172));
#26464=CARTESIAN_POINT('Ctrl Pts',(1.22453613304507,1.,1.81436959209778));
#26465=CARTESIAN_POINT('Ctrl Pts',(1.22921864890975,1.,1.81655087183054));
#26466=CARTESIAN_POINT('Ctrl Pts',(1.23274224526804,1.,1.81817389920914));
#26467=CARTESIAN_POINT('Ctrl Pts',(1.23509651170384,1.,1.81925017193531));
#26468=CARTESIAN_POINT('Ctrl Pts',(1.23627494547115,1.,1.81978687191668));
#26469=CARTESIAN_POINT('',(0.892032620296854,0.,1.5055822144029));
#26470=CARTESIAN_POINT('Origin',(0.,0.,0.));
#26471=CARTESIAN_POINT('',(0.693717979106305,1.,1.60662857109684));
#26472=CARTESIAN_POINT('Origin',(0.,1.,0.));
#26473=CARTESIAN_POINT('',(0.693717979106305,0.,1.60662857109684));
#26474=CARTESIAN_POINT('Ctrl Pts',(0.7455743247944,-1.,2.0698113262342));
#26475=CARTESIAN_POINT('Ctrl Pts',(0.7455743247944,1.,2.0698113262342));
#26476=CARTESIAN_POINT('Ctrl Pts',(0.745832791378367,-1.,2.06854248895728));
#26477=CARTESIAN_POINT('Ctrl Pts',(0.745832791378367,1.,2.06854248895728));
#26478=CARTESIAN_POINT('Ctrl Pts',(0.7463458715442,-1.,2.06600523016815));
#26479=CARTESIAN_POINT('Ctrl Pts',(0.7463458715442,1.,2.06600523016815));
#26480=CARTESIAN_POINT('Ctrl Pts',(0.747103932787919,-1.,2.06220058927826));
#26481=CARTESIAN_POINT('Ctrl Pts',(0.747103932787919,1.,2.06220058927826));
#26482=CARTESIAN_POINT('Ctrl Pts',(0.748091554183802,-1.,2.05713023031007));
#26483=CARTESIAN_POINT('Ctrl Pts',(0.748091554183802,1.,2.05713023031007));
#26484=CARTESIAN_POINT('Ctrl Pts',(0.749287468665046,-1.,2.05079645592154));
#26485=CARTESIAN_POINT('Ctrl Pts',(0.749287468665046,1.,2.05079645592154));
#26486=CARTESIAN_POINT('Ctrl Pts',(0.750444657875575,-1.,2.04446689147979));
#26487=CARTESIAN_POINT('Ctrl Pts',(0.750444657875575,1.,2.04446689147979));
#26488=CARTESIAN_POINT('Ctrl Pts',(0.751562963361115,-1.,2.03814160092099));
#26489=CARTESIAN_POINT('Ctrl Pts',(0.751562963361115,1.,2.03814160092099));
#26490=CARTESIAN_POINT('Ctrl Pts',(0.75264218048721,-1.,2.03182068456221));
#26491=CARTESIAN_POINT('Ctrl Pts',(0.75264218048721,1.,2.03182068456221));
#26492=CARTESIAN_POINT('Ctrl Pts',(0.753682061112768,-1.,2.02550428623313));
#26493=CARTESIAN_POINT('Ctrl Pts',(0.753682061112768,1.,2.02550428623313));
#26494=CARTESIAN_POINT('Ctrl Pts',(0.754682330722816,-1.,2.01919259405809));
#26495=CARTESIAN_POINT('Ctrl Pts',(0.754682330722816,1.,2.01919259405809));
#26496=CARTESIAN_POINT('Ctrl Pts',(0.755642704957865,-1.,2.01288584328084));
#26497=CARTESIAN_POINT('Ctrl Pts',(0.755642704957865,1.,2.01288584328084));
#26498=CARTESIAN_POINT('Ctrl Pts',(0.75656290464667,-1.,2.0065843158773));
#26499=CARTESIAN_POINT('Ctrl Pts',(0.75656290464667,1.,2.0065843158773));
#26500=CARTESIAN_POINT('Ctrl Pts',(0.757442676862724,-1.,2.00028834739178));
#26501=CARTESIAN_POINT('Ctrl Pts',(0.757442676862724,1.,2.00028834739178));
#26502=CARTESIAN_POINT('Ctrl Pts',(0.758281796766761,-1.,1.99399831098817));
#26503=CARTESIAN_POINT('Ctrl Pts',(0.758281796766761,1.,1.99399831098817));
#26504=CARTESIAN_POINT('Ctrl Pts',(0.759080037802488,-1.,1.98771456680874));
#26505=CARTESIAN_POINT('Ctrl Pts',(0.759080037802488,1.,1.98771456680874));
#26506=CARTESIAN_POINT('Ctrl Pts',(0.75983714745219,-1.,1.98143741418172));
#26507=CARTESIAN_POINT('Ctrl Pts',(0.75983714745219,1.,1.98143741418172));
#26508=CARTESIAN_POINT('Ctrl Pts',(0.760552825409757,-1.,1.97516705321494));
#26509=CARTESIAN_POINT('Ctrl Pts',(0.760552825409757,1.,1.97516705321494));
#26510=CARTESIAN_POINT('Ctrl Pts',(0.76122669048382,-1.,1.96890351582499));
#26511=CARTESIAN_POINT('Ctrl Pts',(0.76122669048382,1.,1.96890351582499));
#26512=CARTESIAN_POINT('Ctrl Pts',(0.761858300014423,-1.,1.96264672744186));
#26513=CARTESIAN_POINT('Ctrl Pts',(0.761858300014423,1.,1.96264672744186));
#26514=CARTESIAN_POINT('Ctrl Pts',(0.762447203806178,-1.,1.95639665309869));
#26515=CARTESIAN_POINT('Ctrl Pts',(0.762447203806178,1.,1.95639665309869));
#26516=CARTESIAN_POINT('Ctrl Pts',(0.762992990878769,-1.,1.95015342590024));
#26517=CARTESIAN_POINT('Ctrl Pts',(0.762992990878769,1.,1.95015342590024));
#26518=CARTESIAN_POINT('Ctrl Pts',(0.763495333538629,-1.,1.9439174661764));
#26519=CARTESIAN_POINT('Ctrl Pts',(0.763495333538629,1.,1.9439174661764));
#26520=CARTESIAN_POINT('Ctrl Pts',(0.763954049121458,-1.,1.93768964875886));
#26521=CARTESIAN_POINT('Ctrl Pts',(0.763954049121458,1.,1.93768964875886));
#26522=CARTESIAN_POINT('Ctrl Pts',(0.76436901067394,-1.,1.93147105496382));
#26523=CARTESIAN_POINT('Ctrl Pts',(0.76436901067394,1.,1.93147105496382));
#26524=CARTESIAN_POINT('Ctrl Pts',(0.764740025488211,-1.,1.92526263537048));
#26525=CARTESIAN_POINT('Ctrl Pts',(0.764740025488211,1.,1.92526263537048));
#26526=CARTESIAN_POINT('Ctrl Pts',(0.765066729667088,-1.,1.91906491634196));
#26527=CARTESIAN_POINT('Ctrl Pts',(0.765066729667088,1.,1.91906491634196));
#26528=CARTESIAN_POINT('Ctrl Pts',(0.765348465884722,-1.,1.91287765805169));
#26529=CARTESIAN_POINT('Ctrl Pts',(0.765348465884722,1.,1.91287765805169));
#26530=CARTESIAN_POINT('Ctrl Pts',(0.765584196937919,-1.,1.90669961402356));
#26531=CARTESIAN_POINT('Ctrl Pts',(0.765584196937919,1.,1.90669961402356));
#26532=CARTESIAN_POINT('Ctrl Pts',(0.765772772593386,-1.,1.90052930393596));
#26533=CARTESIAN_POINT('Ctrl Pts',(0.765772772593386,1.,1.90052930393596));
#26534=CARTESIAN_POINT('Ctrl Pts',(0.765913193856978,-1.,1.89436577771388));
#26535=CARTESIAN_POINT('Ctrl Pts',(0.765913193856978,1.,1.89436577771388));
#26536=CARTESIAN_POINT('Ctrl Pts',(0.766004837062091,-1.,1.88820926433409));
#26537=CARTESIAN_POINT('Ctrl Pts',(0.766004837062091,1.,1.88820926433409));
#26538=CARTESIAN_POINT('Ctrl Pts',(0.766047794851864,-1.,1.88206215302561));
#26539=CARTESIAN_POINT('Ctrl Pts',(0.766047794851864,1.,1.88206215302561));
#26540=CARTESIAN_POINT('Ctrl Pts',(0.766042837036744,-1.,1.87592888967883));
#26541=CARTESIAN_POINT('Ctrl Pts',(0.766042837036744,1.,1.87592888967883));
#26542=CARTESIAN_POINT('Ctrl Pts',(0.765990708546091,-1.,1.86981398314341));
#26543=CARTESIAN_POINT('Ctrl Pts',(0.765990708546091,1.,1.86981398314341));
#26544=CARTESIAN_POINT('Ctrl Pts',(0.765891519092547,-1.,1.86372027063312));
#26545=CARTESIAN_POINT('Ctrl Pts',(0.765891519092547,1.,1.86372027063312));
#26546=CARTESIAN_POINT('Ctrl Pts',(0.765744212909318,-1.,1.85764741390394));
#26547=CARTESIAN_POINT('Ctrl Pts',(0.765744212909318,1.,1.85764741390394));
#26548=CARTESIAN_POINT('Ctrl Pts',(0.765545710619062,-1.,1.85158945130063));
#26549=CARTESIAN_POINT('Ctrl Pts',(0.765545710619062,1.,1.85158945130063));
#26550=CARTESIAN_POINT('Ctrl Pts',(0.765291664862029,-1.,1.84553698875924));
#26551=CARTESIAN_POINT('Ctrl Pts',(0.765291664862029,1.,1.84553698875924));
#26552=CARTESIAN_POINT('Ctrl Pts',(0.764978057881737,-1.,1.83948181064835));
#26553=CARTESIAN_POINT('Ctrl Pts',(0.764978057881737,1.,1.83948181064835));
#26554=CARTESIAN_POINT('Ctrl Pts',(0.764602549687853,-1.,1.83342077227142));
#26555=CARTESIAN_POINT('Ctrl Pts',(0.764602549687853,1.,1.83342077227142));
#26556=CARTESIAN_POINT('Ctrl Pts',(0.764165902605995,-1.,1.82735991200065));
#26557=CARTESIAN_POINT('Ctrl Pts',(0.764165902605995,1.,1.82735991200065));
#26558=CARTESIAN_POINT('Ctrl Pts',(0.763673465462726,-1.,1.82131873145266));
#26559=CARTESIAN_POINT('Ctrl Pts',(0.763673465462726,1.,1.82131873145266));
#26560=CARTESIAN_POINT('Ctrl Pts',(0.763132003836634,-1.,1.8153211840553));
#26561=CARTESIAN_POINT('Ctrl Pts',(0.763132003836634,1.,1.8153211840553));
#26562=CARTESIAN_POINT('Ctrl Pts',(0.762546129463938,-1.,1.80938551463965));
#26563=CARTESIAN_POINT('Ctrl Pts',(0.762546129463938,1.,1.80938551463965));
#26564=CARTESIAN_POINT('Ctrl Pts',(0.761915336443547,-1.,1.80351583877342));
#26565=CARTESIAN_POINT('Ctrl Pts',(0.761915336443547,1.,1.80351583877342));
#26566=CARTESIAN_POINT('Ctrl Pts',(0.761229695230558,-1.,1.79768986997783));
#26567=CARTESIAN_POINT('Ctrl Pts',(0.761229695230558,1.,1.79768986997783));
#26568=CARTESIAN_POINT('Ctrl Pts',(0.760469555880749,-1.,1.7918581561088));
#26569=CARTESIAN_POINT('Ctrl Pts',(0.760469555880749,1.,1.7918581561088));
#26570=CARTESIAN_POINT('Ctrl Pts',(0.759614401110189,-1.,1.78596964884604));
#26571=CARTESIAN_POINT('Ctrl Pts',(0.759614401110189,1.,1.78596964884604));
#26572=CARTESIAN_POINT('Ctrl Pts',(0.758650626677518,-1.,1.77999411220945));
#26573=CARTESIAN_POINT('Ctrl Pts',(0.758650626677518,1.,1.77999411220945));
#26574=CARTESIAN_POINT('Ctrl Pts',(0.757578264077028,-1.,1.77394167108292));
#26575=CARTESIAN_POINT('Ctrl Pts',(0.757578264077028,1.,1.77394167108292));
#26576=CARTESIAN_POINT('Ctrl Pts',(0.75642189602781,-1.,1.76789396002998));
#26577=CARTESIAN_POINT('Ctrl Pts',(0.75642189602781,1.,1.76789396002998));
#26578=CARTESIAN_POINT('Ctrl Pts',(0.755220979974461,-1.,1.76197817240128));
#26579=CARTESIAN_POINT('Ctrl Pts',(0.755220979974461,1.,1.76197817240128));
#26580=CARTESIAN_POINT('Ctrl Pts',(0.754009254027828,-1.,1.75631083600019));
#26581=CARTESIAN_POINT('Ctrl Pts',(0.754009254027828,1.,1.75631083600019));
#26582=CARTESIAN_POINT('Ctrl Pts',(0.752797683531314,-1.,1.75095139468794));
#26583=CARTESIAN_POINT('Ctrl Pts',(0.752797683531314,1.,1.75095139468794));
#26584=CARTESIAN_POINT('Ctrl Pts',(0.751555614164482,-1.,1.74585086852502));
#26585=CARTESIAN_POINT('Ctrl Pts',(0.751555614164482,1.,1.74585086852502));
#26586=CARTESIAN_POINT('Ctrl Pts',(0.750193435981249,-1.,1.74080458267114));
#26587=CARTESIAN_POINT('Ctrl Pts',(0.750193435981249,1.,1.74080458267114));
#26588=CARTESIAN_POINT('Ctrl Pts',(0.74858246295687,-1.,1.7355035168033));
#26589=CARTESIAN_POINT('Ctrl Pts',(0.74858246295687,1.,1.7355035168033));
#26590=CARTESIAN_POINT('Ctrl Pts',(0.746574710097752,-1.,1.72958533647714));
#26591=CARTESIAN_POINT('Ctrl Pts',(0.746574710097752,1.,1.72958533647714));
#26592=CARTESIAN_POINT('Ctrl Pts',(0.744021445433093,-1.,1.72268229916769));
#26593=CARTESIAN_POINT('Ctrl Pts',(0.744021445433093,1.,1.72268229916769));
#26594=CARTESIAN_POINT('Ctrl Pts',(0.74079516202821,-1.,1.71447789751001));
#26595=CARTESIAN_POINT('Ctrl Pts',(0.74079516202821,1.,1.71447789751001));
#26596=CARTESIAN_POINT('Ctrl Pts',(0.736799665716932,-1.,1.70473309004249));
#26597=CARTESIAN_POINT('Ctrl Pts',(0.736799665716932,1.,1.70473309004249));
#26598=CARTESIAN_POINT('Ctrl Pts',(0.731963238685357,-1.,1.69326921972915));
#26599=CARTESIAN_POINT('Ctrl Pts',(0.731963238685357,1.,1.69326921972915));
#26600=CARTESIAN_POINT('Ctrl Pts',(0.726235967982445,-1.,1.67996158451922));
#26601=CARTESIAN_POINT('Ctrl Pts',(0.726235967982445,1.,1.67996158451922));
#26602=CARTESIAN_POINT('Ctrl Pts',(0.719585433787949,-1.,1.66472880551777));
#26603=CARTESIAN_POINT('Ctrl Pts',(0.719585433787949,1.,1.66472880551777));
#26604=CARTESIAN_POINT('Ctrl Pts',(0.711993139340447,-1.,1.64752408828442));
#26605=CARTESIAN_POINT('Ctrl Pts',(0.711993139340447,1.,1.64752408828442));
#26606=CARTESIAN_POINT('Ctrl Pts',(0.705159151977294,-1.,1.6321654166204));
#26607=CARTESIAN_POINT('Ctrl Pts',(0.705159151977294,1.,1.6321654166204));
#26608=CARTESIAN_POINT('Ctrl Pts',(0.699605146398836,-1.,1.61974673471117));
#26609=CARTESIAN_POINT('Ctrl Pts',(0.699605146398836,1.,1.61974673471117));
#26610=CARTESIAN_POINT('Ctrl Pts',(0.69571209787897,-1.,1.61106790957619));
#26611=CARTESIAN_POINT('Ctrl Pts',(0.69571209787897,1.,1.61106790957619));
#26612=CARTESIAN_POINT('Ctrl Pts',(0.693717979106305,-1.,1.60662857109684));
#26613=CARTESIAN_POINT('Ctrl Pts',(0.693717979106305,1.,1.60662857109684));
#26614=CARTESIAN_POINT('',(0.7455743247944,1.,2.0698113262342));
#26615=CARTESIAN_POINT('Ctrl Pts',(0.7455743247944,1.,2.0698113262342));
#26616=CARTESIAN_POINT('Ctrl Pts',(0.745832791378367,1.,2.06854248895728));
#26617=CARTESIAN_POINT('Ctrl Pts',(0.7463458715442,1.,2.06600523016815));
#26618=CARTESIAN_POINT('Ctrl Pts',(0.747103932787919,1.,2.06220058927826));
#26619=CARTESIAN_POINT('Ctrl Pts',(0.748091554183802,1.,2.05713023031007));
#26620=CARTESIAN_POINT('Ctrl Pts',(0.749287468665046,1.,2.05079645592154));
#26621=CARTESIAN_POINT('Ctrl Pts',(0.750444657875575,1.,2.04446689147979));
#26622=CARTESIAN_POINT('Ctrl Pts',(0.751562963361115,1.,2.03814160092099));
#26623=CARTESIAN_POINT('Ctrl Pts',(0.75264218048721,1.,2.03182068456221));
#26624=CARTESIAN_POINT('Ctrl Pts',(0.753682061112768,1.,2.02550428623313));
#26625=CARTESIAN_POINT('Ctrl Pts',(0.754682330722816,1.,2.01919259405809));
#26626=CARTESIAN_POINT('Ctrl Pts',(0.755642704957865,1.,2.01288584328084));
#26627=CARTESIAN_POINT('Ctrl Pts',(0.75656290464667,1.,2.0065843158773));
#26628=CARTESIAN_POINT('Ctrl Pts',(0.757442676862724,1.,2.00028834739178));
#26629=CARTESIAN_POINT('Ctrl Pts',(0.758281796766761,1.,1.99399831098817));
#26630=CARTESIAN_POINT('Ctrl Pts',(0.759080037802488,1.,1.98771456680874));
#26631=CARTESIAN_POINT('Ctrl Pts',(0.75983714745219,1.,1.98143741418172));
#26632=CARTESIAN_POINT('Ctrl Pts',(0.760552825409757,1.,1.97516705321494));
#26633=CARTESIAN_POINT('Ctrl Pts',(0.76122669048382,1.,1.96890351582499));
#26634=CARTESIAN_POINT('Ctrl Pts',(0.761858300014423,1.,1.96264672744186));
#26635=CARTESIAN_POINT('Ctrl Pts',(0.762447203806178,1.,1.95639665309869));
#26636=CARTESIAN_POINT('Ctrl Pts',(0.762992990878769,1.,1.95015342590024));
#26637=CARTESIAN_POINT('Ctrl Pts',(0.763495333538629,1.,1.9439174661764));
#26638=CARTESIAN_POINT('Ctrl Pts',(0.763954049121458,1.,1.93768964875886));
#26639=CARTESIAN_POINT('Ctrl Pts',(0.76436901067394,1.,1.93147105496382));
#26640=CARTESIAN_POINT('Ctrl Pts',(0.764740025488211,1.,1.92526263537048));
#26641=CARTESIAN_POINT('Ctrl Pts',(0.765066729667088,1.,1.91906491634196));
#26642=CARTESIAN_POINT('Ctrl Pts',(0.765348465884722,1.,1.91287765805169));
#26643=CARTESIAN_POINT('Ctrl Pts',(0.765584196937919,1.,1.90669961402356));
#26644=CARTESIAN_POINT('Ctrl Pts',(0.765772772593386,1.,1.90052930393596));
#26645=CARTESIAN_POINT('Ctrl Pts',(0.765913193856978,1.,1.89436577771388));
#26646=CARTESIAN_POINT('Ctrl Pts',(0.766004837062091,1.,1.88820926433409));
#26647=CARTESIAN_POINT('Ctrl Pts',(0.766047794851864,1.,1.88206215302561));
#26648=CARTESIAN_POINT('Ctrl Pts',(0.766042837036744,1.,1.87592888967883));
#26649=CARTESIAN_POINT('Ctrl Pts',(0.765990708546091,1.,1.86981398314341));
#26650=CARTESIAN_POINT('Ctrl Pts',(0.765891519092547,1.,1.86372027063312));
#26651=CARTESIAN_POINT('Ctrl Pts',(0.765744212909318,1.,1.85764741390394));
#26652=CARTESIAN_POINT('Ctrl Pts',(0.765545710619062,1.,1.85158945130063));
#26653=CARTESIAN_POINT('Ctrl Pts',(0.765291664862029,1.,1.84553698875924));
#26654=CARTESIAN_POINT('Ctrl Pts',(0.764978057881737,1.,1.83948181064835));
#26655=CARTESIAN_POINT('Ctrl Pts',(0.764602549687853,1.,1.83342077227142));
#26656=CARTESIAN_POINT('Ctrl Pts',(0.764165902605995,1.,1.82735991200065));
#26657=CARTESIAN_POINT('Ctrl Pts',(0.763673465462726,1.,1.82131873145266));
#26658=CARTESIAN_POINT('Ctrl Pts',(0.763132003836634,1.,1.8153211840553));
#26659=CARTESIAN_POINT('Ctrl Pts',(0.762546129463938,1.,1.80938551463965));
#26660=CARTESIAN_POINT('Ctrl Pts',(0.761915336443547,1.,1.80351583877342));
#26661=CARTESIAN_POINT('Ctrl Pts',(0.761229695230558,1.,1.79768986997783));
#26662=CARTESIAN_POINT('Ctrl Pts',(0.760469555880749,1.,1.7918581561088));
#26663=CARTESIAN_POINT('Ctrl Pts',(0.759614401110189,1.,1.78596964884604));
#26664=CARTESIAN_POINT('Ctrl Pts',(0.758650626677518,1.,1.77999411220945));
#26665=CARTESIAN_POINT('Ctrl Pts',(0.757578264077028,1.,1.77394167108292));
#26666=CARTESIAN_POINT('Ctrl Pts',(0.75642189602781,1.,1.76789396002998));
#26667=CARTESIAN_POINT('Ctrl Pts',(0.755220979974461,1.,1.76197817240128));
#26668=CARTESIAN_POINT('Ctrl Pts',(0.754009254027828,1.,1.75631083600019));
#26669=CARTESIAN_POINT('Ctrl Pts',(0.752797683531314,1.,1.75095139468794));
#26670=CARTESIAN_POINT('Ctrl Pts',(0.751555614164482,1.,1.74585086852502));
#26671=CARTESIAN_POINT('Ctrl Pts',(0.750193435981249,1.,1.74080458267114));
#26672=CARTESIAN_POINT('Ctrl Pts',(0.74858246295687,1.,1.7355035168033));
#26673=CARTESIAN_POINT('Ctrl Pts',(0.746574710097752,1.,1.72958533647714));
#26674=CARTESIAN_POINT('Ctrl Pts',(0.744021445433093,1.,1.72268229916769));
#26675=CARTESIAN_POINT('Ctrl Pts',(0.74079516202821,1.,1.71447789751001));
#26676=CARTESIAN_POINT('Ctrl Pts',(0.736799665716932,1.,1.70473309004249));
#26677=CARTESIAN_POINT('Ctrl Pts',(0.731963238685357,1.,1.69326921972915));
#26678=CARTESIAN_POINT('Ctrl Pts',(0.726235967982445,1.,1.67996158451922));
#26679=CARTESIAN_POINT('Ctrl Pts',(0.719585433787949,1.,1.66472880551777));
#26680=CARTESIAN_POINT('Ctrl Pts',(0.711993139340447,1.,1.64752408828442));
#26681=CARTESIAN_POINT('Ctrl Pts',(0.705159151977294,1.,1.6321654166204));
#26682=CARTESIAN_POINT('Ctrl Pts',(0.699605146398836,1.,1.61974673471117));
#26683=CARTESIAN_POINT('Ctrl Pts',(0.69571209787897,1.,1.61106790957619));
#26684=CARTESIAN_POINT('Ctrl Pts',(0.693717979106305,1.,1.60662857109684));
#26685=CARTESIAN_POINT('',(0.7455743247944,0.,2.0698113262342));
#26686=CARTESIAN_POINT('Origin',(0.61342227326009,0.,2.11275013067528));
#26687=CARTESIAN_POINT('',(0.61342227326009,1.,2.11275013067528));
#26688=CARTESIAN_POINT('',(0.7455743247944,1.,2.0698113262342));
#26689=CARTESIAN_POINT('',(0.61342227326009,0.,2.11275013067528));
#26690=CARTESIAN_POINT('Ctrl Pts',(0.383122945602004,-1.,1.7075470150345));
#26691=CARTESIAN_POINT('Ctrl Pts',(0.383122945602004,1.,1.7075470150345));
#26692=CARTESIAN_POINT('Ctrl Pts',(0.384119047315541,-1.,1.71231062891958));
#26693=CARTESIAN_POINT('Ctrl Pts',(0.384119047315541,1.,1.71231062891958));
#26694=CARTESIAN_POINT('Ctrl Pts',(0.38607079032701,-1.,1.72162022246158));
#26695=CARTESIAN_POINT('Ctrl Pts',(0.38607079032701,1.,1.72162022246158));
#26696=CARTESIAN_POINT('Ctrl Pts',(0.388877023509191,-1.,1.7349317097561));
#26697=CARTESIAN_POINT('Ctrl Pts',(0.388877023509191,1.,1.7349317097561));
#26698=CARTESIAN_POINT('Ctrl Pts',(0.392375812294307,-1.,1.75137405313962));
#26699=CARTESIAN_POINT('Ctrl Pts',(0.392375812294307,1.,1.75137405313962));
#26700=CARTESIAN_POINT('Ctrl Pts',(0.39634619612042,-1.,1.7697556004756));
#26701=CARTESIAN_POINT('Ctrl Pts',(0.39634619612042,1.,1.7697556004756));
#26702=CARTESIAN_POINT('Ctrl Pts',(0.39991940378308,-1.,1.78598826347533));
#26703=CARTESIAN_POINT('Ctrl Pts',(0.39991940378308,1.,1.78598826347533));
#26704=CARTESIAN_POINT('Ctrl Pts',(0.403107976170441,-1.,1.80012077176221));
#26705=CARTESIAN_POINT('Ctrl Pts',(0.403107976170441,1.,1.80012077176221));
#26706=CARTESIAN_POINT('Ctrl Pts',(0.405933518411838,-1.,1.81223801813988));
#26707=CARTESIAN_POINT('Ctrl Pts',(0.405933518411838,1.,1.81223801813988));
#26708=CARTESIAN_POINT('Ctrl Pts',(0.408428948108533,-1.,1.8224702267854));
#26709=CARTESIAN_POINT('Ctrl Pts',(0.408428948108533,1.,1.8224702267854));
#26710=CARTESIAN_POINT('Ctrl Pts',(0.410641256301674,-1.,1.83100408895216));
#26711=CARTESIAN_POINT('Ctrl Pts',(0.410641256301674,1.,1.83100408895216));
#26712=CARTESIAN_POINT('Ctrl Pts',(0.412633125322161,-1.,1.83808953475839));
#26713=CARTESIAN_POINT('Ctrl Pts',(0.412633125322161,1.,1.83808953475839));
#26714=CARTESIAN_POINT('Ctrl Pts',(0.41448743825434,-1.,1.8440575707371));
#26715=CARTESIAN_POINT('Ctrl Pts',(0.41448743825434,1.,1.8440575707371));
#26716=CARTESIAN_POINT('Ctrl Pts',(0.416300022038864,-1.,1.84929312929882));
#26717=CARTESIAN_POINT('Ctrl Pts',(0.416300022038864,1.,1.84929312929882));
#26718=CARTESIAN_POINT('Ctrl Pts',(0.418164129143534,-1.,1.85417632856234));
#26719=CARTESIAN_POINT('Ctrl Pts',(0.418164129143534,1.,1.85417632856234));
#26720=CARTESIAN_POINT('Ctrl Pts',(0.420157287975619,-1.,1.85903281096686));
#26721=CARTESIAN_POINT('Ctrl Pts',(0.420157287975619,1.,1.85903281096686));
#26722=CARTESIAN_POINT('Ctrl Pts',(0.422327307418275,-1.,1.86408083334028));
#26723=CARTESIAN_POINT('Ctrl Pts',(0.422327307418275,1.,1.86408083334028));
#26724=CARTESIAN_POINT('Ctrl Pts',(0.424678177291358,-1.,1.86937803944323));
#26725=CARTESIAN_POINT('Ctrl Pts',(0.424678177291358,1.,1.86937803944323));
#26726=CARTESIAN_POINT('Ctrl Pts',(0.427183828519102,-1.,1.87486989291484));
#26727=CARTESIAN_POINT('Ctrl Pts',(0.427183828519102,1.,1.87486989291484));
#26728=CARTESIAN_POINT('Ctrl Pts',(0.429803062482344,-1.,1.88044229001832));
#26729=CARTESIAN_POINT('Ctrl Pts',(0.429803062482344,1.,1.88044229001832));
#26730=CARTESIAN_POINT('Ctrl Pts',(0.432493038548748,-1.,1.88596913666793));
#26731=CARTESIAN_POINT('Ctrl Pts',(0.432493038548748,1.,1.88596913666793));
#26732=CARTESIAN_POINT('Ctrl Pts',(0.435225660963383,-1.,1.89136993975504));
#26733=CARTESIAN_POINT('Ctrl Pts',(0.435225660963383,1.,1.89136993975504));
#26734=CARTESIAN_POINT('Ctrl Pts',(0.437995003948244,-1.,1.89663648956466));
#26735=CARTESIAN_POINT('Ctrl Pts',(0.437995003948244,1.,1.89663648956466));
#26736=CARTESIAN_POINT('Ctrl Pts',(0.440807833704038,-1.,1.90180124389086));
#26737=CARTESIAN_POINT('Ctrl Pts',(0.440807833704038,1.,1.90180124389086));
#26738=CARTESIAN_POINT('Ctrl Pts',(0.44367755684915,-1.,1.90691756144898));
#26739=CARTESIAN_POINT('Ctrl Pts',(0.44367755684915,1.,1.90691756144898));
#26740=CARTESIAN_POINT('Ctrl Pts',(0.446617343485711,-1.,1.9120369998112));
#26741=CARTESIAN_POINT('Ctrl Pts',(0.446617343485711,1.,1.9120369998112));
#26742=CARTESIAN_POINT('Ctrl Pts',(0.449632260106662,-1.,1.91718342555755));
#26743=CARTESIAN_POINT('Ctrl Pts',(0.449632260106662,1.,1.91718342555755));
#26744=CARTESIAN_POINT('Ctrl Pts',(0.452719478359432,-1.,1.92235380648502));
#26745=CARTESIAN_POINT('Ctrl Pts',(0.452719478359432,1.,1.92235380648502));
#26746=CARTESIAN_POINT('Ctrl Pts',(0.45587200517437,-1.,1.92753067150476));
#26747=CARTESIAN_POINT('Ctrl Pts',(0.45587200517437,1.,1.92753067150476));
#26748=CARTESIAN_POINT('Ctrl Pts',(0.459081234547926,-1.,1.93269066517934));
#26749=CARTESIAN_POINT('Ctrl Pts',(0.459081234547926,1.,1.93269066517934));
#26750=CARTESIAN_POINT('Ctrl Pts',(0.462340031009056,-1.,1.93781486640821));
#26751=CARTESIAN_POINT('Ctrl Pts',(0.462340031009056,1.,1.93781486640821));
#26752=CARTESIAN_POINT('Ctrl Pts',(0.46564546202603,-1.,1.9428979419619));
#26753=CARTESIAN_POINT('Ctrl Pts',(0.46564546202603,1.,1.9428979419619));
#26754=CARTESIAN_POINT('Ctrl Pts',(0.468997482913135,-1.,1.94794381136514));
#26755=CARTESIAN_POINT('Ctrl Pts',(0.468997482913135,1.,1.94794381136514));
#26756=CARTESIAN_POINT('Ctrl Pts',(0.472397672264072,-1.,1.95296148278133));
#26757=CARTESIAN_POINT('Ctrl Pts',(0.472397672264072,1.,1.95296148278133));
#26758=CARTESIAN_POINT('Ctrl Pts',(0.475848034683176,-1.,1.95796111148177));
#26759=CARTESIAN_POINT('Ctrl Pts',(0.475848034683176,1.,1.95796111148177));
#26760=CARTESIAN_POINT('Ctrl Pts',(0.479349583074855,-1.,1.96294933055943));
#26761=CARTESIAN_POINT('Ctrl Pts',(0.479349583074855,1.,1.96294933055943));
#26762=CARTESIAN_POINT('Ctrl Pts',(0.48290166212069,-1.,1.96792703422362));
#26763=CARTESIAN_POINT('Ctrl Pts',(0.48290166212069,1.,1.96792703422362));
#26764=CARTESIAN_POINT('Ctrl Pts',(0.486502692907658,-1.,1.97289186263272));
#26765=CARTESIAN_POINT('Ctrl Pts',(0.486502692907658,1.,1.97289186263272));
#26766=CARTESIAN_POINT('Ctrl Pts',(0.490150627860952,-1.,1.97783973019229));
#26767=CARTESIAN_POINT('Ctrl Pts',(0.490150627860952,1.,1.97783973019229));
#26768=CARTESIAN_POINT('Ctrl Pts',(0.493843476541494,-1.,1.98276658761821));
#26769=CARTESIAN_POINT('Ctrl Pts',(0.493843476541494,1.,1.98276658761821));
#26770=CARTESIAN_POINT('Ctrl Pts',(0.497579909545574,-1.,1.98767044752932));
#26771=CARTESIAN_POINT('Ctrl Pts',(0.497579909545574,1.,1.98767044752932));
#26772=CARTESIAN_POINT('Ctrl Pts',(0.501359287727146,-1.,1.99255149126155));
#26773=CARTESIAN_POINT('Ctrl Pts',(0.501359287727146,1.,1.99255149126155));
#26774=CARTESIAN_POINT('Ctrl Pts',(0.505181361323026,-1.,1.99741107463572));
#26775=CARTESIAN_POINT('Ctrl Pts',(0.505181361323026,1.,1.99741107463572));
#26776=CARTESIAN_POINT('Ctrl Pts',(0.509046069886157,-1.,2.00225107134734));
#26777=CARTESIAN_POINT('Ctrl Pts',(0.509046069886157,1.,2.00225107134734));
#26778=CARTESIAN_POINT('Ctrl Pts',(0.512953306961792,-1.,2.00707309946949));
#26779=CARTESIAN_POINT('Ctrl Pts',(0.512953306961792,1.,2.00707309946949));
#26780=CARTESIAN_POINT('Ctrl Pts',(0.516902681728687,-1.,2.01187773939242));
#26781=CARTESIAN_POINT('Ctrl Pts',(0.516902681728687,1.,2.01187773939242));
#26782=CARTESIAN_POINT('Ctrl Pts',(0.52089359039937,-1.,2.01666477917286));
#26783=CARTESIAN_POINT('Ctrl Pts',(0.52089359039937,1.,2.01666477917286));
#26784=CARTESIAN_POINT('Ctrl Pts',(0.524925318333476,-1.,2.02143356304698));
#26785=CARTESIAN_POINT('Ctrl Pts',(0.524925318333476,1.,2.02143356304698));
#26786=CARTESIAN_POINT('Ctrl Pts',(0.528997127241914,-1.,2.0261832908329));
#26787=CARTESIAN_POINT('Ctrl Pts',(0.528997127241914,1.,2.0261832908329));
#26788=CARTESIAN_POINT('Ctrl Pts',(0.533108355132976,-1.,2.03091336214426));
#26789=CARTESIAN_POINT('Ctrl Pts',(0.533108355132976,1.,2.03091336214426));
#26790=CARTESIAN_POINT('Ctrl Pts',(0.537258489833262,-1.,2.03562362954037));
#26791=CARTESIAN_POINT('Ctrl Pts',(0.537258489833262,1.,2.03562362954037));
#26792=CARTESIAN_POINT('Ctrl Pts',(0.541447120615659,-1.,2.04031422690527));
#26793=CARTESIAN_POINT('Ctrl Pts',(0.541447120615659,1.,2.04031422690527));
#26794=CARTESIAN_POINT('Ctrl Pts',(0.54567390381743,-1.,2.04498544714588));
#26795=CARTESIAN_POINT('Ctrl Pts',(0.54567390381743,1.,2.04498544714588));
#26796=CARTESIAN_POINT('Ctrl Pts',(0.549938525150295,-1.,2.04963761077958));
#26797=CARTESIAN_POINT('Ctrl Pts',(0.549938525150295,1.,2.04963761077958));
#26798=CARTESIAN_POINT('Ctrl Pts',(0.554240657463906,-1.,2.05427091604413));
#26799=CARTESIAN_POINT('Ctrl Pts',(0.554240657463906,1.,2.05427091604413));
#26800=CARTESIAN_POINT('Ctrl Pts',(0.558579940185151,-1.,2.05888537756462));
#26801=CARTESIAN_POINT('Ctrl Pts',(0.558579940185151,1.,2.05888537756462));
#26802=CARTESIAN_POINT('Ctrl Pts',(0.562955993082261,-1.,2.06348090160589));
#26803=CARTESIAN_POINT('Ctrl Pts',(0.562955993082261,1.,2.06348090160589));
#26804=CARTESIAN_POINT('Ctrl Pts',(0.567368421181087,-1.,2.06805732997334));
#26805=CARTESIAN_POINT('Ctrl Pts',(0.567368421181087,1.,2.06805732997334));
#26806=CARTESIAN_POINT('Ctrl Pts',(0.571816823242602,-1.,2.07261449292824));
#26807=CARTESIAN_POINT('Ctrl Pts',(0.571816823242602,1.,2.07261449292824));
#26808=CARTESIAN_POINT('Ctrl Pts',(0.576300797416844,-1.,2.07715226767559));
#26809=CARTESIAN_POINT('Ctrl Pts',(0.576300797416844,1.,2.07715226767559));
#26810=CARTESIAN_POINT('Ctrl Pts',(0.580819952108063,-1.,2.08167059018418));
#26811=CARTESIAN_POINT('Ctrl Pts',(0.580819952108063,1.,2.08167059018418));
#26812=CARTESIAN_POINT('Ctrl Pts',(0.585373918991617,-1.,2.08616943727951));
#26813=CARTESIAN_POINT('Ctrl Pts',(0.585373918991617,1.,2.08616943727951));
#26814=CARTESIAN_POINT('Ctrl Pts',(0.589962365403406,-1.,2.09064881812129));
#26815=CARTESIAN_POINT('Ctrl Pts',(0.589962365403406,1.,2.09064881812129));
#26816=CARTESIAN_POINT('Ctrl Pts',(0.594585006052162,-1.,2.0951087622027));
#26817=CARTESIAN_POINT('Ctrl Pts',(0.594585006052162,1.,2.0951087622027));
#26818=CARTESIAN_POINT('Ctrl Pts',(0.599241616420533,-1.,2.0995493086477));
#26819=CARTESIAN_POINT('Ctrl Pts',(0.599241616420533,1.,2.0995493086477));
#26820=CARTESIAN_POINT('Ctrl Pts',(0.60393203073603,-1.,2.10397049886949));
#26821=CARTESIAN_POINT('Ctrl Pts',(0.60393203073603,1.,2.10397049886949));
#26822=CARTESIAN_POINT('Ctrl Pts',(0.607711315454876,-1.,2.1074919961518));
#26823=CARTESIAN_POINT('Ctrl Pts',(0.607711315454876,1.,2.1074919961518));
#26824=CARTESIAN_POINT('Ctrl Pts',(0.610560911689898,-1.,2.11012443807238));
#26825=CARTESIAN_POINT('Ctrl Pts',(0.610560911689898,1.,2.11012443807238));
#26826=CARTESIAN_POINT('Ctrl Pts',(0.6124673655618,-1.,2.11187554259986));
#26827=CARTESIAN_POINT('Ctrl Pts',(0.6124673655618,1.,2.11187554259986));
#26828=CARTESIAN_POINT('Ctrl Pts',(0.61342227326009,-1.,2.11275013067528));
#26829=CARTESIAN_POINT('Ctrl Pts',(0.61342227326009,1.,2.11275013067528));
#26830=CARTESIAN_POINT('',(0.383122945602004,1.,1.7075470150345));
#26831=CARTESIAN_POINT('Ctrl Pts',(0.383122945602004,1.,1.7075470150345));
#26832=CARTESIAN_POINT('Ctrl Pts',(0.384119047315541,1.,1.71231062891958));
#26833=CARTESIAN_POINT('Ctrl Pts',(0.38607079032701,1.,1.72162022246158));
#26834=CARTESIAN_POINT('Ctrl Pts',(0.388877023509191,1.,1.7349317097561));
#26835=CARTESIAN_POINT('Ctrl Pts',(0.392375812294307,1.,1.75137405313962));
#26836=CARTESIAN_POINT('Ctrl Pts',(0.39634619612042,1.,1.7697556004756));
#26837=CARTESIAN_POINT('Ctrl Pts',(0.39991940378308,1.,1.78598826347533));
#26838=CARTESIAN_POINT('Ctrl Pts',(0.403107976170441,1.,1.80012077176221));
#26839=CARTESIAN_POINT('Ctrl Pts',(0.405933518411838,1.,1.81223801813988));
#26840=CARTESIAN_POINT('Ctrl Pts',(0.408428948108533,1.,1.8224702267854));
#26841=CARTESIAN_POINT('Ctrl Pts',(0.410641256301674,1.,1.83100408895216));
#26842=CARTESIAN_POINT('Ctrl Pts',(0.412633125322161,1.,1.83808953475839));
#26843=CARTESIAN_POINT('Ctrl Pts',(0.41448743825434,1.,1.8440575707371));
#26844=CARTESIAN_POINT('Ctrl Pts',(0.416300022038864,1.,1.84929312929882));
#26845=CARTESIAN_POINT('Ctrl Pts',(0.418164129143534,1.,1.85417632856234));
#26846=CARTESIAN_POINT('Ctrl Pts',(0.420157287975619,1.,1.85903281096686));
#26847=CARTESIAN_POINT('Ctrl Pts',(0.422327307418275,1.,1.86408083334028));
#26848=CARTESIAN_POINT('Ctrl Pts',(0.424678177291358,1.,1.86937803944323));
#26849=CARTESIAN_POINT('Ctrl Pts',(0.427183828519102,1.,1.87486989291484));
#26850=CARTESIAN_POINT('Ctrl Pts',(0.429803062482344,1.,1.88044229001832));
#26851=CARTESIAN_POINT('Ctrl Pts',(0.432493038548748,1.,1.88596913666793));
#26852=CARTESIAN_POINT('Ctrl Pts',(0.435225660963383,1.,1.89136993975504));
#26853=CARTESIAN_POINT('Ctrl Pts',(0.437995003948244,1.,1.89663648956466));
#26854=CARTESIAN_POINT('Ctrl Pts',(0.440807833704038,1.,1.90180124389086));
#26855=CARTESIAN_POINT('Ctrl Pts',(0.44367755684915,1.,1.90691756144898));
#26856=CARTESIAN_POINT('Ctrl Pts',(0.446617343485711,1.,1.9120369998112));
#26857=CARTESIAN_POINT('Ctrl Pts',(0.449632260106662,1.,1.91718342555755));
#26858=CARTESIAN_POINT('Ctrl Pts',(0.452719478359432,1.,1.92235380648502));
#26859=CARTESIAN_POINT('Ctrl Pts',(0.45587200517437,1.,1.92753067150476));
#26860=CARTESIAN_POINT('Ctrl Pts',(0.459081234547926,1.,1.93269066517934));
#26861=CARTESIAN_POINT('Ctrl Pts',(0.462340031009056,1.,1.93781486640821));
#26862=CARTESIAN_POINT('Ctrl Pts',(0.46564546202603,1.,1.9428979419619));
#26863=CARTESIAN_POINT('Ctrl Pts',(0.468997482913135,1.,1.94794381136514));
#26864=CARTESIAN_POINT('Ctrl Pts',(0.472397672264072,1.,1.95296148278133));
#26865=CARTESIAN_POINT('Ctrl Pts',(0.475848034683176,1.,1.95796111148177));
#26866=CARTESIAN_POINT('Ctrl Pts',(0.479349583074855,1.,1.96294933055943));
#26867=CARTESIAN_POINT('Ctrl Pts',(0.48290166212069,1.,1.96792703422362));
#26868=CARTESIAN_POINT('Ctrl Pts',(0.486502692907658,1.,1.97289186263272));
#26869=CARTESIAN_POINT('Ctrl Pts',(0.490150627860952,1.,1.97783973019229));
#26870=CARTESIAN_POINT('Ctrl Pts',(0.493843476541494,1.,1.98276658761821));
#26871=CARTESIAN_POINT('Ctrl Pts',(0.497579909545574,1.,1.98767044752932));
#26872=CARTESIAN_POINT('Ctrl Pts',(0.501359287727146,1.,1.99255149126155));
#26873=CARTESIAN_POINT('Ctrl Pts',(0.505181361323026,1.,1.99741107463572));
#26874=CARTESIAN_POINT('Ctrl Pts',(0.509046069886157,1.,2.00225107134734));
#26875=CARTESIAN_POINT('Ctrl Pts',(0.512953306961792,1.,2.00707309946949));
#26876=CARTESIAN_POINT('Ctrl Pts',(0.516902681728687,1.,2.01187773939242));
#26877=CARTESIAN_POINT('Ctrl Pts',(0.52089359039937,1.,2.01666477917286));
#26878=CARTESIAN_POINT('Ctrl Pts',(0.524925318333476,1.,2.02143356304698));
#26879=CARTESIAN_POINT('Ctrl Pts',(0.528997127241914,1.,2.0261832908329));
#26880=CARTESIAN_POINT('Ctrl Pts',(0.533108355132976,1.,2.03091336214426));
#26881=CARTESIAN_POINT('Ctrl Pts',(0.537258489833262,1.,2.03562362954037));
#26882=CARTESIAN_POINT('Ctrl Pts',(0.541447120615659,1.,2.04031422690527));
#26883=CARTESIAN_POINT('Ctrl Pts',(0.54567390381743,1.,2.04498544714588));
#26884=CARTESIAN_POINT('Ctrl Pts',(0.549938525150295,1.,2.04963761077958));
#26885=CARTESIAN_POINT('Ctrl Pts',(0.554240657463906,1.,2.05427091604413));
#26886=CARTESIAN_POINT('Ctrl Pts',(0.558579940185151,1.,2.05888537756462));
#26887=CARTESIAN_POINT('Ctrl Pts',(0.562955993082261,1.,2.06348090160589));
#26888=CARTESIAN_POINT('Ctrl Pts',(0.567368421181087,1.,2.06805732997334));
#26889=CARTESIAN_POINT('Ctrl Pts',(0.571816823242602,1.,2.07261449292824));
#26890=CARTESIAN_POINT('Ctrl Pts',(0.576300797416844,1.,2.07715226767559));
#26891=CARTESIAN_POINT('Ctrl Pts',(0.580819952108063,1.,2.08167059018418));
#26892=CARTESIAN_POINT('Ctrl Pts',(0.585373918991617,1.,2.08616943727951));
#26893=CARTESIAN_POINT('Ctrl Pts',(0.589962365403406,1.,2.09064881812129));
#26894=CARTESIAN_POINT('Ctrl Pts',(0.594585006052162,1.,2.0951087622027));
#26895=CARTESIAN_POINT('Ctrl Pts',(0.599241616420533,1.,2.0995493086477));
#26896=CARTESIAN_POINT('Ctrl Pts',(0.60393203073603,1.,2.10397049886949));
#26897=CARTESIAN_POINT('Ctrl Pts',(0.607711315454876,1.,2.1074919961518));
#26898=CARTESIAN_POINT('Ctrl Pts',(0.610560911689898,1.,2.11012443807238));
#26899=CARTESIAN_POINT('Ctrl Pts',(0.6124673655618,1.,2.11187554259986));
#26900=CARTESIAN_POINT('Ctrl Pts',(0.61342227326009,1.,2.11275013067528));
#26901=CARTESIAN_POINT('',(0.383122945602003,0.,1.7075470150345));
#26902=CARTESIAN_POINT('Origin',(0.,0.,0.));
#26903=CARTESIAN_POINT('',(0.163289472382896,1.,1.74236521665491));
#26904=CARTESIAN_POINT('Origin',(0.,1.,0.));
#26905=CARTESIAN_POINT('',(0.163289472382896,0.,1.74236521665491));
#26906=CARTESIAN_POINT('Ctrl Pts',(0.0694764450219578,-1.,2.19890268624765));
#26907=CARTESIAN_POINT('Ctrl Pts',(0.0694764450219578,1.,2.19890268624765));
#26908=CARTESIAN_POINT('Ctrl Pts',(0.0701143536325487,-1.,2.19777582085423));
#26909=CARTESIAN_POINT('Ctrl Pts',(0.0701143536325487,1.,2.19777582085423));
#26910=CARTESIAN_POINT('Ctrl Pts',(0.0713863779526151,-1.,2.19552129484002));
#26911=CARTESIAN_POINT('Ctrl Pts',(0.0713863779526151,1.,2.19552129484002));
#26912=CARTESIAN_POINT('Ctrl Pts',(0.0732830357306722,-1.,2.19213712013662));
#26913=CARTESIAN_POINT('Ctrl Pts',(0.0732830357306722,1.,2.19213712013662));
#26914=CARTESIAN_POINT('Ctrl Pts',(0.0757891465836145,-1.,2.1876201139953));
#26915=CARTESIAN_POINT('Ctrl Pts',(0.0757891465836145,1.,2.1876201139953));
#26916=CARTESIAN_POINT('Ctrl Pts',(0.078883772768524,-1.,2.18196589448887));
#26917=CARTESIAN_POINT('Ctrl Pts',(0.078883772768524,1.,2.18196589448887));
#26918=CARTESIAN_POINT('Ctrl Pts',(0.0819402680872763,-1.,2.176303712113));
#26919=CARTESIAN_POINT('Ctrl Pts',(0.0819402680872763,1.,2.176303712113));
#26920=CARTESIAN_POINT('Ctrl Pts',(0.084958462083537,-1.,2.17063357870952));
#26921=CARTESIAN_POINT('Ctrl Pts',(0.084958462083537,1.,2.17063357870952));
#26922=CARTESIAN_POINT('Ctrl Pts',(0.087938129138692,-1.,2.16495552645014));
#26923=CARTESIAN_POINT('Ctrl Pts',(0.087938129138692,1.,2.16495552645014));
#26924=CARTESIAN_POINT('Ctrl Pts',(0.0908789888107263,-1.,2.15926961544516));
#26925=CARTESIAN_POINT('Ctrl Pts',(0.0908789888107263,1.,2.15926961544516));
#26926=CARTESIAN_POINT('Ctrl Pts',(0.0937807218867641,-1.,2.1535759397817));
#26927=CARTESIAN_POINT('Ctrl Pts',(0.0937807218867641,1.,2.1535759397817));
#26928=CARTESIAN_POINT('Ctrl Pts',(0.0966429852305456,-1.,2.14787463531795));
#26929=CARTESIAN_POINT('Ctrl Pts',(0.0966429852305456,1.,2.14787463531795));
#26930=CARTESIAN_POINT('Ctrl Pts',(0.0994654261990913,-1.,2.14216588396025));
#26931=CARTESIAN_POINT('Ctrl Pts',(0.0994654261990913,1.,2.14216588396025));
#26932=CARTESIAN_POINT('Ctrl Pts',(0.1022477005561,-1.,2.13644992667165));
#26933=CARTESIAN_POINT('Ctrl Pts',(0.1022477005561,1.,2.13644992667165));
#26934=CARTESIAN_POINT('Ctrl Pts',(0.104989479152739,-1.,2.13072704887293));
#26935=CARTESIAN_POINT('Ctrl Pts',(0.104989479152739,1.,2.13072704887293));
#26936=CARTESIAN_POINT('Ctrl Pts',(0.10769043523109,-1.,2.12499752307));
#26937=CARTESIAN_POINT('Ctrl Pts',(0.10769043523109,1.,2.12499752307));
#26938=CARTESIAN_POINT('Ctrl Pts',(0.110350236135025,-1.,2.11926155590865));
#26939=CARTESIAN_POINT('Ctrl Pts',(0.110350236135025,1.,2.11926155590865));
#26940=CARTESIAN_POINT('Ctrl Pts',(0.112968534419737,-1.,2.11351924490306));
#26941=CARTESIAN_POINT('Ctrl Pts',(0.112968534419737,1.,2.11351924490306));
#26942=CARTESIAN_POINT('Ctrl Pts',(0.115544957687926,-1.,2.10777050261309));
#26943=CARTESIAN_POINT('Ctrl Pts',(0.115544957687926,1.,2.10777050261309));
#26944=CARTESIAN_POINT('Ctrl Pts',(0.118079107988355,-1.,2.102015121329));
#26945=CARTESIAN_POINT('Ctrl Pts',(0.118079107988355,1.,2.102015121329));
#26946=CARTESIAN_POINT('Ctrl Pts',(0.120570567965122,-1.,2.0962529286773));
#26947=CARTESIAN_POINT('Ctrl Pts',(0.120570567965122,1.,2.0962529286773));
#26948=CARTESIAN_POINT('Ctrl Pts',(0.123018905621083,-1.,2.09048392424825));
#26949=CARTESIAN_POINT('Ctrl Pts',(0.123018905621083,1.,2.09048392424825));
#26950=CARTESIAN_POINT('Ctrl Pts',(0.125423679412061,-1.,2.08470840653643));
#26951=CARTESIAN_POINT('Ctrl Pts',(0.125423679412061,1.,2.08470840653643));
#26952=CARTESIAN_POINT('Ctrl Pts',(0.12778444527612,-1.,2.07892715110987));
#26953=CARTESIAN_POINT('Ctrl Pts',(0.12778444527612,1.,2.07892715110987));
#26954=CARTESIAN_POINT('Ctrl Pts',(0.130100748328403,-1.,2.07314114713063));
#26955=CARTESIAN_POINT('Ctrl Pts',(0.130100748328403,1.,2.07314114713063));
#26956=CARTESIAN_POINT('Ctrl Pts',(0.13237211154771,-1.,2.06735123910326));
#26957=CARTESIAN_POINT('Ctrl Pts',(0.13237211154771,1.,2.06735123910326));
#26958=CARTESIAN_POINT('Ctrl Pts',(0.134598026192106,-1.,2.06155781517842));
#26959=CARTESIAN_POINT('Ctrl Pts',(0.134598026192106,1.,2.06155781517842));
#26960=CARTESIAN_POINT('Ctrl Pts',(0.136777941218043,-1.,2.05576044414264));
#26961=CARTESIAN_POINT('Ctrl Pts',(0.136777941218043,1.,2.05576044414264));
#26962=CARTESIAN_POINT('Ctrl Pts',(0.138911255368966,-1.,2.04995762001328));
#26963=CARTESIAN_POINT('Ctrl Pts',(0.138911255368966,1.,2.04995762001328));
#26964=CARTESIAN_POINT('Ctrl Pts',(0.140997332152546,-1.,2.04414757947916));
#26965=CARTESIAN_POINT('Ctrl Pts',(0.140997332152546,1.,2.04414757947916));
#26966=CARTESIAN_POINT('Ctrl Pts',(0.143035515058208,-1.,2.03832911025912));
#26967=CARTESIAN_POINT('Ctrl Pts',(0.143035515058208,1.,2.03832911025912));
#26968=CARTESIAN_POINT('Ctrl Pts',(0.145025140186057,-1.,2.03250223739942));
#26969=CARTESIAN_POINT('Ctrl Pts',(0.145025140186057,1.,2.03250223739942));
#26970=CARTESIAN_POINT('Ctrl Pts',(0.146965557332583,-1.,2.02666926182017));
#26971=CARTESIAN_POINT('Ctrl Pts',(0.146965557332583,1.,2.02666926182017));
#26972=CARTESIAN_POINT('Ctrl Pts',(0.148856124775337,-1.,2.02083464969894));
#26973=CARTESIAN_POINT('Ctrl Pts',(0.148856124775337,1.,2.02083464969894));
#26974=CARTESIAN_POINT('Ctrl Pts',(0.150696157673078,-1.,2.01500291940238));
#26975=CARTESIAN_POINT('Ctrl Pts',(0.150696157673078,1.,2.01500291940238));
#26976=CARTESIAN_POINT('Ctrl Pts',(0.152484883621449,-1.,2.00917680318424));
#26977=CARTESIAN_POINT('Ctrl Pts',(0.152484883621449,1.,2.00917680318424));
#26978=CARTESIAN_POINT('Ctrl Pts',(0.154221403049722,-1.,2.00335565310543));
#26979=CARTESIAN_POINT('Ctrl Pts',(0.154221403049722,1.,2.00335565310543));
#26980=CARTESIAN_POINT('Ctrl Pts',(0.155904629548783,-1.,1.99753284771497));
#26981=CARTESIAN_POINT('Ctrl Pts',(0.155904629548783,1.,1.99753284771497));
#26982=CARTESIAN_POINT('Ctrl Pts',(0.157533331459227,-1.,1.99169810931908));
#26983=CARTESIAN_POINT('Ctrl Pts',(0.157533331459227,1.,1.99169810931908));
#26984=CARTESIAN_POINT('Ctrl Pts',(0.159106226437299,-1.,1.98584238283292));
#26985=CARTESIAN_POINT('Ctrl Pts',(0.159106226437299,1.,1.98584238283292));
#26986=CARTESIAN_POINT('Ctrl Pts',(0.160622060784611,-1.,1.97996195437559));
#26987=CARTESIAN_POINT('Ctrl Pts',(0.160622060784611,1.,1.97996195437559));
#26988=CARTESIAN_POINT('Ctrl Pts',(0.162079693556288,-1.,1.97406280235188));
#26989=CARTESIAN_POINT('Ctrl Pts',(0.162079693556288,1.,1.97406280235188));
#26990=CARTESIAN_POINT('Ctrl Pts',(0.163478185457734,-1.,1.96816512677967));
#26991=CARTESIAN_POINT('Ctrl Pts',(0.163478185457734,1.,1.96816512677967));
#26992=CARTESIAN_POINT('Ctrl Pts',(0.164816568920269,-1.,1.96229379940136));
#26993=CARTESIAN_POINT('Ctrl Pts',(0.164816568920269,1.,1.96229379940136));
#26994=CARTESIAN_POINT('Ctrl Pts',(0.166093592002812,-1.,1.9564675971873));
#26995=CARTESIAN_POINT('Ctrl Pts',(0.166093592002812,1.,1.9564675971873));
#26996=CARTESIAN_POINT('Ctrl Pts',(0.167307501784475,-1.,1.95069027794294));
#26997=CARTESIAN_POINT('Ctrl Pts',(0.167307501784475,1.,1.95069027794294));
#26998=CARTESIAN_POINT('Ctrl Pts',(0.168455741607556,-1.,1.94493757756931));
#26999=CARTESIAN_POINT('Ctrl Pts',(0.168455741607556,1.,1.94493757756931));
#27000=CARTESIAN_POINT('Ctrl Pts',(0.16953490481749,-1.,1.93915639211581));
#27001=CARTESIAN_POINT('Ctrl Pts',(0.16953490481749,1.,1.93915639211581));
#27002=CARTESIAN_POINT('Ctrl Pts',(0.170541253116201,-1.,1.93329183155539));
#27003=CARTESIAN_POINT('Ctrl Pts',(0.170541253116201,1.,1.93329183155539));
#27004=CARTESIAN_POINT('Ctrl Pts',(0.171471191532988,-1.,1.92731093582036));
#27005=CARTESIAN_POINT('Ctrl Pts',(0.171471191532988,1.,1.92731093582036));
#27006=CARTESIAN_POINT('Ctrl Pts',(0.172321621259513,-1.,1.9212233439798));
#27007=CARTESIAN_POINT('Ctrl Pts',(0.172321621259513,1.,1.9212233439798));
#27008=CARTESIAN_POINT('Ctrl Pts',(0.173090695383496,-1.,1.91511429159527));
#27009=CARTESIAN_POINT('Ctrl Pts',(0.173090695383496,1.,1.91511429159527));
#27010=CARTESIAN_POINT('Ctrl Pts',(0.173776635257816,-1.,1.90911693975267));
#27011=CARTESIAN_POINT('Ctrl Pts',(0.173776635257816,1.,1.90911693975267));
#27012=CARTESIAN_POINT('Ctrl Pts',(0.174375518661085,-1.,1.90335253862834));
#27013=CARTESIAN_POINT('Ctrl Pts',(0.174375518661085,1.,1.90335253862834));
#27014=CARTESIAN_POINT('Ctrl Pts',(0.174879405091263,-1.,1.89788101117132));
#27015=CARTESIAN_POINT('Ctrl Pts',(0.174879405091263,1.,1.89788101117132));
#27016=CARTESIAN_POINT('Ctrl Pts',(0.175274276190844,-1.,1.892646301985));
#27017=CARTESIAN_POINT('Ctrl Pts',(0.175274276190844,1.,1.892646301985));
#27018=CARTESIAN_POINT('Ctrl Pts',(0.175538155840648,-1.,1.88742606273259));
#27019=CARTESIAN_POINT('Ctrl Pts',(0.175538155840648,1.,1.88742606273259));
#27020=CARTESIAN_POINT('Ctrl Pts',(0.175644148889698,-1.,1.88188663145367));
#27021=CARTESIAN_POINT('Ctrl Pts',(0.175644148889698,1.,1.88188663145367));
#27022=CARTESIAN_POINT('Ctrl Pts',(0.175563480746485,-1.,1.87563767773588));
#27023=CARTESIAN_POINT('Ctrl Pts',(0.175563480746485,1.,1.87563767773588));
#27024=CARTESIAN_POINT('Ctrl Pts',(0.175268337590757,-1.,1.86828349694799));
#27025=CARTESIAN_POINT('Ctrl Pts',(0.175268337590757,1.,1.86828349694799));
#27026=CARTESIAN_POINT('Ctrl Pts',(0.17473525927603,-1.,1.85948367088837));
#27027=CARTESIAN_POINT('Ctrl Pts',(0.17473525927603,1.,1.85948367088837));
#27028=CARTESIAN_POINT('Ctrl Pts',(0.173946627587731,-1.,1.8489811319852));
#27029=CARTESIAN_POINT('Ctrl Pts',(0.173946627587731,1.,1.8489811319852));
#27030=CARTESIAN_POINT('Ctrl Pts',(0.1728894428919,-1.,1.83658380527692));
#27031=CARTESIAN_POINT('Ctrl Pts',(0.1728894428919,1.,1.83658380527692));
#27032=CARTESIAN_POINT('Ctrl Pts',(0.171554770204119,-1.,1.82215766811545));
#27033=CARTESIAN_POINT('Ctrl Pts',(0.171554770204119,1.,1.82215766811545));
#27034=CARTESIAN_POINT('Ctrl Pts',(0.169936923904608,-1.,1.80561530629706));
#27035=CARTESIAN_POINT('Ctrl Pts',(0.169936923904608,1.,1.80561530629706));
#27036=CARTESIAN_POINT('Ctrl Pts',(0.168032772805197,-1.,1.7869064998507));
#27037=CARTESIAN_POINT('Ctrl Pts',(0.168032772805197,1.,1.7869064998507));
#27038=CARTESIAN_POINT('Ctrl Pts',(0.1662793551464,-1.,1.77018771684844));
#27039=CARTESIAN_POINT('Ctrl Pts',(0.1662793551464,1.,1.77018771684844));
#27040=CARTESIAN_POINT('Ctrl Pts',(0.164834765707158,-1.,1.75666056638427));
#27041=CARTESIAN_POINT('Ctrl Pts',(0.164834765707158,1.,1.75666056638427));
#27042=CARTESIAN_POINT('Ctrl Pts',(0.163814161002002,-1.,1.7472034950333));
#27043=CARTESIAN_POINT('Ctrl Pts',(0.163814161002002,1.,1.7472034950333));
#27044=CARTESIAN_POINT('Ctrl Pts',(0.163289472382896,-1.,1.74236521665491));
#27045=CARTESIAN_POINT('Ctrl Pts',(0.163289472382896,1.,1.74236521665491));
#27046=CARTESIAN_POINT('',(0.0694764450219578,1.,2.19890268624765));
#27047=CARTESIAN_POINT('Ctrl Pts',(0.0694764450219578,1.,2.19890268624765));
#27048=CARTESIAN_POINT('Ctrl Pts',(0.0701143536325487,1.,2.19777582085423));
#27049=CARTESIAN_POINT('Ctrl Pts',(0.0713863779526151,1.,2.19552129484002));
#27050=CARTESIAN_POINT('Ctrl Pts',(0.0732830357306722,1.,2.19213712013662));
#27051=CARTESIAN_POINT('Ctrl Pts',(0.0757891465836145,1.,2.1876201139953));
#27052=CARTESIAN_POINT('Ctrl Pts',(0.078883772768524,1.,2.18196589448887));
#27053=CARTESIAN_POINT('Ctrl Pts',(0.0819402680872763,1.,2.176303712113));
#27054=CARTESIAN_POINT('Ctrl Pts',(0.084958462083537,1.,2.17063357870952));
#27055=CARTESIAN_POINT('Ctrl Pts',(0.087938129138692,1.,2.16495552645014));
#27056=CARTESIAN_POINT('Ctrl Pts',(0.0908789888107263,1.,2.15926961544516));
#27057=CARTESIAN_POINT('Ctrl Pts',(0.0937807218867641,1.,2.1535759397817));
#27058=CARTESIAN_POINT('Ctrl Pts',(0.0966429852305456,1.,2.14787463531795));
#27059=CARTESIAN_POINT('Ctrl Pts',(0.0994654261990913,1.,2.14216588396025));
#27060=CARTESIAN_POINT('Ctrl Pts',(0.1022477005561,1.,2.13644992667165));
#27061=CARTESIAN_POINT('Ctrl Pts',(0.104989479152739,1.,2.13072704887293));
#27062=CARTESIAN_POINT('Ctrl Pts',(0.10769043523109,1.,2.12499752307));
#27063=CARTESIAN_POINT('Ctrl Pts',(0.110350236135025,1.,2.11926155590865));
#27064=CARTESIAN_POINT('Ctrl Pts',(0.112968534419737,1.,2.11351924490306));
#27065=CARTESIAN_POINT('Ctrl Pts',(0.115544957687926,1.,2.10777050261309));
#27066=CARTESIAN_POINT('Ctrl Pts',(0.118079107988355,1.,2.102015121329));
#27067=CARTESIAN_POINT('Ctrl Pts',(0.120570567965122,1.,2.0962529286773));
#27068=CARTESIAN_POINT('Ctrl Pts',(0.123018905621083,1.,2.09048392424825));
#27069=CARTESIAN_POINT('Ctrl Pts',(0.125423679412061,1.,2.08470840653643));
#27070=CARTESIAN_POINT('Ctrl Pts',(0.12778444527612,1.,2.07892715110987));
#27071=CARTESIAN_POINT('Ctrl Pts',(0.130100748328403,1.,2.07314114713063));
#27072=CARTESIAN_POINT('Ctrl Pts',(0.13237211154771,1.,2.06735123910326));
#27073=CARTESIAN_POINT('Ctrl Pts',(0.134598026192106,1.,2.06155781517842));
#27074=CARTESIAN_POINT('Ctrl Pts',(0.136777941218043,1.,2.05576044414264));
#27075=CARTESIAN_POINT('Ctrl Pts',(0.138911255368966,1.,2.04995762001328));
#27076=CARTESIAN_POINT('Ctrl Pts',(0.140997332152546,1.,2.04414757947916));
#27077=CARTESIAN_POINT('Ctrl Pts',(0.143035515058208,1.,2.03832911025912));
#27078=CARTESIAN_POINT('Ctrl Pts',(0.145025140186057,1.,2.03250223739942));
#27079=CARTESIAN_POINT('Ctrl Pts',(0.146965557332583,1.,2.02666926182017));
#27080=CARTESIAN_POINT('Ctrl Pts',(0.148856124775337,1.,2.02083464969894));
#27081=CARTESIAN_POINT('Ctrl Pts',(0.150696157673078,1.,2.01500291940238));
#27082=CARTESIAN_POINT('Ctrl Pts',(0.152484883621449,1.,2.00917680318424));
#27083=CARTESIAN_POINT('Ctrl Pts',(0.154221403049722,1.,2.00335565310543));
#27084=CARTESIAN_POINT('Ctrl Pts',(0.155904629548783,1.,1.99753284771497));
#27085=CARTESIAN_POINT('Ctrl Pts',(0.157533331459227,1.,1.99169810931908));
#27086=CARTESIAN_POINT('Ctrl Pts',(0.159106226437299,1.,1.98584238283292));
#27087=CARTESIAN_POINT('Ctrl Pts',(0.160622060784611,1.,1.97996195437559));
#27088=CARTESIAN_POINT('Ctrl Pts',(0.162079693556288,1.,1.97406280235188));
#27089=CARTESIAN_POINT('Ctrl Pts',(0.163478185457734,1.,1.96816512677967));
#27090=CARTESIAN_POINT('Ctrl Pts',(0.164816568920269,1.,1.96229379940136));
#27091=CARTESIAN_POINT('Ctrl Pts',(0.166093592002812,1.,1.9564675971873));
#27092=CARTESIAN_POINT('Ctrl Pts',(0.167307501784475,1.,1.95069027794294));
#27093=CARTESIAN_POINT('Ctrl Pts',(0.168455741607556,1.,1.94493757756931));
#27094=CARTESIAN_POINT('Ctrl Pts',(0.16953490481749,1.,1.93915639211581));
#27095=CARTESIAN_POINT('Ctrl Pts',(0.170541253116201,1.,1.93329183155539));
#27096=CARTESIAN_POINT('Ctrl Pts',(0.171471191532988,1.,1.92731093582036));
#27097=CARTESIAN_POINT('Ctrl Pts',(0.172321621259513,1.,1.9212233439798));
#27098=CARTESIAN_POINT('Ctrl Pts',(0.173090695383496,1.,1.91511429159527));
#27099=CARTESIAN_POINT('Ctrl Pts',(0.173776635257816,1.,1.90911693975267));
#27100=CARTESIAN_POINT('Ctrl Pts',(0.174375518661085,1.,1.90335253862834));
#27101=CARTESIAN_POINT('Ctrl Pts',(0.174879405091263,1.,1.89788101117132));
#27102=CARTESIAN_POINT('Ctrl Pts',(0.175274276190844,1.,1.892646301985));
#27103=CARTESIAN_POINT('Ctrl Pts',(0.175538155840648,1.,1.88742606273259));
#27104=CARTESIAN_POINT('Ctrl Pts',(0.175644148889698,1.,1.88188663145367));
#27105=CARTESIAN_POINT('Ctrl Pts',(0.175563480746485,1.,1.87563767773588));
#27106=CARTESIAN_POINT('Ctrl Pts',(0.175268337590757,1.,1.86828349694799));
#27107=CARTESIAN_POINT('Ctrl Pts',(0.17473525927603,1.,1.85948367088837));
#27108=CARTESIAN_POINT('Ctrl Pts',(0.173946627587731,1.,1.8489811319852));
#27109=CARTESIAN_POINT('Ctrl Pts',(0.1728894428919,1.,1.83658380527692));
#27110=CARTESIAN_POINT('Ctrl Pts',(0.171554770204119,1.,1.82215766811545));
#27111=CARTESIAN_POINT('Ctrl Pts',(0.169936923904608,1.,1.80561530629706));
#27112=CARTESIAN_POINT('Ctrl Pts',(0.168032772805197,1.,1.7869064998507));
#27113=CARTESIAN_POINT('Ctrl Pts',(0.1662793551464,1.,1.77018771684844));
#27114=CARTESIAN_POINT('Ctrl Pts',(0.164834765707158,1.,1.75666056638427));
#27115=CARTESIAN_POINT('Ctrl Pts',(0.163814161002002,1.,1.7472034950333));
#27116=CARTESIAN_POINT('Ctrl Pts',(0.163289472382896,1.,1.74236521665491));
#27117=CARTESIAN_POINT('',(0.0694764450219578,0.,2.19890268624765));
#27118=CARTESIAN_POINT('Origin',(-0.0694764450219586,0.,2.19890268624765));
#27119=CARTESIAN_POINT('',(-0.0694764450219586,1.,2.19890268624765));
#27120=CARTESIAN_POINT('',(0.0694764450219578,1.,2.19890268624765));
#27121=CARTESIAN_POINT('',(-0.0694764450219586,0.,2.19890268624765));
#27122=CARTESIAN_POINT('Ctrl Pts',(-0.163289472382896,-1.,1.74236521665491));
#27123=CARTESIAN_POINT('Ctrl Pts',(-0.163289472382896,1.,1.74236521665491));
#27124=CARTESIAN_POINT('Ctrl Pts',(-0.163814161002474,-1.,1.74720349503904));
#27125=CARTESIAN_POINT('Ctrl Pts',(-0.163814161002474,1.,1.74720349503904));
#27126=CARTESIAN_POINT('Ctrl Pts',(-0.164834765708484,-1.,1.75666056640041));
#27127=CARTESIAN_POINT('Ctrl Pts',(-0.164834765708484,1.,1.75666056640041));
#27128=CARTESIAN_POINT('Ctrl Pts',(-0.166279355148738,-1.,1.77018771687692));
#27129=CARTESIAN_POINT('Ctrl Pts',(-0.166279355148738,1.,1.77018771687692));
#27130=CARTESIAN_POINT('Ctrl Pts',(-0.16803277280837,-1.,1.78690649988931));
#27131=CARTESIAN_POINT('Ctrl Pts',(-0.16803277280837,1.,1.78690649988931));
#27132=CARTESIAN_POINT('Ctrl Pts',(-0.169936923908078,-1.,1.80561530633924));
#27133=CARTESIAN_POINT('Ctrl Pts',(-0.169936923908078,1.,1.80561530633924));
#27134=CARTESIAN_POINT('Ctrl Pts',(-0.171554770207306,-1.,1.82215766815414));
#27135=CARTESIAN_POINT('Ctrl Pts',(-0.171554770207306,1.,1.82215766815414));
#27136=CARTESIAN_POINT('Ctrl Pts',(-0.17288944289442,-1.,1.83658380530747));
#27137=CARTESIAN_POINT('Ctrl Pts',(-0.17288944289442,1.,1.83658380530747));
#27138=CARTESIAN_POINT('Ctrl Pts',(-0.173946627589401,-1.,1.84898113200543));
#27139=CARTESIAN_POINT('Ctrl Pts',(-0.173946627589401,1.,1.84898113200543));
#27140=CARTESIAN_POINT('Ctrl Pts',(-0.174735259276856,-1.,1.85948367089838));
#27141=CARTESIAN_POINT('Ctrl Pts',(-0.174735259276856,1.,1.85948367089838));
#27142=CARTESIAN_POINT('Ctrl Pts',(-0.175268337590901,-1.,1.86828349694972));
#27143=CARTESIAN_POINT('Ctrl Pts',(-0.175268337590901,1.,1.86828349694972));
#27144=CARTESIAN_POINT('Ctrl Pts',(-0.175563480746206,-1.,1.87563767773249));
#27145=CARTESIAN_POINT('Ctrl Pts',(-0.175563480746206,1.,1.87563767773249));
#27146=CARTESIAN_POINT('Ctrl Pts',(-0.175644148889271,-1.,1.88188663144846));
#27147=CARTESIAN_POINT('Ctrl Pts',(-0.175644148889271,1.,1.88188663144846));
#27148=CARTESIAN_POINT('Ctrl Pts',(-0.175538155840286,-1.,1.88742606272818));
#27149=CARTESIAN_POINT('Ctrl Pts',(-0.175538155840286,1.,1.88742606272818));
#27150=CARTESIAN_POINT('Ctrl Pts',(-0.175274276190664,-1.,1.89264630198279));
#27151=CARTESIAN_POINT('Ctrl Pts',(-0.175274276190664,1.,1.89264630198279));
#27152=CARTESIAN_POINT('Ctrl Pts',(-0.174879405091277,-1.,1.89788101117148));
#27153=CARTESIAN_POINT('Ctrl Pts',(-0.174879405091277,1.,1.89788101117148));
#27154=CARTESIAN_POINT('Ctrl Pts',(-0.174375518661222,-1.,1.90335253863003));
#27155=CARTESIAN_POINT('Ctrl Pts',(-0.174375518661222,1.,1.90335253863003));
#27156=CARTESIAN_POINT('Ctrl Pts',(-0.173776635257984,-1.,1.90911693975475));
#27157=CARTESIAN_POINT('Ctrl Pts',(-0.173776635257984,1.,1.90911693975475));
#27158=CARTESIAN_POINT('Ctrl Pts',(-0.173090695383619,-1.,1.91511429159681));
#27159=CARTESIAN_POINT('Ctrl Pts',(-0.173090695383619,1.,1.91511429159681));
#27160=CARTESIAN_POINT('Ctrl Pts',(-0.172321621259557,-1.,1.92122334398034));
#27161=CARTESIAN_POINT('Ctrl Pts',(-0.172321621259557,1.,1.92122334398034));
#27162=CARTESIAN_POINT('Ctrl Pts',(-0.17147119153296,-1.,1.92731093582));
#27163=CARTESIAN_POINT('Ctrl Pts',(-0.17147119153296,1.,1.92731093582));
#27164=CARTESIAN_POINT('Ctrl Pts',(-0.170541253116136,-1.,1.93329183155455));
#27165=CARTESIAN_POINT('Ctrl Pts',(-0.170541253116136,1.,1.93329183155455));
#27166=CARTESIAN_POINT('Ctrl Pts',(-0.169534904817425,-1.,1.93915639211497));
#27167=CARTESIAN_POINT('Ctrl Pts',(-0.169534904817425,1.,1.93915639211497));
#27168=CARTESIAN_POINT('Ctrl Pts',(-0.168455741607516,-1.,1.94493757756879));
#27169=CARTESIAN_POINT('Ctrl Pts',(-0.168455741607516,1.,1.94493757756879));
#27170=CARTESIAN_POINT('Ctrl Pts',(-0.167307501784469,-1.,1.95069027794286));
#27171=CARTESIAN_POINT('Ctrl Pts',(-0.167307501784469,1.,1.95069027794286));
#27172=CARTESIAN_POINT('Ctrl Pts',(-0.166093592002833,-1.,1.95646759718755));
#27173=CARTESIAN_POINT('Ctrl Pts',(-0.166093592002833,1.,1.95646759718755));
#27174=CARTESIAN_POINT('Ctrl Pts',(-0.1648165689203,-1.,1.96229379940174));
#27175=CARTESIAN_POINT('Ctrl Pts',(-0.1648165689203,1.,1.96229379940174));
#27176=CARTESIAN_POINT('Ctrl Pts',(-0.16347818545776,-1.,1.96816512678));
#27177=CARTESIAN_POINT('Ctrl Pts',(-0.16347818545776,1.,1.96816512678));
#27178=CARTESIAN_POINT('Ctrl Pts',(-0.162079693556302,-1.,1.97406280235204));
#27179=CARTESIAN_POINT('Ctrl Pts',(-0.162079693556302,1.,1.97406280235204));
#27180=CARTESIAN_POINT('Ctrl Pts',(-0.16062206078461,-1.,1.97996195437557));
#27181=CARTESIAN_POINT('Ctrl Pts',(-0.16062206078461,1.,1.97996195437557));
#27182=CARTESIAN_POINT('Ctrl Pts',(-0.159106226437289,-1.,1.98584238283279));
#27183=CARTESIAN_POINT('Ctrl Pts',(-0.159106226437289,1.,1.98584238283279));
#27184=CARTESIAN_POINT('Ctrl Pts',(-0.157533331459215,-1.,1.99169810931893));
#27185=CARTESIAN_POINT('Ctrl Pts',(-0.157533331459215,1.,1.99169810931893));
#27186=CARTESIAN_POINT('Ctrl Pts',(-0.155904629548775,-1.,1.99753284771487));
#27187=CARTESIAN_POINT('Ctrl Pts',(-0.155904629548775,1.,1.99753284771487));
#27188=CARTESIAN_POINT('Ctrl Pts',(-0.154221403049719,-1.,2.00335565310539));
#27189=CARTESIAN_POINT('Ctrl Pts',(-0.154221403049719,1.,2.00335565310539));
#27190=CARTESIAN_POINT('Ctrl Pts',(-0.152484883621452,-1.,2.00917680318426));
#27191=CARTESIAN_POINT('Ctrl Pts',(-0.152484883621452,1.,2.00917680318426));
#27192=CARTESIAN_POINT('Ctrl Pts',(-0.150696157673084,-1.,2.01500291940243));
#27193=CARTESIAN_POINT('Ctrl Pts',(-0.150696157673084,1.,2.01500291940243));
#27194=CARTESIAN_POINT('Ctrl Pts',(-0.148856124775343,-1.,2.02083464969897));
#27195=CARTESIAN_POINT('Ctrl Pts',(-0.148856124775343,1.,2.02083464969897));
#27196=CARTESIAN_POINT('Ctrl Pts',(-0.146965557332586,-1.,2.02666926182017));
#27197=CARTESIAN_POINT('Ctrl Pts',(-0.146965557332586,1.,2.02666926182017));
#27198=CARTESIAN_POINT('Ctrl Pts',(-0.145025140186058,-1.,2.03250223739941));
#27199=CARTESIAN_POINT('Ctrl Pts',(-0.145025140186058,1.,2.03250223739941));
#27200=CARTESIAN_POINT('Ctrl Pts',(-0.143035515058208,-1.,2.03832911025913));
#27201=CARTESIAN_POINT('Ctrl Pts',(-0.143035515058208,1.,2.03832911025913));
#27202=CARTESIAN_POINT('Ctrl Pts',(-0.140997332152546,-1.,2.04414757947919));
#27203=CARTESIAN_POINT('Ctrl Pts',(-0.140997332152546,1.,2.04414757947919));
#27204=CARTESIAN_POINT('Ctrl Pts',(-0.138911255368966,-1.,2.04995762001333));
#27205=CARTESIAN_POINT('Ctrl Pts',(-0.138911255368966,1.,2.04995762001333));
#27206=CARTESIAN_POINT('Ctrl Pts',(-0.136777941218044,-1.,2.0557604441427));
#27207=CARTESIAN_POINT('Ctrl Pts',(-0.136777941218044,1.,2.0557604441427));
#27208=CARTESIAN_POINT('Ctrl Pts',(-0.134598026192107,-1.,2.06155781517844));
#27209=CARTESIAN_POINT('Ctrl Pts',(-0.134598026192107,1.,2.06155781517844));
#27210=CARTESIAN_POINT('Ctrl Pts',(-0.13237211154771,-1.,2.06735123910319));
#27211=CARTESIAN_POINT('Ctrl Pts',(-0.13237211154771,1.,2.06735123910319));
#27212=CARTESIAN_POINT('Ctrl Pts',(-0.130100748328401,-1.,2.07314114713047));
#27213=CARTESIAN_POINT('Ctrl Pts',(-0.130100748328401,1.,2.07314114713047));
#27214=CARTESIAN_POINT('Ctrl Pts',(-0.127784445276116,-1.,2.07892715110967));
#27215=CARTESIAN_POINT('Ctrl Pts',(-0.127784445276116,1.,2.07892715110967));
#27216=CARTESIAN_POINT('Ctrl Pts',(-0.125423679412058,-1.,2.08470840653628));
#27217=CARTESIAN_POINT('Ctrl Pts',(-0.125423679412058,1.,2.08470840653628));
#27218=CARTESIAN_POINT('Ctrl Pts',(-0.123018905621083,-1.,2.09048392424826));
#27219=CARTESIAN_POINT('Ctrl Pts',(-0.123018905621083,1.,2.09048392424826));
#27220=CARTESIAN_POINT('Ctrl Pts',(-0.120570567965129,-1.,2.09625292867756));
#27221=CARTESIAN_POINT('Ctrl Pts',(-0.120570567965129,1.,2.09625292867756));
#27222=CARTESIAN_POINT('Ctrl Pts',(-0.118079107988368,-1.,2.10201512132945));
#27223=CARTESIAN_POINT('Ctrl Pts',(-0.118079107988368,1.,2.10201512132945));
#27224=CARTESIAN_POINT('Ctrl Pts',(-0.115544957687941,-1.,2.10777050261359));
#27225=CARTESIAN_POINT('Ctrl Pts',(-0.115544957687941,1.,2.10777050261359));
#27226=CARTESIAN_POINT('Ctrl Pts',(-0.112968534419746,-1.,2.11351924490335));
#27227=CARTESIAN_POINT('Ctrl Pts',(-0.112968534419746,1.,2.11351924490335));
#27228=CARTESIAN_POINT('Ctrl Pts',(-0.11035023613502,-1.,2.11926155590849));
#27229=CARTESIAN_POINT('Ctrl Pts',(-0.11035023613502,1.,2.11926155590849));
#27230=CARTESIAN_POINT('Ctrl Pts',(-0.107690435231068,-1.,2.12499752306927));
#27231=CARTESIAN_POINT('Ctrl Pts',(-0.107690435231068,1.,2.12499752306927));
#27232=CARTESIAN_POINT('Ctrl Pts',(-0.104989479152703,-1.,2.1307270488718));
#27233=CARTESIAN_POINT('Ctrl Pts',(-0.104989479152703,1.,2.1307270488718));
#27234=CARTESIAN_POINT('Ctrl Pts',(-0.102247700556064,-1.,2.13644992667052));
#27235=CARTESIAN_POINT('Ctrl Pts',(-0.102247700556064,1.,2.13644992667052));
#27236=CARTESIAN_POINT('Ctrl Pts',(-0.0994654261990745,-1.,2.14216588395974));
#27237=CARTESIAN_POINT('Ctrl Pts',(-0.0994654261990745,1.,2.14216588395974));
#27238=CARTESIAN_POINT('Ctrl Pts',(-0.0966429852305691,-1.,2.14787463531864));
#27239=CARTESIAN_POINT('Ctrl Pts',(-0.0966429852305691,1.,2.14787463531864));
#27240=CARTESIAN_POINT('Ctrl Pts',(-0.0937807218868348,-1.,2.15357593978377));
#27241=CARTESIAN_POINT('Ctrl Pts',(-0.0937807218868348,1.,2.15357593978377));
#27242=CARTESIAN_POINT('Ctrl Pts',(-0.0908789888108269,-1.,2.15926961544808));
#27243=CARTESIAN_POINT('Ctrl Pts',(-0.0908789888108269,1.,2.15926961544808));
#27244=CARTESIAN_POINT('Ctrl Pts',(-0.0879381291387825,-1.,2.16495552645275));
#27245=CARTESIAN_POINT('Ctrl Pts',(-0.0879381291387825,1.,2.16495552645275));
#27246=CARTESIAN_POINT('Ctrl Pts',(-0.0849584620835646,-1.,2.17063357871031));
#27247=CARTESIAN_POINT('Ctrl Pts',(-0.0849584620835646,1.,2.17063357871031));
#27248=CARTESIAN_POINT('Ctrl Pts',(-0.0819402680871942,-1.,2.1763037121106));
#27249=CARTESIAN_POINT('Ctrl Pts',(-0.0819402680871942,1.,2.1763037121106));
#27250=CARTESIAN_POINT('Ctrl Pts',(-0.078883772768323,-1.,2.18196589448304));
#27251=CARTESIAN_POINT('Ctrl Pts',(-0.078883772768323,1.,2.18196589448304));
#27252=CARTESIAN_POINT('Ctrl Pts',(-0.0757891465833414,-1.,2.1876201139874));
#27253=CARTESIAN_POINT('Ctrl Pts',(-0.0757891465833414,1.,2.1876201139874));
#27254=CARTESIAN_POINT('Ctrl Pts',(-0.0732830357304279,-1.,2.19213712012956));
#27255=CARTESIAN_POINT('Ctrl Pts',(-0.0732830357304279,1.,2.19213712012956));
#27256=CARTESIAN_POINT('Ctrl Pts',(-0.071386377952463,-1.,2.19552129483562));
#27257=CARTESIAN_POINT('Ctrl Pts',(-0.071386377952463,1.,2.19552129483562));
#27258=CARTESIAN_POINT('Ctrl Pts',(-0.0701143536324929,-1.,2.19777582085261));
#27259=CARTESIAN_POINT('Ctrl Pts',(-0.0701143536324929,1.,2.19777582085261));
#27260=CARTESIAN_POINT('Ctrl Pts',(-0.0694764450219586,-1.,2.19890268624765));
#27261=CARTESIAN_POINT('Ctrl Pts',(-0.0694764450219586,1.,2.19890268624765));
#27262=CARTESIAN_POINT('',(-0.163289472382896,1.,1.74236521665491));
#27263=CARTESIAN_POINT('Ctrl Pts',(-0.163289472382896,1.,1.74236521665491));
#27264=CARTESIAN_POINT('Ctrl Pts',(-0.163814161002474,1.,1.74720349503904));
#27265=CARTESIAN_POINT('Ctrl Pts',(-0.164834765708484,1.,1.75666056640041));
#27266=CARTESIAN_POINT('Ctrl Pts',(-0.166279355148738,1.,1.77018771687692));
#27267=CARTESIAN_POINT('Ctrl Pts',(-0.16803277280837,1.,1.78690649988931));
#27268=CARTESIAN_POINT('Ctrl Pts',(-0.169936923908078,1.,1.80561530633924));
#27269=CARTESIAN_POINT('Ctrl Pts',(-0.171554770207306,1.,1.82215766815414));
#27270=CARTESIAN_POINT('Ctrl Pts',(-0.17288944289442,1.,1.83658380530747));
#27271=CARTESIAN_POINT('Ctrl Pts',(-0.173946627589401,1.,1.84898113200543));
#27272=CARTESIAN_POINT('Ctrl Pts',(-0.174735259276856,1.,1.85948367089838));
#27273=CARTESIAN_POINT('Ctrl Pts',(-0.175268337590901,1.,1.86828349694972));
#27274=CARTESIAN_POINT('Ctrl Pts',(-0.175563480746206,1.,1.87563767773249));
#27275=CARTESIAN_POINT('Ctrl Pts',(-0.175644148889271,1.,1.88188663144846));
#27276=CARTESIAN_POINT('Ctrl Pts',(-0.175538155840286,1.,1.88742606272818));
#27277=CARTESIAN_POINT('Ctrl Pts',(-0.175274276190664,1.,1.89264630198279));
#27278=CARTESIAN_POINT('Ctrl Pts',(-0.174879405091277,1.,1.89788101117148));
#27279=CARTESIAN_POINT('Ctrl Pts',(-0.174375518661222,1.,1.90335253863003));
#27280=CARTESIAN_POINT('Ctrl Pts',(-0.173776635257984,1.,1.90911693975475));
#27281=CARTESIAN_POINT('Ctrl Pts',(-0.173090695383619,1.,1.91511429159681));
#27282=CARTESIAN_POINT('Ctrl Pts',(-0.172321621259557,1.,1.92122334398034));
#27283=CARTESIAN_POINT('Ctrl Pts',(-0.17147119153296,1.,1.92731093582));
#27284=CARTESIAN_POINT('Ctrl Pts',(-0.170541253116136,1.,1.93329183155455));
#27285=CARTESIAN_POINT('Ctrl Pts',(-0.169534904817425,1.,1.93915639211497));
#27286=CARTESIAN_POINT('Ctrl Pts',(-0.168455741607516,1.,1.94493757756879));
#27287=CARTESIAN_POINT('Ctrl Pts',(-0.167307501784469,1.,1.95069027794286));
#27288=CARTESIAN_POINT('Ctrl Pts',(-0.166093592002833,1.,1.95646759718755));
#27289=CARTESIAN_POINT('Ctrl Pts',(-0.1648165689203,1.,1.96229379940174));
#27290=CARTESIAN_POINT('Ctrl Pts',(-0.16347818545776,1.,1.96816512678));
#27291=CARTESIAN_POINT('Ctrl Pts',(-0.162079693556302,1.,1.97406280235204));
#27292=CARTESIAN_POINT('Ctrl Pts',(-0.16062206078461,1.,1.97996195437557));
#27293=CARTESIAN_POINT('Ctrl Pts',(-0.159106226437289,1.,1.98584238283279));
#27294=CARTESIAN_POINT('Ctrl Pts',(-0.157533331459215,1.,1.99169810931893));
#27295=CARTESIAN_POINT('Ctrl Pts',(-0.155904629548775,1.,1.99753284771487));
#27296=CARTESIAN_POINT('Ctrl Pts',(-0.154221403049719,1.,2.00335565310539));
#27297=CARTESIAN_POINT('Ctrl Pts',(-0.152484883621452,1.,2.00917680318426));
#27298=CARTESIAN_POINT('Ctrl Pts',(-0.150696157673084,1.,2.01500291940243));
#27299=CARTESIAN_POINT('Ctrl Pts',(-0.148856124775343,1.,2.02083464969897));
#27300=CARTESIAN_POINT('Ctrl Pts',(-0.146965557332586,1.,2.02666926182017));
#27301=CARTESIAN_POINT('Ctrl Pts',(-0.145025140186058,1.,2.03250223739941));
#27302=CARTESIAN_POINT('Ctrl Pts',(-0.143035515058208,1.,2.03832911025913));
#27303=CARTESIAN_POINT('Ctrl Pts',(-0.140997332152546,1.,2.04414757947919));
#27304=CARTESIAN_POINT('Ctrl Pts',(-0.138911255368966,1.,2.04995762001333));
#27305=CARTESIAN_POINT('Ctrl Pts',(-0.136777941218044,1.,2.0557604441427));
#27306=CARTESIAN_POINT('Ctrl Pts',(-0.134598026192107,1.,2.06155781517844));
#27307=CARTESIAN_POINT('Ctrl Pts',(-0.13237211154771,1.,2.06735123910319));
#27308=CARTESIAN_POINT('Ctrl Pts',(-0.130100748328401,1.,2.07314114713047));
#27309=CARTESIAN_POINT('Ctrl Pts',(-0.127784445276116,1.,2.07892715110967));
#27310=CARTESIAN_POINT('Ctrl Pts',(-0.125423679412058,1.,2.08470840653628));
#27311=CARTESIAN_POINT('Ctrl Pts',(-0.123018905621083,1.,2.09048392424826));
#27312=CARTESIAN_POINT('Ctrl Pts',(-0.120570567965129,1.,2.09625292867756));
#27313=CARTESIAN_POINT('Ctrl Pts',(-0.118079107988368,1.,2.10201512132945));
#27314=CARTESIAN_POINT('Ctrl Pts',(-0.115544957687941,1.,2.10777050261359));
#27315=CARTESIAN_POINT('Ctrl Pts',(-0.112968534419746,1.,2.11351924490335));
#27316=CARTESIAN_POINT('Ctrl Pts',(-0.11035023613502,1.,2.11926155590849));
#27317=CARTESIAN_POINT('Ctrl Pts',(-0.107690435231068,1.,2.12499752306927));
#27318=CARTESIAN_POINT('Ctrl Pts',(-0.104989479152703,1.,2.1307270488718));
#27319=CARTESIAN_POINT('Ctrl Pts',(-0.102247700556064,1.,2.13644992667052));
#27320=CARTESIAN_POINT('Ctrl Pts',(-0.0994654261990745,1.,2.14216588395974));
#27321=CARTESIAN_POINT('Ctrl Pts',(-0.0966429852305691,1.,2.14787463531864));
#27322=CARTESIAN_POINT('Ctrl Pts',(-0.0937807218868348,1.,2.15357593978377));
#27323=CARTESIAN_POINT('Ctrl Pts',(-0.0908789888108269,1.,2.15926961544808));
#27324=CARTESIAN_POINT('Ctrl Pts',(-0.0879381291387825,1.,2.16495552645275));
#27325=CARTESIAN_POINT('Ctrl Pts',(-0.0849584620835646,1.,2.17063357871031));
#27326=CARTESIAN_POINT('Ctrl Pts',(-0.0819402680871942,1.,2.1763037121106));
#27327=CARTESIAN_POINT('Ctrl Pts',(-0.078883772768323,1.,2.18196589448304));
#27328=CARTESIAN_POINT('Ctrl Pts',(-0.0757891465833414,1.,2.1876201139874));
#27329=CARTESIAN_POINT('Ctrl Pts',(-0.0732830357304279,1.,2.19213712012956));
#27330=CARTESIAN_POINT('Ctrl Pts',(-0.071386377952463,1.,2.19552129483562));
#27331=CARTESIAN_POINT('Ctrl Pts',(-0.0701143536324929,1.,2.19777582085261));
#27332=CARTESIAN_POINT('Ctrl Pts',(-0.0694764450219586,1.,2.19890268624765));
#27333=CARTESIAN_POINT('',(-0.163289472382897,0.,1.74236521665491));
#27334=CARTESIAN_POINT('Origin',(0.,0.,0.));
#27335=CARTESIAN_POINT('',(-0.383122945602004,1.,1.7075470150345));
#27336=CARTESIAN_POINT('Origin',(0.,1.,0.));
#27337=CARTESIAN_POINT('',(-0.383122945602004,0.,1.7075470150345));
#27338=CARTESIAN_POINT('Ctrl Pts',(-0.61342227326009,-1.,2.11275013067528));
#27339=CARTESIAN_POINT('Ctrl Pts',(-0.61342227326009,1.,2.11275013067528));
#27340=CARTESIAN_POINT('Ctrl Pts',(-0.61246736556225,-1.,2.11187554260142));
#27341=CARTESIAN_POINT('Ctrl Pts',(-0.61246736556225,1.,2.11187554260142));
#27342=CARTESIAN_POINT('Ctrl Pts',(-0.610560911691113,-1.,2.11012443807661));
#27343=CARTESIAN_POINT('Ctrl Pts',(-0.610560911691113,1.,2.11012443807661));
#27344=CARTESIAN_POINT('Ctrl Pts',(-0.607711315456826,-1.,2.10749199615859));
#27345=CARTESIAN_POINT('Ctrl Pts',(-0.607711315456826,1.,2.10749199615859));
#27346=CARTESIAN_POINT('Ctrl Pts',(-0.603932030738212,-1.,2.10397049887709));
#27347=CARTESIAN_POINT('Ctrl Pts',(-0.603932030738212,1.,2.10397049887709));
#27348=CARTESIAN_POINT('Ctrl Pts',(-0.599241616422144,-1.,2.09954930865331));
#27349=CARTESIAN_POINT('Ctrl Pts',(-0.599241616422144,1.,2.09954930865331));
#27350=CARTESIAN_POINT('Ctrl Pts',(-0.594585006052824,-1.,2.09510876220501));
#27351=CARTESIAN_POINT('Ctrl Pts',(-0.594585006052824,1.,2.09510876220501));
#27352=CARTESIAN_POINT('Ctrl Pts',(-0.589962365403189,-1.,2.09064881812053));
#27353=CARTESIAN_POINT('Ctrl Pts',(-0.589962365403189,1.,2.09064881812053));
#27354=CARTESIAN_POINT('Ctrl Pts',(-0.585373918990895,-1.,2.086169437277));
#27355=CARTESIAN_POINT('Ctrl Pts',(-0.585373918990895,1.,2.086169437277));
#27356=CARTESIAN_POINT('Ctrl Pts',(-0.580819952107257,-1.,2.08167059018138));
#27357=CARTESIAN_POINT('Ctrl Pts',(-0.580819952107257,1.,2.08167059018138));
#27358=CARTESIAN_POINT('Ctrl Pts',(-0.576300797416275,-1.,2.07715226767361));
#27359=CARTESIAN_POINT('Ctrl Pts',(-0.576300797416275,1.,2.07715226767361));
#27360=CARTESIAN_POINT('Ctrl Pts',(-0.571816823242411,-1.,2.07261449292757));
#27361=CARTESIAN_POINT('Ctrl Pts',(-0.571816823242411,1.,2.07261449292757));
#27362=CARTESIAN_POINT('Ctrl Pts',(-0.567368421181229,-1.,2.06805732997383));
#27363=CARTESIAN_POINT('Ctrl Pts',(-0.567368421181229,1.,2.06805732997383));
#27364=CARTESIAN_POINT('Ctrl Pts',(-0.562955993082574,-1.,2.06348090160697));
#27365=CARTESIAN_POINT('Ctrl Pts',(-0.562955993082574,1.,2.06348090160697));
#27366=CARTESIAN_POINT('Ctrl Pts',(-0.558579940185467,-1.,2.05888537756571));
#27367=CARTESIAN_POINT('Ctrl Pts',(-0.558579940185467,1.,2.05888537756571));
#27368=CARTESIAN_POINT('Ctrl Pts',(-0.55424065746411,-1.,2.05427091604482));
#27369=CARTESIAN_POINT('Ctrl Pts',(-0.55424065746411,1.,2.05427091604482));
#27370=CARTESIAN_POINT('Ctrl Pts',(-0.549938525150342,-1.,2.04963761077974));
#27371=CARTESIAN_POINT('Ctrl Pts',(-0.549938525150342,1.,2.04963761077974));
#27372=CARTESIAN_POINT('Ctrl Pts',(-0.545673903817348,-1.,2.0449854471456));
#27373=CARTESIAN_POINT('Ctrl Pts',(-0.545673903817348,1.,2.0449854471456));
#27374=CARTESIAN_POINT('Ctrl Pts',(-0.54144712061552,-1.,2.0403142269048));
#27375=CARTESIAN_POINT('Ctrl Pts',(-0.54144712061552,1.,2.0403142269048));
#27376=CARTESIAN_POINT('Ctrl Pts',(-0.537258489833134,-1.,2.03562362953993));
#27377=CARTESIAN_POINT('Ctrl Pts',(-0.537258489833134,1.,2.03562362953993));
#27378=CARTESIAN_POINT('Ctrl Pts',(-0.533108355132905,-1.,2.03091336214401));
#27379=CARTESIAN_POINT('Ctrl Pts',(-0.533108355132905,1.,2.03091336214401));
#27380=CARTESIAN_POINT('Ctrl Pts',(-0.528997127241911,-1.,2.02618329083289));
#27381=CARTESIAN_POINT('Ctrl Pts',(-0.528997127241911,1.,2.02618329083289));
#27382=CARTESIAN_POINT('Ctrl Pts',(-0.524925318333518,-1.,2.02143356304712));
#27383=CARTESIAN_POINT('Ctrl Pts',(-0.524925318333518,1.,2.02143356304712));
#27384=CARTESIAN_POINT('Ctrl Pts',(-0.520893590399428,-1.,2.01666477917305));
#27385=CARTESIAN_POINT('Ctrl Pts',(-0.520893590399428,1.,2.01666477917305));
#27386=CARTESIAN_POINT('Ctrl Pts',(-0.516902681728733,-1.,2.01187773939257));
#27387=CARTESIAN_POINT('Ctrl Pts',(-0.516902681728733,1.,2.01187773939257));
#27388=CARTESIAN_POINT('Ctrl Pts',(-0.512953306961814,-1.,2.00707309946955));
#27389=CARTESIAN_POINT('Ctrl Pts',(-0.512953306961814,1.,2.00707309946955));
#27390=CARTESIAN_POINT('Ctrl Pts',(-0.509046069886152,-1.,2.00225107134733));
#27391=CARTESIAN_POINT('Ctrl Pts',(-0.509046069886152,1.,2.00225107134733));
#27392=CARTESIAN_POINT('Ctrl Pts',(-0.505181361323011,-1.,1.99741107463567));
#27393=CARTESIAN_POINT('Ctrl Pts',(-0.505181361323011,1.,1.99741107463567));
#27394=CARTESIAN_POINT('Ctrl Pts',(-0.501359287727129,-1.,1.9925514912615));
#27395=CARTESIAN_POINT('Ctrl Pts',(-0.501359287727129,1.,1.9925514912615));
#27396=CARTESIAN_POINT('Ctrl Pts',(-0.497579909545564,-1.,1.98767044752929));
#27397=CARTESIAN_POINT('Ctrl Pts',(-0.497579909545564,1.,1.98767044752929));
#27398=CARTESIAN_POINT('Ctrl Pts',(-0.493843476541492,-1.,1.9827665876182));
#27399=CARTESIAN_POINT('Ctrl Pts',(-0.493843476541492,1.,1.9827665876182));
#27400=CARTESIAN_POINT('Ctrl Pts',(-0.490150627860955,-1.,1.97783973019229));
#27401=CARTESIAN_POINT('Ctrl Pts',(-0.490150627860955,1.,1.97783973019229));
#27402=CARTESIAN_POINT('Ctrl Pts',(-0.486502692907661,-1.,1.97289186263272));
#27403=CARTESIAN_POINT('Ctrl Pts',(-0.486502692907661,1.,1.97289186263272));
#27404=CARTESIAN_POINT('Ctrl Pts',(-0.482901662120687,-1.,1.96792703422358));
#27405=CARTESIAN_POINT('Ctrl Pts',(-0.482901662120687,1.,1.96792703422358));
#27406=CARTESIAN_POINT('Ctrl Pts',(-0.479349583074846,-1.,1.96294933055938));
#27407=CARTESIAN_POINT('Ctrl Pts',(-0.479349583074846,1.,1.96294933055938));
#27408=CARTESIAN_POINT('Ctrl Pts',(-0.475848034683172,-1.,1.95796111148175));
#27409=CARTESIAN_POINT('Ctrl Pts',(-0.475848034683172,1.,1.95796111148175));
#27410=CARTESIAN_POINT('Ctrl Pts',(-0.47239767226408,-1.,1.95296148278136));
#27411=CARTESIAN_POINT('Ctrl Pts',(-0.47239767226408,1.,1.95296148278136));
#27412=CARTESIAN_POINT('Ctrl Pts',(-0.468997482913158,-1.,1.94794381136524));
#27413=CARTESIAN_POINT('Ctrl Pts',(-0.468997482913158,1.,1.94794381136524));
#27414=CARTESIAN_POINT('Ctrl Pts',(-0.465645462026065,-1.,1.94289794196205));
#27415=CARTESIAN_POINT('Ctrl Pts',(-0.465645462026065,1.,1.94289794196205));
#27416=CARTESIAN_POINT('Ctrl Pts',(-0.462340031009087,-1.,1.93781486640834));
#27417=CARTESIAN_POINT('Ctrl Pts',(-0.462340031009087,1.,1.93781486640834));
#27418=CARTESIAN_POINT('Ctrl Pts',(-0.459081234547931,-1.,1.93269066517936));
#27419=CARTESIAN_POINT('Ctrl Pts',(-0.459081234547931,1.,1.93269066517936));
#27420=CARTESIAN_POINT('Ctrl Pts',(-0.455872005174335,-1.,1.92753067150461));
#27421=CARTESIAN_POINT('Ctrl Pts',(-0.455872005174335,1.,1.92753067150461));
#27422=CARTESIAN_POINT('Ctrl Pts',(-0.452719478359356,-1.,1.9223538064847));
#27423=CARTESIAN_POINT('Ctrl Pts',(-0.452719478359356,1.,1.9223538064847));
#27424=CARTESIAN_POINT('Ctrl Pts',(-0.449632260106572,-1.,1.91718342555717));
#27425=CARTESIAN_POINT('Ctrl Pts',(-0.449632260106572,1.,1.91718342555717));
#27426=CARTESIAN_POINT('Ctrl Pts',(-0.446617343485651,-1.,1.91203699981095));
#27427=CARTESIAN_POINT('Ctrl Pts',(-0.446617343485651,1.,1.91203699981095));
#27428=CARTESIAN_POINT('Ctrl Pts',(-0.44367755684917,-1.,1.90691756144906));
#27429=CARTESIAN_POINT('Ctrl Pts',(-0.44367755684917,1.,1.90691756144906));
#27430=CARTESIAN_POINT('Ctrl Pts',(-0.440807833704161,-1.,1.90180124389137));
#27431=CARTESIAN_POINT('Ctrl Pts',(-0.440807833704161,1.,1.90180124389137));
#27432=CARTESIAN_POINT('Ctrl Pts',(-0.437995003948443,-1.,1.89663648956549));
#27433=CARTESIAN_POINT('Ctrl Pts',(-0.437995003948443,1.,1.89663648956549));
#27434=CARTESIAN_POINT('Ctrl Pts',(-0.43522566096358,-1.,1.89136993975585));
#27435=CARTESIAN_POINT('Ctrl Pts',(-0.43522566096358,1.,1.89136993975585));
#27436=CARTESIAN_POINT('Ctrl Pts',(-0.432493038548833,-1.,1.88596913666828));
#27437=CARTESIAN_POINT('Ctrl Pts',(-0.432493038548833,1.,1.88596913666828));
#27438=CARTESIAN_POINT('Ctrl Pts',(-0.429803062482217,-1.,1.88044229001778));
#27439=CARTESIAN_POINT('Ctrl Pts',(-0.429803062482217,1.,1.88044229001778));
#27440=CARTESIAN_POINT('Ctrl Pts',(-0.427183828518743,-1.,1.87486989291333));
#27441=CARTESIAN_POINT('Ctrl Pts',(-0.427183828518743,1.,1.87486989291333));
#27442=CARTESIAN_POINT('Ctrl Pts',(-0.424678177290876,-1.,1.8693780394412));
#27443=CARTESIAN_POINT('Ctrl Pts',(-0.424678177290876,1.,1.8693780394412));
#27444=CARTESIAN_POINT('Ctrl Pts',(-0.422327307417885,-1.,1.86408083333863));
#27445=CARTESIAN_POINT('Ctrl Pts',(-0.422327307417885,1.,1.86408083333863));
#27446=CARTESIAN_POINT('Ctrl Pts',(-0.420157287975583,-1.,1.8590328109667));
#27447=CARTESIAN_POINT('Ctrl Pts',(-0.420157287975583,1.,1.8590328109667));
#27448=CARTESIAN_POINT('Ctrl Pts',(-0.418164129144045,-1.,1.8541763285645));
#27449=CARTESIAN_POINT('Ctrl Pts',(-0.418164129144045,1.,1.8541763285645));
#27450=CARTESIAN_POINT('Ctrl Pts',(-0.416300022039885,-1.,1.84929312930314));
#27451=CARTESIAN_POINT('Ctrl Pts',(-0.416300022039885,1.,1.84929312930314));
#27452=CARTESIAN_POINT('Ctrl Pts',(-0.414487438255542,-1.,1.84405757074218));
#27453=CARTESIAN_POINT('Ctrl Pts',(-0.414487438255542,1.,1.84405757074218));
#27454=CARTESIAN_POINT('Ctrl Pts',(-0.412633125322945,-1.,1.8380895347617));
#27455=CARTESIAN_POINT('Ctrl Pts',(-0.412633125322945,1.,1.8380895347617));
#27456=CARTESIAN_POINT('Ctrl Pts',(-0.410641256301276,-1.,1.83100408895047));
#27457=CARTESIAN_POINT('Ctrl Pts',(-0.410641256301276,1.,1.83100408895047));
#27458=CARTESIAN_POINT('Ctrl Pts',(-0.408428948106227,-1.,1.82247022677562));
#27459=CARTESIAN_POINT('Ctrl Pts',(-0.408428948106227,1.,1.82247022677562));
#27460=CARTESIAN_POINT('Ctrl Pts',(-0.405933518407175,-1.,1.81223801812013));
#27461=CARTESIAN_POINT('Ctrl Pts',(-0.405933518407175,1.,1.81223801812013));
#27462=CARTESIAN_POINT('Ctrl Pts',(-0.403107976163396,-1.,1.80012077173238));
#27463=CARTESIAN_POINT('Ctrl Pts',(-0.403107976163396,1.,1.80012077173238));
#27464=CARTESIAN_POINT('Ctrl Pts',(-0.399919403774155,-1.,1.78598826343754));
#27465=CARTESIAN_POINT('Ctrl Pts',(-0.399919403774155,1.,1.78598826343754));
#27466=CARTESIAN_POINT('Ctrl Pts',(-0.396346196110688,-1.,1.76975560043442));
#27467=CARTESIAN_POINT('Ctrl Pts',(-0.396346196110688,1.,1.76975560043442));
#27468=CARTESIAN_POINT('Ctrl Pts',(-0.392375812285395,-1.,1.75137405310193));
#27469=CARTESIAN_POINT('Ctrl Pts',(-0.392375812285395,1.,1.75137405310193));
#27470=CARTESIAN_POINT('Ctrl Pts',(-0.388877023502615,-1.,1.73493170972829));
#27471=CARTESIAN_POINT('Ctrl Pts',(-0.388877023502615,1.,1.73493170972829));
#27472=CARTESIAN_POINT('Ctrl Pts',(-0.386070790323281,-1.,1.72162022244582));
#27473=CARTESIAN_POINT('Ctrl Pts',(-0.386070790323281,1.,1.72162022244582));
#27474=CARTESIAN_POINT('Ctrl Pts',(-0.384119047314215,-1.,1.71231062891398));
#27475=CARTESIAN_POINT('Ctrl Pts',(-0.384119047314215,1.,1.71231062891398));
#27476=CARTESIAN_POINT('Ctrl Pts',(-0.383122945602004,-1.,1.7075470150345));
#27477=CARTESIAN_POINT('Ctrl Pts',(-0.383122945602004,1.,1.7075470150345));
#27478=CARTESIAN_POINT('',(-0.61342227326009,1.,2.11275013067528));
#27479=CARTESIAN_POINT('Ctrl Pts',(-0.61342227326009,1.,2.11275013067528));
#27480=CARTESIAN_POINT('Ctrl Pts',(-0.61246736556225,1.,2.11187554260142));
#27481=CARTESIAN_POINT('Ctrl Pts',(-0.610560911691113,1.,2.11012443807661));
#27482=CARTESIAN_POINT('Ctrl Pts',(-0.607711315456826,1.,2.10749199615859));
#27483=CARTESIAN_POINT('Ctrl Pts',(-0.603932030738212,1.,2.10397049887709));
#27484=CARTESIAN_POINT('Ctrl Pts',(-0.599241616422144,1.,2.09954930865331));
#27485=CARTESIAN_POINT('Ctrl Pts',(-0.594585006052824,1.,2.09510876220501));
#27486=CARTESIAN_POINT('Ctrl Pts',(-0.589962365403189,1.,2.09064881812053));
#27487=CARTESIAN_POINT('Ctrl Pts',(-0.585373918990895,1.,2.086169437277));
#27488=CARTESIAN_POINT('Ctrl Pts',(-0.580819952107257,1.,2.08167059018138));
#27489=CARTESIAN_POINT('Ctrl Pts',(-0.576300797416275,1.,2.07715226767361));
#27490=CARTESIAN_POINT('Ctrl Pts',(-0.571816823242411,1.,2.07261449292757));
#27491=CARTESIAN_POINT('Ctrl Pts',(-0.567368421181229,1.,2.06805732997383));
#27492=CARTESIAN_POINT('Ctrl Pts',(-0.562955993082574,1.,2.06348090160697));
#27493=CARTESIAN_POINT('Ctrl Pts',(-0.558579940185467,1.,2.05888537756571));
#27494=CARTESIAN_POINT('Ctrl Pts',(-0.55424065746411,1.,2.05427091604482));
#27495=CARTESIAN_POINT('Ctrl Pts',(-0.549938525150342,1.,2.04963761077974));
#27496=CARTESIAN_POINT('Ctrl Pts',(-0.545673903817348,1.,2.0449854471456));
#27497=CARTESIAN_POINT('Ctrl Pts',(-0.54144712061552,1.,2.0403142269048));
#27498=CARTESIAN_POINT('Ctrl Pts',(-0.537258489833134,1.,2.03562362953993));
#27499=CARTESIAN_POINT('Ctrl Pts',(-0.533108355132905,1.,2.03091336214401));
#27500=CARTESIAN_POINT('Ctrl Pts',(-0.528997127241911,1.,2.02618329083289));
#27501=CARTESIAN_POINT('Ctrl Pts',(-0.524925318333518,1.,2.02143356304712));
#27502=CARTESIAN_POINT('Ctrl Pts',(-0.520893590399428,1.,2.01666477917305));
#27503=CARTESIAN_POINT('Ctrl Pts',(-0.516902681728733,1.,2.01187773939257));
#27504=CARTESIAN_POINT('Ctrl Pts',(-0.512953306961814,1.,2.00707309946955));
#27505=CARTESIAN_POINT('Ctrl Pts',(-0.509046069886152,1.,2.00225107134733));
#27506=CARTESIAN_POINT('Ctrl Pts',(-0.505181361323011,1.,1.99741107463567));
#27507=CARTESIAN_POINT('Ctrl Pts',(-0.501359287727129,1.,1.9925514912615));
#27508=CARTESIAN_POINT('Ctrl Pts',(-0.497579909545564,1.,1.98767044752929));
#27509=CARTESIAN_POINT('Ctrl Pts',(-0.493843476541492,1.,1.9827665876182));
#27510=CARTESIAN_POINT('Ctrl Pts',(-0.490150627860955,1.,1.97783973019229));
#27511=CARTESIAN_POINT('Ctrl Pts',(-0.486502692907661,1.,1.97289186263272));
#27512=CARTESIAN_POINT('Ctrl Pts',(-0.482901662120687,1.,1.96792703422358));
#27513=CARTESIAN_POINT('Ctrl Pts',(-0.479349583074846,1.,1.96294933055938));
#27514=CARTESIAN_POINT('Ctrl Pts',(-0.475848034683172,1.,1.95796111148175));
#27515=CARTESIAN_POINT('Ctrl Pts',(-0.47239767226408,1.,1.95296148278136));
#27516=CARTESIAN_POINT('Ctrl Pts',(-0.468997482913158,1.,1.94794381136524));
#27517=CARTESIAN_POINT('Ctrl Pts',(-0.465645462026065,1.,1.94289794196205));
#27518=CARTESIAN_POINT('Ctrl Pts',(-0.462340031009087,1.,1.93781486640834));
#27519=CARTESIAN_POINT('Ctrl Pts',(-0.459081234547931,1.,1.93269066517936));
#27520=CARTESIAN_POINT('Ctrl Pts',(-0.455872005174335,1.,1.92753067150461));
#27521=CARTESIAN_POINT('Ctrl Pts',(-0.452719478359356,1.,1.9223538064847));
#27522=CARTESIAN_POINT('Ctrl Pts',(-0.449632260106572,1.,1.91718342555717));
#27523=CARTESIAN_POINT('Ctrl Pts',(-0.446617343485651,1.,1.91203699981095));
#27524=CARTESIAN_POINT('Ctrl Pts',(-0.44367755684917,1.,1.90691756144906));
#27525=CARTESIAN_POINT('Ctrl Pts',(-0.440807833704161,1.,1.90180124389137));
#27526=CARTESIAN_POINT('Ctrl Pts',(-0.437995003948443,1.,1.89663648956549));
#27527=CARTESIAN_POINT('Ctrl Pts',(-0.43522566096358,1.,1.89136993975585));
#27528=CARTESIAN_POINT('Ctrl Pts',(-0.432493038548833,1.,1.88596913666828));
#27529=CARTESIAN_POINT('Ctrl Pts',(-0.429803062482217,1.,1.88044229001778));
#27530=CARTESIAN_POINT('Ctrl Pts',(-0.427183828518743,1.,1.87486989291333));
#27531=CARTESIAN_POINT('Ctrl Pts',(-0.424678177290876,1.,1.8693780394412));
#27532=CARTESIAN_POINT('Ctrl Pts',(-0.422327307417885,1.,1.86408083333863));
#27533=CARTESIAN_POINT('Ctrl Pts',(-0.420157287975583,1.,1.8590328109667));
#27534=CARTESIAN_POINT('Ctrl Pts',(-0.418164129144045,1.,1.8541763285645));
#27535=CARTESIAN_POINT('Ctrl Pts',(-0.416300022039885,1.,1.84929312930314));
#27536=CARTESIAN_POINT('Ctrl Pts',(-0.414487438255542,1.,1.84405757074218));
#27537=CARTESIAN_POINT('Ctrl Pts',(-0.412633125322945,1.,1.8380895347617));
#27538=CARTESIAN_POINT('Ctrl Pts',(-0.410641256301276,1.,1.83100408895047));
#27539=CARTESIAN_POINT('Ctrl Pts',(-0.408428948106227,1.,1.82247022677562));
#27540=CARTESIAN_POINT('Ctrl Pts',(-0.405933518407175,1.,1.81223801812013));
#27541=CARTESIAN_POINT('Ctrl Pts',(-0.403107976163396,1.,1.80012077173238));
#27542=CARTESIAN_POINT('Ctrl Pts',(-0.399919403774155,1.,1.78598826343754));
#27543=CARTESIAN_POINT('Ctrl Pts',(-0.396346196110688,1.,1.76975560043442));
#27544=CARTESIAN_POINT('Ctrl Pts',(-0.392375812285395,1.,1.75137405310193));
#27545=CARTESIAN_POINT('Ctrl Pts',(-0.388877023502615,1.,1.73493170972829));
#27546=CARTESIAN_POINT('Ctrl Pts',(-0.386070790323281,1.,1.72162022244582));
#27547=CARTESIAN_POINT('Ctrl Pts',(-0.384119047314215,1.,1.71231062891398));
#27548=CARTESIAN_POINT('Ctrl Pts',(-0.383122945602004,1.,1.7075470150345));
#27549=CARTESIAN_POINT('',(-0.61342227326009,0.,2.11275013067528));
#27550=CARTESIAN_POINT('Origin',(-0.745574324794401,0.,2.0698113262342));
#27551=CARTESIAN_POINT('',(-0.745574324794401,1.,2.0698113262342));
#27552=CARTESIAN_POINT('',(-0.61342227326009,1.,2.11275013067528));
#27553=CARTESIAN_POINT('',(-0.745574324794401,0.,2.0698113262342));
#27554=CARTESIAN_POINT('Ctrl Pts',(-0.693717979106306,-1.,1.60662857109684));
#27555=CARTESIAN_POINT('Ctrl Pts',(-0.693717979106306,1.,1.60662857109684));
#27556=CARTESIAN_POINT('Ctrl Pts',(-0.695712097881194,-1.,1.61106790958151));
#27557=CARTESIAN_POINT('Ctrl Pts',(-0.695712097881194,1.,1.61106790958151));
#27558=CARTESIAN_POINT('Ctrl Pts',(-0.699605146405088,-1.,1.61974673472612));
#27559=CARTESIAN_POINT('Ctrl Pts',(-0.699605146405088,1.,1.61974673472612));
#27560=CARTESIAN_POINT('Ctrl Pts',(-0.705159151988319,-1.,1.63216541664676));
#27561=CARTESIAN_POINT('Ctrl Pts',(-0.705159151988319,1.,1.63216541664676));
#27562=CARTESIAN_POINT('Ctrl Pts',(-0.711993139355394,-1.,1.64752408832016));
#27563=CARTESIAN_POINT('Ctrl Pts',(-0.711993139355394,1.,1.64752408832016));
#27564=CARTESIAN_POINT('Ctrl Pts',(-0.719585433804282,-1.,1.6647288055568));
#27565=CARTESIAN_POINT('Ctrl Pts',(-0.719585433804282,1.,1.6647288055568));
#27566=CARTESIAN_POINT('Ctrl Pts',(-0.726235967997433,-1.,1.67996158455503));
#27567=CARTESIAN_POINT('Ctrl Pts',(-0.726235967997433,1.,1.67996158455503));
#27568=CARTESIAN_POINT('Ctrl Pts',(-0.731963238697195,-1.,1.69326921975743));
#27569=CARTESIAN_POINT('Ctrl Pts',(-0.731963238697195,1.,1.69326921975743));
#27570=CARTESIAN_POINT('Ctrl Pts',(-0.736799665724771,-1.,1.70473309006121));
#27571=CARTESIAN_POINT('Ctrl Pts',(-0.736799665724771,1.,1.70473309006121));
#27572=CARTESIAN_POINT('Ctrl Pts',(-0.740795162032088,-1.,1.71447789751927));
#27573=CARTESIAN_POINT('Ctrl Pts',(-0.740795162032088,1.,1.71447789751927));
#27574=CARTESIAN_POINT('Ctrl Pts',(-0.744021445433764,-1.,1.7226822991693));
#27575=CARTESIAN_POINT('Ctrl Pts',(-0.744021445433764,1.,1.7226822991693));
#27576=CARTESIAN_POINT('Ctrl Pts',(-0.746574710096436,-1.,1.72958533647399));
#27577=CARTESIAN_POINT('Ctrl Pts',(-0.746574710096436,1.,1.72958533647399));
#27578=CARTESIAN_POINT('Ctrl Pts',(-0.748582462954855,-1.,1.73550351679848));
#27579=CARTESIAN_POINT('Ctrl Pts',(-0.748582462954855,1.,1.73550351679848));
#27580=CARTESIAN_POINT('Ctrl Pts',(-0.75019343597954,-1.,1.74080458266705));
#27581=CARTESIAN_POINT('Ctrl Pts',(-0.75019343597954,1.,1.74080458266705));
#27582=CARTESIAN_POINT('Ctrl Pts',(-0.751555614163629,-1.,1.74585086852298));
#27583=CARTESIAN_POINT('Ctrl Pts',(-0.751555614163629,1.,1.74585086852298));
#27584=CARTESIAN_POINT('Ctrl Pts',(-0.752797683531377,-1.,1.75095139468809));
#27585=CARTESIAN_POINT('Ctrl Pts',(-0.752797683531377,1.,1.75095139468809));
#27586=CARTESIAN_POINT('Ctrl Pts',(-0.75400925402848,-1.,1.75631083600175));
#27587=CARTESIAN_POINT('Ctrl Pts',(-0.75400925402848,1.,1.75631083600175));
#27588=CARTESIAN_POINT('Ctrl Pts',(-0.755220979975262,-1.,1.7619781724032));
#27589=CARTESIAN_POINT('Ctrl Pts',(-0.755220979975262,1.,1.7619781724032));
#27590=CARTESIAN_POINT('Ctrl Pts',(-0.756421896028403,-1.,1.76789396003141));
#27591=CARTESIAN_POINT('Ctrl Pts',(-0.756421896028403,1.,1.76789396003141));
#27592=CARTESIAN_POINT('Ctrl Pts',(-0.757578264077238,-1.,1.77394167108342));
#27593=CARTESIAN_POINT('Ctrl Pts',(-0.757578264077238,1.,1.77394167108342));
#27594=CARTESIAN_POINT('Ctrl Pts',(-0.75865062667738,-1.,1.77999411220912));
#27595=CARTESIAN_POINT('Ctrl Pts',(-0.75865062667738,1.,1.77999411220912));
#27596=CARTESIAN_POINT('Ctrl Pts',(-0.759614401109868,-1.,1.78596964884526));
#27597=CARTESIAN_POINT('Ctrl Pts',(-0.759614401109868,1.,1.78596964884526));
#27598=CARTESIAN_POINT('Ctrl Pts',(-0.760469555880425,-1.,1.79185815610802));
#27599=CARTESIAN_POINT('Ctrl Pts',(-0.760469555880425,1.,1.79185815610802));
#27600=CARTESIAN_POINT('Ctrl Pts',(-0.761229695230359,-1.,1.79768986997735));
#27601=CARTESIAN_POINT('Ctrl Pts',(-0.761229695230359,1.,1.79768986997735));
#27602=CARTESIAN_POINT('Ctrl Pts',(-0.761915336443516,-1.,1.80351583877334));
#27603=CARTESIAN_POINT('Ctrl Pts',(-0.761915336443516,1.,1.80351583877334));
#27604=CARTESIAN_POINT('Ctrl Pts',(-0.762546129464036,-1.,1.80938551463989));
#27605=CARTESIAN_POINT('Ctrl Pts',(-0.762546129464036,1.,1.80938551463989));
#27606=CARTESIAN_POINT('Ctrl Pts',(-0.763132003836783,-1.,1.81532118405566));
#27607=CARTESIAN_POINT('Ctrl Pts',(-0.763132003836783,1.,1.81532118405566));
#27608=CARTESIAN_POINT('Ctrl Pts',(-0.763673465462854,-1.,1.82131873145297));
#27609=CARTESIAN_POINT('Ctrl Pts',(-0.763673465462854,1.,1.82131873145297));
#27610=CARTESIAN_POINT('Ctrl Pts',(-0.764165902606055,-1.,1.8273599120008));
#27611=CARTESIAN_POINT('Ctrl Pts',(-0.764165902606055,1.,1.8273599120008));
#27612=CARTESIAN_POINT('Ctrl Pts',(-0.764602549687845,-1.,1.8334207722714));
#27613=CARTESIAN_POINT('Ctrl Pts',(-0.764602549687845,1.,1.8334207722714));
#27614=CARTESIAN_POINT('Ctrl Pts',(-0.764978057881687,-1.,1.83948181064823));
#27615=CARTESIAN_POINT('Ctrl Pts',(-0.764978057881687,1.,1.83948181064823));
#27616=CARTESIAN_POINT('Ctrl Pts',(-0.765291664861971,-1.,1.8455369887591));
#27617=CARTESIAN_POINT('Ctrl Pts',(-0.765291664861971,1.,1.8455369887591));
#27618=CARTESIAN_POINT('Ctrl Pts',(-0.765545710619023,-1.,1.85158945130054));
#27619=CARTESIAN_POINT('Ctrl Pts',(-0.765545710619023,1.,1.85158945130054));
#27620=CARTESIAN_POINT('Ctrl Pts',(-0.765744212909305,-1.,1.85764741390391));
#27621=CARTESIAN_POINT('Ctrl Pts',(-0.765744212909305,1.,1.85764741390391));
#27622=CARTESIAN_POINT('Ctrl Pts',(-0.765891519092557,-1.,1.86372027063314));
#27623=CARTESIAN_POINT('Ctrl Pts',(-0.765891519092557,1.,1.86372027063314));
#27624=CARTESIAN_POINT('Ctrl Pts',(-0.765990708546111,-1.,1.86981398314345));
#27625=CARTESIAN_POINT('Ctrl Pts',(-0.765990708546111,1.,1.86981398314345));
#27626=CARTESIAN_POINT('Ctrl Pts',(-0.766042837036759,-1.,1.87592888967886));
#27627=CARTESIAN_POINT('Ctrl Pts',(-0.766042837036759,1.,1.87592888967886));
#27628=CARTESIAN_POINT('Ctrl Pts',(-0.766047794851869,-1.,1.88206215302561));
#27629=CARTESIAN_POINT('Ctrl Pts',(-0.766047794851869,1.,1.88206215302561));
#27630=CARTESIAN_POINT('Ctrl Pts',(-0.76600483706209,-1.,1.88820926433409));
#27631=CARTESIAN_POINT('Ctrl Pts',(-0.76600483706209,1.,1.88820926433409));
#27632=CARTESIAN_POINT('Ctrl Pts',(-0.765913193856979,-1.,1.89436577771389));
#27633=CARTESIAN_POINT('Ctrl Pts',(-0.765913193856979,1.,1.89436577771389));
#27634=CARTESIAN_POINT('Ctrl Pts',(-0.765772772593395,-1.,1.90052930393599));
#27635=CARTESIAN_POINT('Ctrl Pts',(-0.765772772593395,1.,1.90052930393599));
#27636=CARTESIAN_POINT('Ctrl Pts',(-0.765584196937936,-1.,1.90669961402362));
#27637=CARTESIAN_POINT('Ctrl Pts',(-0.765584196937936,1.,1.90669961402362));
#27638=CARTESIAN_POINT('Ctrl Pts',(-0.765348465884739,-1.,1.91287765805174));
#27639=CARTESIAN_POINT('Ctrl Pts',(-0.765348465884739,1.,1.91287765805174));
#27640=CARTESIAN_POINT('Ctrl Pts',(-0.765066729667095,-1.,1.91906491634197));
#27641=CARTESIAN_POINT('Ctrl Pts',(-0.765066729667095,1.,1.91906491634197));
#27642=CARTESIAN_POINT('Ctrl Pts',(-0.764740025488189,-1.,1.92526263537041));
#27643=CARTESIAN_POINT('Ctrl Pts',(-0.764740025488189,1.,1.92526263537041));
#27644=CARTESIAN_POINT('Ctrl Pts',(-0.764369010673889,-1.,1.93147105496367));
#27645=CARTESIAN_POINT('Ctrl Pts',(-0.764369010673889,1.,1.93147105496367));
#27646=CARTESIAN_POINT('Ctrl Pts',(-0.763954049121393,-1.,1.93768964875867));
#27647=CARTESIAN_POINT('Ctrl Pts',(-0.763954049121393,1.,1.93768964875867));
#27648=CARTESIAN_POINT('Ctrl Pts',(-0.76349533353858,-1.,1.94391746617626));
#27649=CARTESIAN_POINT('Ctrl Pts',(-0.76349533353858,1.,1.94391746617626));
#27650=CARTESIAN_POINT('Ctrl Pts',(-0.762992990878774,-1.,1.95015342590025));
#27651=CARTESIAN_POINT('Ctrl Pts',(-0.762992990878774,1.,1.95015342590025));
#27652=CARTESIAN_POINT('Ctrl Pts',(-0.762447203806263,-1.,1.95639665309893));
#27653=CARTESIAN_POINT('Ctrl Pts',(-0.762447203806263,1.,1.95639665309893));
#27654=CARTESIAN_POINT('Ctrl Pts',(-0.761858300014575,-1.,1.96264672744229));
#27655=CARTESIAN_POINT('Ctrl Pts',(-0.761858300014575,1.,1.96264672744229));
#27656=CARTESIAN_POINT('Ctrl Pts',(-0.761226690483986,-1.,1.96890351582545));
#27657=CARTESIAN_POINT('Ctrl Pts',(-0.761226690483986,1.,1.96890351582545));
#27658=CARTESIAN_POINT('Ctrl Pts',(-0.760552825409855,-1.,1.97516705321521));
#27659=CARTESIAN_POINT('Ctrl Pts',(-0.760552825409855,1.,1.97516705321521));
#27660=CARTESIAN_POINT('Ctrl Pts',(-0.759837147452135,-1.,1.98143741418156));
#27661=CARTESIAN_POINT('Ctrl Pts',(-0.759837147452135,1.,1.98143741418156));
#27662=CARTESIAN_POINT('Ctrl Pts',(-0.759080037802243,-1.,1.98771456680806));
#27663=CARTESIAN_POINT('Ctrl Pts',(-0.759080037802243,1.,1.98771456680806));
#27664=CARTESIAN_POINT('Ctrl Pts',(-0.758281796766377,-1.,1.9939983109871));
#27665=CARTESIAN_POINT('Ctrl Pts',(-0.758281796766377,1.,1.9939983109871));
#27666=CARTESIAN_POINT('Ctrl Pts',(-0.757442676862341,-1.,2.00028834739072));
#27667=CARTESIAN_POINT('Ctrl Pts',(-0.757442676862341,1.,2.00028834739072));
#27668=CARTESIAN_POINT('Ctrl Pts',(-0.756562904646496,-1.,2.00658431587682));
#27669=CARTESIAN_POINT('Ctrl Pts',(-0.756562904646496,1.,2.00658431587682));
#27670=CARTESIAN_POINT('Ctrl Pts',(-0.7556427049581,-1.,2.01288584328149));
#27671=CARTESIAN_POINT('Ctrl Pts',(-0.7556427049581,1.,2.01288584328149));
#27672=CARTESIAN_POINT('Ctrl Pts',(-0.75468233072352,-1.,2.01919259406003));
#27673=CARTESIAN_POINT('Ctrl Pts',(-0.75468233072352,1.,2.01919259406003));
#27674=CARTESIAN_POINT('Ctrl Pts',(-0.753682061113766,-1.,2.02550428623587));
#27675=CARTESIAN_POINT('Ctrl Pts',(-0.753682061113766,1.,2.02550428623587));
#27676=CARTESIAN_POINT('Ctrl Pts',(-0.752642180488104,-1.,2.03182068456467));
#27677=CARTESIAN_POINT('Ctrl Pts',(-0.752642180488104,1.,2.03182068456467));
#27678=CARTESIAN_POINT('Ctrl Pts',(-0.751562963361384,-1.,2.03814160092173));
#27679=CARTESIAN_POINT('Ctrl Pts',(-0.751562963361384,1.,2.03814160092173));
#27680=CARTESIAN_POINT('Ctrl Pts',(-0.750444657874758,-1.,2.04446689147754));
#27681=CARTESIAN_POINT('Ctrl Pts',(-0.750444657874758,1.,2.04446689147754));
#27682=CARTESIAN_POINT('Ctrl Pts',(-0.749287468663053,-1.,2.05079645591606));
#27683=CARTESIAN_POINT('Ctrl Pts',(-0.749287468663053,1.,2.05079645591606));
#27684=CARTESIAN_POINT('Ctrl Pts',(-0.748091554181101,-1.,2.05713023030263));
#27685=CARTESIAN_POINT('Ctrl Pts',(-0.748091554181101,1.,2.05713023030263));
#27686=CARTESIAN_POINT('Ctrl Pts',(-0.747103932785504,-1.,2.06220058927162));
#27687=CARTESIAN_POINT('Ctrl Pts',(-0.747103932785504,1.,2.06220058927162));
#27688=CARTESIAN_POINT('Ctrl Pts',(-0.746345871542696,-1.,2.06600523016401));
#27689=CARTESIAN_POINT('Ctrl Pts',(-0.746345871542696,1.,2.06600523016401));
#27690=CARTESIAN_POINT('Ctrl Pts',(-0.74583279137781,-1.,2.06854248895575));
#27691=CARTESIAN_POINT('Ctrl Pts',(-0.74583279137781,1.,2.06854248895575));
#27692=CARTESIAN_POINT('Ctrl Pts',(-0.745574324794401,-1.,2.0698113262342));
#27693=CARTESIAN_POINT('Ctrl Pts',(-0.745574324794401,1.,2.0698113262342));
#27694=CARTESIAN_POINT('',(-0.693717979106306,1.,1.60662857109684));
#27695=CARTESIAN_POINT('Ctrl Pts',(-0.693717979106306,1.,1.60662857109684));
#27696=CARTESIAN_POINT('Ctrl Pts',(-0.695712097881194,1.,1.61106790958151));
#27697=CARTESIAN_POINT('Ctrl Pts',(-0.699605146405088,1.,1.61974673472612));
#27698=CARTESIAN_POINT('Ctrl Pts',(-0.705159151988319,1.,1.63216541664676));
#27699=CARTESIAN_POINT('Ctrl Pts',(-0.711993139355394,1.,1.64752408832016));
#27700=CARTESIAN_POINT('Ctrl Pts',(-0.719585433804282,1.,1.6647288055568));
#27701=CARTESIAN_POINT('Ctrl Pts',(-0.726235967997433,1.,1.67996158455503));
#27702=CARTESIAN_POINT('Ctrl Pts',(-0.731963238697195,1.,1.69326921975743));
#27703=CARTESIAN_POINT('Ctrl Pts',(-0.736799665724771,1.,1.70473309006121));
#27704=CARTESIAN_POINT('Ctrl Pts',(-0.740795162032088,1.,1.71447789751927));
#27705=CARTESIAN_POINT('Ctrl Pts',(-0.744021445433764,1.,1.7226822991693));
#27706=CARTESIAN_POINT('Ctrl Pts',(-0.746574710096436,1.,1.72958533647399));
#27707=CARTESIAN_POINT('Ctrl Pts',(-0.748582462954855,1.,1.73550351679848));
#27708=CARTESIAN_POINT('Ctrl Pts',(-0.75019343597954,1.,1.74080458266705));
#27709=CARTESIAN_POINT('Ctrl Pts',(-0.751555614163629,1.,1.74585086852298));
#27710=CARTESIAN_POINT('Ctrl Pts',(-0.752797683531377,1.,1.75095139468809));
#27711=CARTESIAN_POINT('Ctrl Pts',(-0.75400925402848,1.,1.75631083600175));
#27712=CARTESIAN_POINT('Ctrl Pts',(-0.755220979975262,1.,1.7619781724032));
#27713=CARTESIAN_POINT('Ctrl Pts',(-0.756421896028403,1.,1.76789396003141));
#27714=CARTESIAN_POINT('Ctrl Pts',(-0.757578264077238,1.,1.77394167108342));
#27715=CARTESIAN_POINT('Ctrl Pts',(-0.75865062667738,1.,1.77999411220912));
#27716=CARTESIAN_POINT('Ctrl Pts',(-0.759614401109868,1.,1.78596964884526));
#27717=CARTESIAN_POINT('Ctrl Pts',(-0.760469555880425,1.,1.79185815610802));
#27718=CARTESIAN_POINT('Ctrl Pts',(-0.761229695230359,1.,1.79768986997735));
#27719=CARTESIAN_POINT('Ctrl Pts',(-0.761915336443516,1.,1.80351583877334));
#27720=CARTESIAN_POINT('Ctrl Pts',(-0.762546129464036,1.,1.80938551463989));
#27721=CARTESIAN_POINT('Ctrl Pts',(-0.763132003836783,1.,1.81532118405566));
#27722=CARTESIAN_POINT('Ctrl Pts',(-0.763673465462854,1.,1.82131873145297));
#27723=CARTESIAN_POINT('Ctrl Pts',(-0.764165902606055,1.,1.8273599120008));
#27724=CARTESIAN_POINT('Ctrl Pts',(-0.764602549687845,1.,1.8334207722714));
#27725=CARTESIAN_POINT('Ctrl Pts',(-0.764978057881687,1.,1.83948181064823));
#27726=CARTESIAN_POINT('Ctrl Pts',(-0.765291664861971,1.,1.8455369887591));
#27727=CARTESIAN_POINT('Ctrl Pts',(-0.765545710619023,1.,1.85158945130054));
#27728=CARTESIAN_POINT('Ctrl Pts',(-0.765744212909305,1.,1.85764741390391));
#27729=CARTESIAN_POINT('Ctrl Pts',(-0.765891519092557,1.,1.86372027063314));
#27730=CARTESIAN_POINT('Ctrl Pts',(-0.765990708546111,1.,1.86981398314345));
#27731=CARTESIAN_POINT('Ctrl Pts',(-0.766042837036759,1.,1.87592888967886));
#27732=CARTESIAN_POINT('Ctrl Pts',(-0.766047794851869,1.,1.88206215302561));
#27733=CARTESIAN_POINT('Ctrl Pts',(-0.76600483706209,1.,1.88820926433409));
#27734=CARTESIAN_POINT('Ctrl Pts',(-0.765913193856979,1.,1.89436577771389));
#27735=CARTESIAN_POINT('Ctrl Pts',(-0.765772772593395,1.,1.90052930393599));
#27736=CARTESIAN_POINT('Ctrl Pts',(-0.765584196937936,1.,1.90669961402362));
#27737=CARTESIAN_POINT('Ctrl Pts',(-0.765348465884739,1.,1.91287765805174));
#27738=CARTESIAN_POINT('Ctrl Pts',(-0.765066729667095,1.,1.91906491634197));
#27739=CARTESIAN_POINT('Ctrl Pts',(-0.764740025488189,1.,1.92526263537041));
#27740=CARTESIAN_POINT('Ctrl Pts',(-0.764369010673889,1.,1.93147105496367));
#27741=CARTESIAN_POINT('Ctrl Pts',(-0.763954049121393,1.,1.93768964875867));
#27742=CARTESIAN_POINT('Ctrl Pts',(-0.76349533353858,1.,1.94391746617626));
#27743=CARTESIAN_POINT('Ctrl Pts',(-0.762992990878774,1.,1.95015342590025));
#27744=CARTESIAN_POINT('Ctrl Pts',(-0.762447203806263,1.,1.95639665309893));
#27745=CARTESIAN_POINT('Ctrl Pts',(-0.761858300014575,1.,1.96264672744229));
#27746=CARTESIAN_POINT('Ctrl Pts',(-0.761226690483986,1.,1.96890351582545));
#27747=CARTESIAN_POINT('Ctrl Pts',(-0.760552825409855,1.,1.97516705321521));
#27748=CARTESIAN_POINT('Ctrl Pts',(-0.759837147452135,1.,1.98143741418156));
#27749=CARTESIAN_POINT('Ctrl Pts',(-0.759080037802243,1.,1.98771456680806));
#27750=CARTESIAN_POINT('Ctrl Pts',(-0.758281796766377,1.,1.9939983109871));
#27751=CARTESIAN_POINT('Ctrl Pts',(-0.757442676862341,1.,2.00028834739072));
#27752=CARTESIAN_POINT('Ctrl Pts',(-0.756562904646496,1.,2.00658431587682));
#27753=CARTESIAN_POINT('Ctrl Pts',(-0.7556427049581,1.,2.01288584328149));
#27754=CARTESIAN_POINT('Ctrl Pts',(-0.75468233072352,1.,2.01919259406003));
#27755=CARTESIAN_POINT('Ctrl Pts',(-0.753682061113766,1.,2.02550428623587));
#27756=CARTESIAN_POINT('Ctrl Pts',(-0.752642180488104,1.,2.03182068456467));
#27757=CARTESIAN_POINT('Ctrl Pts',(-0.751562963361384,1.,2.03814160092173));
#27758=CARTESIAN_POINT('Ctrl Pts',(-0.750444657874758,1.,2.04446689147754));
#27759=CARTESIAN_POINT('Ctrl Pts',(-0.749287468663053,1.,2.05079645591606));
#27760=CARTESIAN_POINT('Ctrl Pts',(-0.748091554181101,1.,2.05713023030263));
#27761=CARTESIAN_POINT('Ctrl Pts',(-0.747103932785504,1.,2.06220058927162));
#27762=CARTESIAN_POINT('Ctrl Pts',(-0.746345871542696,1.,2.06600523016401));
#27763=CARTESIAN_POINT('Ctrl Pts',(-0.74583279137781,1.,2.06854248895575));
#27764=CARTESIAN_POINT('Ctrl Pts',(-0.745574324794401,1.,2.0698113262342));
#27765=CARTESIAN_POINT('',(-0.693717979106306,0.,1.60662857109684));
#27766=CARTESIAN_POINT('Origin',(0.,0.,0.));
#27767=CARTESIAN_POINT('',(-0.892032620296855,1.,1.5055822144029));
#27768=CARTESIAN_POINT('Origin',(0.,1.,0.));
#27769=CARTESIAN_POINT('',(-0.892032620296855,0.,1.5055822144029));
#27770=CARTESIAN_POINT('Ctrl Pts',(-1.23627494547115,-1.,1.81978687191668));
#27771=CARTESIAN_POINT('Ctrl Pts',(-1.23627494547115,1.,1.81978687191668));
#27772=CARTESIAN_POINT('Ctrl Pts',(-1.23509651170476,-1.,1.81925017193666));
#27773=CARTESIAN_POINT('Ctrl Pts',(-1.23509651170476,1.,1.81925017193666));
#27774=CARTESIAN_POINT('Ctrl Pts',(-1.2327422452705,-1.,1.81817389921279));
#27775=CARTESIAN_POINT('Ctrl Pts',(-1.2327422452705,1.,1.81817389921279));
#27776=CARTESIAN_POINT('Ctrl Pts',(-1.2292186489137,-1.,1.8165508718364));
#27777=CARTESIAN_POINT('Ctrl Pts',(-1.2292186489137,1.,1.8165508718364));
#27778=CARTESIAN_POINT('Ctrl Pts',(-1.2245361330495,-1.,1.81436959210434));
#27779=CARTESIAN_POINT('Ctrl Pts',(-1.2245361330495,1.,1.81436959210434));
#27780=CARTESIAN_POINT('Ctrl Pts',(-1.21870906103557,-1.,1.81161420806656));
#27781=CARTESIAN_POINT('Ctrl Pts',(-1.21870906103557,1.,1.81161420806656));
#27782=CARTESIAN_POINT('Ctrl Pts',(-1.21290815708314,-1.,1.80882996917129));
#27783=CARTESIAN_POINT('Ctrl Pts',(-1.21290815708314,1.,1.80882996917129));
#27784=CARTESIAN_POINT('Ctrl Pts',(-1.20713356605475,-1.,1.80601678480707));
#27785=CARTESIAN_POINT('Ctrl Pts',(-1.20713356605475,1.,1.80601678480707));
#27786=CARTESIAN_POINT('Ctrl Pts',(-1.20138548938974,-1.,1.80317454838603));
#27787=CARTESIAN_POINT('Ctrl Pts',(-1.20138548938974,1.,1.80317454838603));
#27788=CARTESIAN_POINT('Ctrl Pts',(-1.19566418930242,-1.,1.80030314369879));
#27789=CARTESIAN_POINT('Ctrl Pts',(-1.19566418930242,1.,1.80030314369879));
#27790=CARTESIAN_POINT('Ctrl Pts',(-1.18996997934445,-1.,1.79740245923478));
#27791=CARTESIAN_POINT('Ctrl Pts',(-1.18996997934445,1.,1.79740245923478));
#27792=CARTESIAN_POINT('Ctrl Pts',(-1.18430321697432,-1.,1.79447240321515));
#27793=CARTESIAN_POINT('Ctrl Pts',(-1.18430321697432,1.,1.79447240321515));
#27794=CARTESIAN_POINT('Ctrl Pts',(-1.17866429440809,-1.,1.79151291552689));
#27795=CARTESIAN_POINT('Ctrl Pts',(-1.17866429440809,1.,1.79151291552689));
#27796=CARTESIAN_POINT('Ctrl Pts',(-1.17305363177328,-1.,1.78852398877616));
#27797=CARTESIAN_POINT('Ctrl Pts',(-1.17305363177328,1.,1.78852398877616));
#27798=CARTESIAN_POINT('Ctrl Pts',(-1.16747166312303,-1.,1.78550566040443));
#27799=CARTESIAN_POINT('Ctrl Pts',(-1.16747166312303,1.,1.78550566040443));
#27800=CARTESIAN_POINT('Ctrl Pts',(-1.16191881298499,-1.,1.78245795881009));
#27801=CARTESIAN_POINT('Ctrl Pts',(-1.16191881298499,1.,1.78245795881009));
#27802=CARTESIAN_POINT('Ctrl Pts',(-1.15639547194698,-1.,1.77938085564275));
#27803=CARTESIAN_POINT('Ctrl Pts',(-1.15639547194698,1.,1.77938085564275));
#27804=CARTESIAN_POINT('Ctrl Pts',(-1.15090197841515,-1.,1.7762742255701));
#27805=CARTESIAN_POINT('Ctrl Pts',(-1.15090197841515,1.,1.7762742255701));
#27806=CARTESIAN_POINT('Ctrl Pts',(-1.1454385822692,-1.,1.77313777896194));
#27807=CARTESIAN_POINT('Ctrl Pts',(-1.1454385822692,1.,1.77313777896194));
#27808=CARTESIAN_POINT('Ctrl Pts',(-1.14000548336975,-1.,1.76997111386769));
#27809=CARTESIAN_POINT('Ctrl Pts',(-1.14000548336975,1.,1.76997111386769));
#27810=CARTESIAN_POINT('Ctrl Pts',(-1.1346029180462,-1.,1.76677384551862));
#27811=CARTESIAN_POINT('Ctrl Pts',(-1.1346029180462,1.,1.76677384551862));
#27812=CARTESIAN_POINT('Ctrl Pts',(-1.12923123555075,-1.,1.7635457196617));
#27813=CARTESIAN_POINT('Ctrl Pts',(-1.12923123555075,1.,1.7635457196617));
#27814=CARTESIAN_POINT('Ctrl Pts',(-1.12389096855086,-1.,1.76028671825096));
#27815=CARTESIAN_POINT('Ctrl Pts',(-1.12389096855086,1.,1.76028671825096));
#27816=CARTESIAN_POINT('Ctrl Pts',(-1.11858293216763,-1.,1.75699720772105));
#27817=CARTESIAN_POINT('Ctrl Pts',(-1.11858293216763,1.,1.75699720772105));
#27818=CARTESIAN_POINT('Ctrl Pts',(-1.11330807582551,-1.,1.7536777209463));
#27819=CARTESIAN_POINT('Ctrl Pts',(-1.11330807582551,1.,1.7536777209463));
#27820=CARTESIAN_POINT('Ctrl Pts',(-1.10806728183007,-1.,1.7503286607592));
#27821=CARTESIAN_POINT('Ctrl Pts',(-1.10806728183007,1.,1.7503286607592));
#27822=CARTESIAN_POINT('Ctrl Pts',(-1.10286118991143,-1.,1.74695004214923));
#27823=CARTESIAN_POINT('Ctrl Pts',(-1.10286118991143,1.,1.74695004214923));
#27824=CARTESIAN_POINT('Ctrl Pts',(-1.09768999241225,-1.,1.74354119236208));
#27825=CARTESIAN_POINT('Ctrl Pts',(-1.09768999241225,1.,1.74354119236208));
#27826=CARTESIAN_POINT('Ctrl Pts',(-1.09255329056493,-1.,1.74010053962247));
#27827=CARTESIAN_POINT('Ctrl Pts',(-1.09255329056493,1.,1.74010053962247));
#27828=CARTESIAN_POINT('Ctrl Pts',(-1.08745056285427,-1.,1.73662628326091));
#27829=CARTESIAN_POINT('Ctrl Pts',(-1.08745056285427,1.,1.73662628326091));
#27830=CARTESIAN_POINT('Ctrl Pts',(-1.08238162784749,-1.,1.73311705663407));
#27831=CARTESIAN_POINT('Ctrl Pts',(-1.08238162784749,1.,1.73311705663407));
#27832=CARTESIAN_POINT('Ctrl Pts',(-1.0773470373727,-1.,1.72957248977424));
#27833=CARTESIAN_POINT('Ctrl Pts',(-1.0773470373727,1.,1.72957248977424));
#27834=CARTESIAN_POINT('Ctrl Pts',(-1.07234866990252,-1.,1.72599406198488));
#27835=CARTESIAN_POINT('Ctrl Pts',(-1.07234866990252,1.,1.72599406198488));
#27836=CARTESIAN_POINT('Ctrl Pts',(-1.06738966975462,-1.,1.72238500928453));
#27837=CARTESIAN_POINT('Ctrl Pts',(-1.06738966975462,1.,1.72238500928453));
#27838=CARTESIAN_POINT('Ctrl Pts',(-1.06247324680647,-1.,1.71874858456904));
#27839=CARTESIAN_POINT('Ctrl Pts',(-1.06247324680647,1.,1.71874858456904));
#27840=CARTESIAN_POINT('Ctrl Pts',(-1.05760163192479,-1.,1.7150865442702));
#27841=CARTESIAN_POINT('Ctrl Pts',(-1.05760163192479,1.,1.7150865442702));
#27842=CARTESIAN_POINT('Ctrl Pts',(-1.05277517202855,-1.,1.71139783543989));
#27843=CARTESIAN_POINT('Ctrl Pts',(-1.05277517202855,1.,1.71139783543989));
#27844=CARTESIAN_POINT('Ctrl Pts',(-1.04799085404995,-1.,1.70767646263649));
#27845=CARTESIAN_POINT('Ctrl Pts',(-1.04799085404995,1.,1.70767646263649));
#27846=CARTESIAN_POINT('Ctrl Pts',(-1.04324363334554,-1.,1.70391338707982));
#27847=CARTESIAN_POINT('Ctrl Pts',(-1.04324363334554,1.,1.70391338707982));
#27848=CARTESIAN_POINT('Ctrl Pts',(-1.03852922490789,-1.,1.70010052930962));
#27849=CARTESIAN_POINT('Ctrl Pts',(-1.03852922490789,1.,1.70010052930962));
#27850=CARTESIAN_POINT('Ctrl Pts',(-1.03384646003588,-1.,1.69623414782771));
#27851=CARTESIAN_POINT('Ctrl Pts',(-1.03384646003588,1.,1.69623414782771));
#27852=CARTESIAN_POINT('Ctrl Pts',(-1.02919977579147,-1.,1.69231840863458));
#27853=CARTESIAN_POINT('Ctrl Pts',(-1.02919977579147,1.,1.69231840863458));
#27854=CARTESIAN_POINT('Ctrl Pts',(-1.02460180535255,-1.,1.68836910178447));
#27855=CARTESIAN_POINT('Ctrl Pts',(-1.02460180535255,1.,1.68836910178447));
#27856=CARTESIAN_POINT('Ctrl Pts',(-1.02006795074201,-1.,1.68440578021706));
#27857=CARTESIAN_POINT('Ctrl Pts',(-1.02006795074201,1.,1.68440578021706));
#27858=CARTESIAN_POINT('Ctrl Pts',(-1.01561026162773,-1.,1.68044289894798));
#27859=CARTESIAN_POINT('Ctrl Pts',(-1.01561026162773,1.,1.68044289894798));
#27860=CARTESIAN_POINT('Ctrl Pts',(-1.01123236493511,-1.,1.67648246776464));
#27861=CARTESIAN_POINT('Ctrl Pts',(-1.01123236493511,1.,1.67648246776464));
#27862=CARTESIAN_POINT('Ctrl Pts',(-1.00692206696414,-1.,1.67250335383293));
#27863=CARTESIAN_POINT('Ctrl Pts',(-1.00692206696414,1.,1.67250335383293));
#27864=CARTESIAN_POINT('Ctrl Pts',(-1.00265091003727,-1.,1.66846059277303));
#27865=CARTESIAN_POINT('Ctrl Pts',(-1.00265091003727,1.,1.66846059277303));
#27866=CARTESIAN_POINT('Ctrl Pts',(-0.998389654952758,-1.,1.66430758030376));
#27867=CARTESIAN_POINT('Ctrl Pts',(-0.998389654952758,1.,1.66430758030376));
#27868=CARTESIAN_POINT('Ctrl Pts',(-0.994121836661306,-1.,1.66001553809947));
#27869=CARTESIAN_POINT('Ctrl Pts',(-0.994121836661306,1.,1.66001553809947));
#27870=CARTESIAN_POINT('Ctrl Pts',(-0.989855627854165,-1.,1.65559044289699));
#27871=CARTESIAN_POINT('Ctrl Pts',(-0.989855627854165,1.,1.65559044289699));
#27872=CARTESIAN_POINT('Ctrl Pts',(-0.985642622920821,-1.,1.65110016612638));
#27873=CARTESIAN_POINT('Ctrl Pts',(-0.985642622920821,1.,1.65110016612638));
#27874=CARTESIAN_POINT('Ctrl Pts',(-0.981562530939489,-1.,1.64665139190656));
#27875=CARTESIAN_POINT('Ctrl Pts',(-0.981562530939489,1.,1.64665139190656));
#27876=CARTESIAN_POINT('Ctrl Pts',(-0.977689794119416,-1.,1.64233990826687));
#27877=CARTESIAN_POINT('Ctrl Pts',(-0.977689794119416,1.,1.64233990826687));
#27878=CARTESIAN_POINT('Ctrl Pts',(-0.974066058287418,-1.,1.63820952658144));
#27879=CARTESIAN_POINT('Ctrl Pts',(-0.974066058287418,1.,1.63820952658144));
#27880=CARTESIAN_POINT('Ctrl Pts',(-0.970669715997509,-1.,1.63420665729798));
#27881=CARTESIAN_POINT('Ctrl Pts',(-0.970669715997509,1.,1.63420665729798));
#27882=CARTESIAN_POINT('Ctrl Pts',(-0.967387853230345,-1.,1.63013849959461));
#27883=CARTESIAN_POINT('Ctrl Pts',(-0.967387853230345,1.,1.63013849959461));
#27884=CARTESIAN_POINT('Ctrl Pts',(-0.964046107040536,-1.,1.62571930670187));
#27885=CARTESIAN_POINT('Ctrl Pts',(-0.964046107040536,1.,1.62571930670187));
#27886=CARTESIAN_POINT('Ctrl Pts',(-0.960438326101729,-1.,1.62061638140221));
#27887=CARTESIAN_POINT('Ctrl Pts',(-0.960438326101729,1.,1.62061638140221));
#27888=CARTESIAN_POINT('Ctrl Pts',(-0.956354422920671,-1.,1.61449324337085));
#27889=CARTESIAN_POINT('Ctrl Pts',(-0.956354422920671,1.,1.61449324337085));
#27890=CARTESIAN_POINT('Ctrl Pts',(-0.951613284356035,-1.,1.60706069896936));
#27891=CARTESIAN_POINT('Ctrl Pts',(-0.951613284356035,1.,1.60706069896936));
#27892=CARTESIAN_POINT('Ctrl Pts',(-0.946078063315257,-1.,1.59810042043673));
#27893=CARTESIAN_POINT('Ctrl Pts',(-0.946078063315257,1.,1.59810042043673));
#27894=CARTESIAN_POINT('Ctrl Pts',(-0.939646377893399,-1.,1.58744937487176));
#27895=CARTESIAN_POINT('Ctrl Pts',(-0.939646377893399,1.,1.58744937487176));
#27896=CARTESIAN_POINT('Ctrl Pts',(-0.932246680108685,-1.,1.57499388382243));
#27897=CARTESIAN_POINT('Ctrl Pts',(-0.932246680108685,1.,1.57499388382243));
#27898=CARTESIAN_POINT('Ctrl Pts',(-0.923832188944341,-1.,1.56065988578893));
#27899=CARTESIAN_POINT('Ctrl Pts',(-0.923832188944341,1.,1.56065988578893));
#27900=CARTESIAN_POINT('Ctrl Pts',(-0.914375919026456,-1.,1.54440491149498));
#27901=CARTESIAN_POINT('Ctrl Pts',(-0.914375919026456,1.,1.54440491149498));
#27902=CARTESIAN_POINT('Ctrl Pts',(-0.905967409625651,-1.,1.52984849887993));
#27903=CARTESIAN_POINT('Ctrl Pts',(-0.905967409625651,1.,1.52984849887993));
#27904=CARTESIAN_POINT('Ctrl Pts',(-0.899185047483511,-1.,1.51805569590094));
#27905=CARTESIAN_POINT('Ctrl Pts',(-0.899185047483511,1.,1.51805569590094));
#27906=CARTESIAN_POINT('Ctrl Pts',(-0.894452006964543,-1.,1.50980486806688));
#27907=CARTESIAN_POINT('Ctrl Pts',(-0.894452006964543,1.,1.50980486806688));
#27908=CARTESIAN_POINT('Ctrl Pts',(-0.892032620296855,-1.,1.5055822144029));
#27909=CARTESIAN_POINT('Ctrl Pts',(-0.892032620296855,1.,1.5055822144029));
#27910=CARTESIAN_POINT('',(-1.23627494547115,1.,1.81978687191668));
#27911=CARTESIAN_POINT('Ctrl Pts',(-1.23627494547115,1.,1.81978687191668));
#27912=CARTESIAN_POINT('Ctrl Pts',(-1.23509651170476,1.,1.81925017193666));
#27913=CARTESIAN_POINT('Ctrl Pts',(-1.2327422452705,1.,1.81817389921279));
#27914=CARTESIAN_POINT('Ctrl Pts',(-1.2292186489137,1.,1.8165508718364));
#27915=CARTESIAN_POINT('Ctrl Pts',(-1.2245361330495,1.,1.81436959210434));
#27916=CARTESIAN_POINT('Ctrl Pts',(-1.21870906103557,1.,1.81161420806656));
#27917=CARTESIAN_POINT('Ctrl Pts',(-1.21290815708314,1.,1.80882996917129));
#27918=CARTESIAN_POINT('Ctrl Pts',(-1.20713356605475,1.,1.80601678480707));
#27919=CARTESIAN_POINT('Ctrl Pts',(-1.20138548938974,1.,1.80317454838603));
#27920=CARTESIAN_POINT('Ctrl Pts',(-1.19566418930242,1.,1.80030314369879));
#27921=CARTESIAN_POINT('Ctrl Pts',(-1.18996997934445,1.,1.79740245923478));
#27922=CARTESIAN_POINT('Ctrl Pts',(-1.18430321697432,1.,1.79447240321515));
#27923=CARTESIAN_POINT('Ctrl Pts',(-1.17866429440809,1.,1.79151291552689));
#27924=CARTESIAN_POINT('Ctrl Pts',(-1.17305363177328,1.,1.78852398877616));
#27925=CARTESIAN_POINT('Ctrl Pts',(-1.16747166312303,1.,1.78550566040443));
#27926=CARTESIAN_POINT('Ctrl Pts',(-1.16191881298499,1.,1.78245795881009));
#27927=CARTESIAN_POINT('Ctrl Pts',(-1.15639547194698,1.,1.77938085564275));
#27928=CARTESIAN_POINT('Ctrl Pts',(-1.15090197841515,1.,1.7762742255701));
#27929=CARTESIAN_POINT('Ctrl Pts',(-1.1454385822692,1.,1.77313777896194));
#27930=CARTESIAN_POINT('Ctrl Pts',(-1.14000548336975,1.,1.76997111386769));
#27931=CARTESIAN_POINT('Ctrl Pts',(-1.1346029180462,1.,1.76677384551862));
#27932=CARTESIAN_POINT('Ctrl Pts',(-1.12923123555075,1.,1.7635457196617));
#27933=CARTESIAN_POINT('Ctrl Pts',(-1.12389096855086,1.,1.76028671825096));
#27934=CARTESIAN_POINT('Ctrl Pts',(-1.11858293216763,1.,1.75699720772105));
#27935=CARTESIAN_POINT('Ctrl Pts',(-1.11330807582551,1.,1.7536777209463));
#27936=CARTESIAN_POINT('Ctrl Pts',(-1.10806728183007,1.,1.7503286607592));
#27937=CARTESIAN_POINT('Ctrl Pts',(-1.10286118991143,1.,1.74695004214923));
#27938=CARTESIAN_POINT('Ctrl Pts',(-1.09768999241225,1.,1.74354119236208));
#27939=CARTESIAN_POINT('Ctrl Pts',(-1.09255329056493,1.,1.74010053962247));
#27940=CARTESIAN_POINT('Ctrl Pts',(-1.08745056285427,1.,1.73662628326091));
#27941=CARTESIAN_POINT('Ctrl Pts',(-1.08238162784749,1.,1.73311705663407));
#27942=CARTESIAN_POINT('Ctrl Pts',(-1.0773470373727,1.,1.72957248977424));
#27943=CARTESIAN_POINT('Ctrl Pts',(-1.07234866990252,1.,1.72599406198488));
#27944=CARTESIAN_POINT('Ctrl Pts',(-1.06738966975462,1.,1.72238500928453));
#27945=CARTESIAN_POINT('Ctrl Pts',(-1.06247324680647,1.,1.71874858456904));
#27946=CARTESIAN_POINT('Ctrl Pts',(-1.05760163192479,1.,1.7150865442702));
#27947=CARTESIAN_POINT('Ctrl Pts',(-1.05277517202855,1.,1.71139783543989));
#27948=CARTESIAN_POINT('Ctrl Pts',(-1.04799085404995,1.,1.70767646263649));
#27949=CARTESIAN_POINT('Ctrl Pts',(-1.04324363334554,1.,1.70391338707982));
#27950=CARTESIAN_POINT('Ctrl Pts',(-1.03852922490789,1.,1.70010052930962));
#27951=CARTESIAN_POINT('Ctrl Pts',(-1.03384646003588,1.,1.69623414782771));
#27952=CARTESIAN_POINT('Ctrl Pts',(-1.02919977579147,1.,1.69231840863458));
#27953=CARTESIAN_POINT('Ctrl Pts',(-1.02460180535255,1.,1.68836910178447));
#27954=CARTESIAN_POINT('Ctrl Pts',(-1.02006795074201,1.,1.68440578021706));
#27955=CARTESIAN_POINT('Ctrl Pts',(-1.01561026162773,1.,1.68044289894798));
#27956=CARTESIAN_POINT('Ctrl Pts',(-1.01123236493511,1.,1.67648246776464));
#27957=CARTESIAN_POINT('Ctrl Pts',(-1.00692206696414,1.,1.67250335383293));
#27958=CARTESIAN_POINT('Ctrl Pts',(-1.00265091003727,1.,1.66846059277303));
#27959=CARTESIAN_POINT('Ctrl Pts',(-0.998389654952758,1.,1.66430758030376));
#27960=CARTESIAN_POINT('Ctrl Pts',(-0.994121836661306,1.,1.66001553809947));
#27961=CARTESIAN_POINT('Ctrl Pts',(-0.989855627854165,1.,1.65559044289699));
#27962=CARTESIAN_POINT('Ctrl Pts',(-0.985642622920821,1.,1.65110016612638));
#27963=CARTESIAN_POINT('Ctrl Pts',(-0.981562530939489,1.,1.64665139190656));
#27964=CARTESIAN_POINT('Ctrl Pts',(-0.977689794119416,1.,1.64233990826687));
#27965=CARTESIAN_POINT('Ctrl Pts',(-0.974066058287418,1.,1.63820952658144));
#27966=CARTESIAN_POINT('Ctrl Pts',(-0.970669715997509,1.,1.63420665729798));
#27967=CARTESIAN_POINT('Ctrl Pts',(-0.967387853230345,1.,1.63013849959461));
#27968=CARTESIAN_POINT('Ctrl Pts',(-0.964046107040536,1.,1.62571930670187));
#27969=CARTESIAN_POINT('Ctrl Pts',(-0.960438326101729,1.,1.62061638140221));
#27970=CARTESIAN_POINT('Ctrl Pts',(-0.956354422920671,1.,1.61449324337085));
#27971=CARTESIAN_POINT('Ctrl Pts',(-0.951613284356035,1.,1.60706069896936));
#27972=CARTESIAN_POINT('Ctrl Pts',(-0.946078063315257,1.,1.59810042043673));
#27973=CARTESIAN_POINT('Ctrl Pts',(-0.939646377893399,1.,1.58744937487176));
#27974=CARTESIAN_POINT('Ctrl Pts',(-0.932246680108685,1.,1.57499388382243));
#27975=CARTESIAN_POINT('Ctrl Pts',(-0.923832188944341,1.,1.56065988578893));
#27976=CARTESIAN_POINT('Ctrl Pts',(-0.914375919026456,1.,1.54440491149498));
#27977=CARTESIAN_POINT('Ctrl Pts',(-0.905967409625651,1.,1.52984849887993));
#27978=CARTESIAN_POINT('Ctrl Pts',(-0.899185047483511,1.,1.51805569590094));
#27979=CARTESIAN_POINT('Ctrl Pts',(-0.894452006964543,1.,1.50980486806688));
#27980=CARTESIAN_POINT('Ctrl Pts',(-0.892032620296855,1.,1.5055822144029));
#27981=CARTESIAN_POINT('',(-1.23627494547115,0.,1.81978687191668));
#27982=CARTESIAN_POINT('Origin',(-1.34869019493419,0.,1.73811241238545));
#27983=CARTESIAN_POINT('',(-1.34869019493419,1.,1.73811241238545));
#27984=CARTESIAN_POINT('',(-1.23627494547115,1.,1.81978687191668));
#27985=CARTESIAN_POINT('',(-1.34869019493419,0.,1.73811241238545));
#27986=CARTESIAN_POINT('Ctrl Pts',(-1.15624053661742,-1.,1.31362392696032));
#27987=CARTESIAN_POINT('Ctrl Pts',(-1.15624053661742,1.,1.31362392696032));
#27988=CARTESIAN_POINT('Ctrl Pts',(-1.15950888730809,-1.,1.31722977216397));
#27989=CARTESIAN_POINT('Ctrl Pts',(-1.15950888730809,1.,1.31722977216397));
#27990=CARTESIAN_POINT('Ctrl Pts',(-1.16589330093588,-1.,1.32428080721772));
#27991=CARTESIAN_POINT('Ctrl Pts',(-1.16589330093588,1.,1.32428080721772));
#27992=CARTESIAN_POINT('Ctrl Pts',(-1.17501305789857,-1.,1.33437539347008));
#27993=CARTESIAN_POINT('Ctrl Pts',(-1.17501305789857,1.,1.33437539347008));
#27994=CARTESIAN_POINT('Ctrl Pts',(-1.18625865667441,-1.,1.34687054001093));
#27995=CARTESIAN_POINT('Ctrl Pts',(-1.18625865667441,1.,1.34687054001093));
#27996=CARTESIAN_POINT('Ctrl Pts',(-1.1987959077932,-1.,1.36088705043885));
#27997=CARTESIAN_POINT('Ctrl Pts',(-1.1987959077932,1.,1.36088705043885));
#27998=CARTESIAN_POINT('Ctrl Pts',(-1.20982812925645,-1.,1.37331915607905));
#27999=CARTESIAN_POINT('Ctrl Pts',(-1.20982812925645,1.,1.37331915607905));
#28000=CARTESIAN_POINT('Ctrl Pts',(-1.21938737280852,-1.,1.38420564527715));
#28001=CARTESIAN_POINT('Ctrl Pts',(-1.21938737280852,1.,1.38420564527715));
#28002=CARTESIAN_POINT('Ctrl Pts',(-1.22752961899387,-1.,1.39361389568796));
#28003=CARTESIAN_POINT('Ctrl Pts',(-1.22752961899387,1.,1.39361389568796));
#28004=CARTESIAN_POINT('Ctrl Pts',(-1.23434087290423,-1.,1.40164708206106));
#28005=CARTESIAN_POINT('Ctrl Pts',(-1.23434087290423,1.,1.40164708206106));
#28006=CARTESIAN_POINT('Ctrl Pts',(-1.23994455029534,-1.,1.40845295531283));
#28007=CARTESIAN_POINT('Ctrl Pts',(-1.23994455029534,1.,1.40845295531283));
#28008=CARTESIAN_POINT('Ctrl Pts',(-1.24450600513056,-1.,1.41422913175179));
#28009=CARTESIAN_POINT('Ctrl Pts',(-1.24450600513056,1.,1.41422913175179));
#28010=CARTESIAN_POINT('Ctrl Pts',(-1.24824430986571,-1.,1.41923722596025));
#28011=CARTESIAN_POINT('Ctrl Pts',(-1.24824430986571,1.,1.41923722596025));
#28012=CARTESIAN_POINT('Ctrl Pts',(-1.2514145557001,-1.,1.42378102115575));
#28013=CARTESIAN_POINT('Ctrl Pts',(-1.2514145557001,1.,1.42378102115575));
#28014=CARTESIAN_POINT('Ctrl Pts',(-1.25426945222639,-1.,1.42815938799387));
#28015=CARTESIAN_POINT('Ctrl Pts',(-1.25426945222639,1.,1.42815938799387));
#28016=CARTESIAN_POINT('Ctrl Pts',(-1.25702687965755,-1.,1.43262645609691));
#28017=CARTESIAN_POINT('Ctrl Pts',(-1.25702687965755,1.,1.43262645609691));
#28018=CARTESIAN_POINT('Ctrl Pts',(-1.25983531012005,-1.,1.43734919180848));
#28019=CARTESIAN_POINT('Ctrl Pts',(-1.25983531012005,1.,1.43734919180848));
#28020=CARTESIAN_POINT('Ctrl Pts',(-1.26273903323859,-1.,1.44236470511303));
#28021=CARTESIAN_POINT('Ctrl Pts',(-1.26273903323859,1.,1.44236470511303));
#28022=CARTESIAN_POINT('Ctrl Pts',(-1.26570925118868,-1.,1.44761985001662));
#28023=CARTESIAN_POINT('Ctrl Pts',(-1.26570925118868,1.,1.44761985001662));
#28024=CARTESIAN_POINT('Ctrl Pts',(-1.2686778680489,-1.,1.45301422764247));
#28025=CARTESIAN_POINT('Ctrl Pts',(-1.2686778680489,1.,1.45301422764247));
#28026=CARTESIAN_POINT('Ctrl Pts',(-1.27156805265289,-1.,1.45843906294697));
#28027=CARTESIAN_POINT('Ctrl Pts',(-1.27156805265289,1.,1.45843906294697));
#28028=CARTESIAN_POINT('Ctrl Pts',(-1.27433119897822,-1.,1.46382431332476));
#28029=CARTESIAN_POINT('Ctrl Pts',(-1.27433119897822,1.,1.46382431332476));
#28030=CARTESIAN_POINT('Ctrl Pts',(-1.27696414831089,-1.,1.46916035917133));
#28031=CARTESIAN_POINT('Ctrl Pts',(-1.27696414831089,1.,1.46916035917133));
#28032=CARTESIAN_POINT('Ctrl Pts',(-1.2794891824849,-1.,1.4744717526707));
#28033=CARTESIAN_POINT('Ctrl Pts',(-1.2794891824849,1.,1.4744717526707));
#28034=CARTESIAN_POINT('Ctrl Pts',(-1.28194158939517,-1.,1.47980070347095));
#28035=CARTESIAN_POINT('Ctrl Pts',(-1.28194158939517,1.,1.47980070347095));
#28036=CARTESIAN_POINT('Ctrl Pts',(-1.28435533880201,-1.,1.4851881711891));
#28037=CARTESIAN_POINT('Ctrl Pts',(-1.28435533880201,1.,1.4851881711891));
#28038=CARTESIAN_POINT('Ctrl Pts',(-1.2867467611644,-1.,1.4906522831278));
#28039=CARTESIAN_POINT('Ctrl Pts',(-1.2867467611644,1.,1.4906522831278));
#28040=CARTESIAN_POINT('Ctrl Pts',(-1.28911506584254,-1.,1.49618896881754));
#28041=CARTESIAN_POINT('Ctrl Pts',(-1.28911506584254,1.,1.49618896881754));
#28042=CARTESIAN_POINT('Ctrl Pts',(-1.29145022885181,-1.,1.50178230149776));
#28043=CARTESIAN_POINT('Ctrl Pts',(-1.29145022885181,1.,1.50178230149776));
#28044=CARTESIAN_POINT('Ctrl Pts',(-1.29373841372842,-1.,1.50741159078365));
#28045=CARTESIAN_POINT('Ctrl Pts',(-1.29373841372842,1.,1.50741159078365));
#28046=CARTESIAN_POINT('Ctrl Pts',(-1.29596850710509,-1.,1.51305994241402));
#28047=CARTESIAN_POINT('Ctrl Pts',(-1.29596850710509,1.,1.51305994241402));
#28048=CARTESIAN_POINT('Ctrl Pts',(-1.29813791800747,-1.,1.51872184912724));
#28049=CARTESIAN_POINT('Ctrl Pts',(-1.29813791800747,1.,1.51872184912724));
#28050=CARTESIAN_POINT('Ctrl Pts',(-1.30024984366328,-1.,1.52439957861062));
#28051=CARTESIAN_POINT('Ctrl Pts',(-1.30024984366328,1.,1.52439957861062));
#28052=CARTESIAN_POINT('Ctrl Pts',(-1.30231064395568,-1.,1.53009970283891));
#28053=CARTESIAN_POINT('Ctrl Pts',(-1.30231064395568,1.,1.53009970283891));
#28054=CARTESIAN_POINT('Ctrl Pts',(-1.30432735639489,-1.,1.53582981268977));
#28055=CARTESIAN_POINT('Ctrl Pts',(-1.30432735639489,1.,1.53582981268977));
#28056=CARTESIAN_POINT('Ctrl Pts',(-1.30630475189556,-1.,1.54159462645432));
#28057=CARTESIAN_POINT('Ctrl Pts',(-1.30630475189556,1.,1.54159462645432));
#28058=CARTESIAN_POINT('Ctrl Pts',(-1.30824393907473,-1.,1.54739413957185));
#28059=CARTESIAN_POINT('Ctrl Pts',(-1.30824393907473,1.,1.54739413957185));
#28060=CARTESIAN_POINT('Ctrl Pts',(-1.31014393684222,-1.,1.55322568759481));
#28061=CARTESIAN_POINT('Ctrl Pts',(-1.31014393684222,1.,1.55322568759481));
#28062=CARTESIAN_POINT('Ctrl Pts',(-1.31200264341696,-1.,1.55908521254821));
#28063=CARTESIAN_POINT('Ctrl Pts',(-1.31200264341696,1.,1.55908521254821));
#28064=CARTESIAN_POINT('Ctrl Pts',(-1.31381795281002,-1.,1.56496872402353));
#28065=CARTESIAN_POINT('Ctrl Pts',(-1.31381795281002,1.,1.56496872402353));
#28066=CARTESIAN_POINT('Ctrl Pts',(-1.31558903860016,-1.,1.57087397835723));
#28067=CARTESIAN_POINT('Ctrl Pts',(-1.31558903860016,1.,1.57087397835723));
#28068=CARTESIAN_POINT('Ctrl Pts',(-1.31731642317187,-1.,1.5768005650559));
#28069=CARTESIAN_POINT('Ctrl Pts',(-1.31731642317187,1.,1.5768005650559));
#28070=CARTESIAN_POINT('Ctrl Pts',(-1.31900135021432,-1.,1.58274907898834));
#28071=CARTESIAN_POINT('Ctrl Pts',(-1.31900135021432,1.,1.58274907898834));
#28072=CARTESIAN_POINT('Ctrl Pts',(-1.32064537110892,-1.,1.58872057258245));
#28073=CARTESIAN_POINT('Ctrl Pts',(-1.32064537110892,1.,1.58872057258245));
#28074=CARTESIAN_POINT('Ctrl Pts',(-1.32224985747682,-1.,1.59471591079403));
#28075=CARTESIAN_POINT('Ctrl Pts',(-1.32224985747682,1.,1.59471591079403));
#28076=CARTESIAN_POINT('Ctrl Pts',(-1.32381550858256,-1.,1.60073511858687));
#28077=CARTESIAN_POINT('Ctrl Pts',(-1.32381550858256,1.,1.60073511858687));
#28078=CARTESIAN_POINT('Ctrl Pts',(-1.32534250785782,-1.,1.60677758290954));
#28079=CARTESIAN_POINT('Ctrl Pts',(-1.32534250785782,1.,1.60677758290954));
#28080=CARTESIAN_POINT('Ctrl Pts',(-1.32683074483356,-1.,1.6128423401575));
#28081=CARTESIAN_POINT('Ctrl Pts',(-1.32683074483356,1.,1.6128423401575));
#28082=CARTESIAN_POINT('Ctrl Pts',(-1.32828000610449,-1.,1.61892832270724));
#28083=CARTESIAN_POINT('Ctrl Pts',(-1.32828000610449,1.,1.61892832270724));
#28084=CARTESIAN_POINT('Ctrl Pts',(-1.3296901950568,-1.,1.62503464209797));
#28085=CARTESIAN_POINT('Ctrl Pts',(-1.3296901950568,1.,1.62503464209797));
#28086=CARTESIAN_POINT('Ctrl Pts',(-1.33106149345645,-1.,1.63116079730923));
#28087=CARTESIAN_POINT('Ctrl Pts',(-1.33106149345645,1.,1.63116079730923));
#28088=CARTESIAN_POINT('Ctrl Pts',(-1.33239425103724,-1.,1.63730653475089));
#28089=CARTESIAN_POINT('Ctrl Pts',(-1.33239425103724,1.,1.63730653475089));
#28090=CARTESIAN_POINT('Ctrl Pts',(-1.33368890676572,-1.,1.6434717485603));
#28091=CARTESIAN_POINT('Ctrl Pts',(-1.33368890676572,1.,1.6434717485603));
#28092=CARTESIAN_POINT('Ctrl Pts',(-1.33494590467993,-1.,1.6496563728683));
#28093=CARTESIAN_POINT('Ctrl Pts',(-1.33494590467993,1.,1.6496563728683));
#28094=CARTESIAN_POINT('Ctrl Pts',(-1.33616559745172,-1.,1.65586025952593));
#28095=CARTESIAN_POINT('Ctrl Pts',(-1.33616559745172,1.,1.65586025952593));
#28096=CARTESIAN_POINT('Ctrl Pts',(-1.33734820885262,-1.,1.66208312541983));
#28097=CARTESIAN_POINT('Ctrl Pts',(-1.33734820885262,1.,1.66208312541983));
#28098=CARTESIAN_POINT('Ctrl Pts',(-1.33849388654388,-1.,1.66832460783989));
#28099=CARTESIAN_POINT('Ctrl Pts',(-1.33849388654388,1.,1.66832460783989));
#28100=CARTESIAN_POINT('Ctrl Pts',(-1.3396027347034,-1.,1.67458429426086));
#28101=CARTESIAN_POINT('Ctrl Pts',(-1.3396027347034,1.,1.67458429426086));
#28102=CARTESIAN_POINT('Ctrl Pts',(-1.34067485185203,-1.,1.68086176030362));
#28103=CARTESIAN_POINT('Ctrl Pts',(-1.34067485185203,1.,1.68086176030362));
#28104=CARTESIAN_POINT('Ctrl Pts',(-1.341710374848,-1.,1.68715660868764));
#28105=CARTESIAN_POINT('Ctrl Pts',(-1.341710374848,1.,1.68715660868764));
#28106=CARTESIAN_POINT('Ctrl Pts',(-1.34270948206319,-1.,1.6934684849687));
#28107=CARTESIAN_POINT('Ctrl Pts',(-1.34270948206319,1.,1.6934684849687));
#28108=CARTESIAN_POINT('Ctrl Pts',(-1.34367237124483,-1.,1.69979707754427));
#28109=CARTESIAN_POINT('Ctrl Pts',(-1.34367237124483,1.,1.69979707754427));
#28110=CARTESIAN_POINT('Ctrl Pts',(-1.34459924533831,-1.,1.70614212266738));
#28111=CARTESIAN_POINT('Ctrl Pts',(-1.34459924533831,1.,1.70614212266738));
#28112=CARTESIAN_POINT('Ctrl Pts',(-1.34549029589416,-1.,1.71250340686822));
#28113=CARTESIAN_POINT('Ctrl Pts',(-1.34549029589416,1.,1.71250340686822));
#28114=CARTESIAN_POINT('Ctrl Pts',(-1.34634568653227,-1.,1.7188807715049));
#28115=CARTESIAN_POINT('Ctrl Pts',(-1.34634568653227,1.,1.7188807715049));
#28116=CARTESIAN_POINT('Ctrl Pts',(-1.34716554819527,-1.,1.72527410680674));
#28117=CARTESIAN_POINT('Ctrl Pts',(-1.34716554819527,1.,1.72527410680674));
#28118=CARTESIAN_POINT('Ctrl Pts',(-1.34779309152035,-1.,1.7304014965394));
#28119=CARTESIAN_POINT('Ctrl Pts',(-1.34779309152035,1.,1.7304014965394));
#28120=CARTESIAN_POINT('Ctrl Pts',(-1.34824783112887,-1.,1.73425417885907));
#28121=CARTESIAN_POINT('Ctrl Pts',(-1.34824783112887,1.,1.73425417885907));
#28122=CARTESIAN_POINT('Ctrl Pts',(-1.34854391898045,-1.,1.73682580585691));
#28123=CARTESIAN_POINT('Ctrl Pts',(-1.34854391898045,1.,1.73682580585691));
#28124=CARTESIAN_POINT('Ctrl Pts',(-1.34869019493419,-1.,1.73811241238545));
#28125=CARTESIAN_POINT('Ctrl Pts',(-1.34869019493419,1.,1.73811241238545));
#28126=CARTESIAN_POINT('',(-1.15624053661742,1.,1.31362392696032));
#28127=CARTESIAN_POINT('Ctrl Pts',(-1.15624053661742,1.,1.31362392696032));
#28128=CARTESIAN_POINT('Ctrl Pts',(-1.15950888730809,1.,1.31722977216397));
#28129=CARTESIAN_POINT('Ctrl Pts',(-1.16589330093588,1.,1.32428080721772));
#28130=CARTESIAN_POINT('Ctrl Pts',(-1.17501305789857,1.,1.33437539347008));
#28131=CARTESIAN_POINT('Ctrl Pts',(-1.18625865667441,1.,1.34687054001093));
#28132=CARTESIAN_POINT('Ctrl Pts',(-1.1987959077932,1.,1.36088705043885));
#28133=CARTESIAN_POINT('Ctrl Pts',(-1.20982812925645,1.,1.37331915607905));
#28134=CARTESIAN_POINT('Ctrl Pts',(-1.21938737280852,1.,1.38420564527715));
#28135=CARTESIAN_POINT('Ctrl Pts',(-1.22752961899387,1.,1.39361389568796));
#28136=CARTESIAN_POINT('Ctrl Pts',(-1.23434087290423,1.,1.40164708206106));
#28137=CARTESIAN_POINT('Ctrl Pts',(-1.23994455029534,1.,1.40845295531283));
#28138=CARTESIAN_POINT('Ctrl Pts',(-1.24450600513056,1.,1.41422913175179));
#28139=CARTESIAN_POINT('Ctrl Pts',(-1.24824430986571,1.,1.41923722596025));
#28140=CARTESIAN_POINT('Ctrl Pts',(-1.2514145557001,1.,1.42378102115575));
#28141=CARTESIAN_POINT('Ctrl Pts',(-1.25426945222639,1.,1.42815938799387));
#28142=CARTESIAN_POINT('Ctrl Pts',(-1.25702687965755,1.,1.43262645609691));
#28143=CARTESIAN_POINT('Ctrl Pts',(-1.25983531012005,1.,1.43734919180848));
#28144=CARTESIAN_POINT('Ctrl Pts',(-1.26273903323859,1.,1.44236470511303));
#28145=CARTESIAN_POINT('Ctrl Pts',(-1.26570925118868,1.,1.44761985001662));
#28146=CARTESIAN_POINT('Ctrl Pts',(-1.2686778680489,1.,1.45301422764247));
#28147=CARTESIAN_POINT('Ctrl Pts',(-1.27156805265289,1.,1.45843906294697));
#28148=CARTESIAN_POINT('Ctrl Pts',(-1.27433119897822,1.,1.46382431332476));
#28149=CARTESIAN_POINT('Ctrl Pts',(-1.27696414831089,1.,1.46916035917133));
#28150=CARTESIAN_POINT('Ctrl Pts',(-1.2794891824849,1.,1.4744717526707));
#28151=CARTESIAN_POINT('Ctrl Pts',(-1.28194158939517,1.,1.47980070347095));
#28152=CARTESIAN_POINT('Ctrl Pts',(-1.28435533880201,1.,1.4851881711891));
#28153=CARTESIAN_POINT('Ctrl Pts',(-1.2867467611644,1.,1.4906522831278));
#28154=CARTESIAN_POINT('Ctrl Pts',(-1.28911506584254,1.,1.49618896881754));
#28155=CARTESIAN_POINT('Ctrl Pts',(-1.29145022885181,1.,1.50178230149776));
#28156=CARTESIAN_POINT('Ctrl Pts',(-1.29373841372842,1.,1.50741159078365));
#28157=CARTESIAN_POINT('Ctrl Pts',(-1.29596850710509,1.,1.51305994241402));
#28158=CARTESIAN_POINT('Ctrl Pts',(-1.29813791800747,1.,1.51872184912724));
#28159=CARTESIAN_POINT('Ctrl Pts',(-1.30024984366328,1.,1.52439957861062));
#28160=CARTESIAN_POINT('Ctrl Pts',(-1.30231064395568,1.,1.53009970283891));
#28161=CARTESIAN_POINT('Ctrl Pts',(-1.30432735639489,1.,1.53582981268977));
#28162=CARTESIAN_POINT('Ctrl Pts',(-1.30630475189556,1.,1.54159462645432));
#28163=CARTESIAN_POINT('Ctrl Pts',(-1.30824393907473,1.,1.54739413957185));
#28164=CARTESIAN_POINT('Ctrl Pts',(-1.31014393684222,1.,1.55322568759481));
#28165=CARTESIAN_POINT('Ctrl Pts',(-1.31200264341696,1.,1.55908521254821));
#28166=CARTESIAN_POINT('Ctrl Pts',(-1.31381795281002,1.,1.56496872402353));
#28167=CARTESIAN_POINT('Ctrl Pts',(-1.31558903860016,1.,1.57087397835723));
#28168=CARTESIAN_POINT('Ctrl Pts',(-1.31731642317187,1.,1.5768005650559));
#28169=CARTESIAN_POINT('Ctrl Pts',(-1.31900135021432,1.,1.58274907898834));
#28170=CARTESIAN_POINT('Ctrl Pts',(-1.32064537110892,1.,1.58872057258245));
#28171=CARTESIAN_POINT('Ctrl Pts',(-1.32224985747682,1.,1.59471591079403));
#28172=CARTESIAN_POINT('Ctrl Pts',(-1.32381550858256,1.,1.60073511858687));
#28173=CARTESIAN_POINT('Ctrl Pts',(-1.32534250785782,1.,1.60677758290954));
#28174=CARTESIAN_POINT('Ctrl Pts',(-1.32683074483356,1.,1.6128423401575));
#28175=CARTESIAN_POINT('Ctrl Pts',(-1.32828000610449,1.,1.61892832270724));
#28176=CARTESIAN_POINT('Ctrl Pts',(-1.3296901950568,1.,1.62503464209797));
#28177=CARTESIAN_POINT('Ctrl Pts',(-1.33106149345645,1.,1.63116079730923));
#28178=CARTESIAN_POINT('Ctrl Pts',(-1.33239425103724,1.,1.63730653475089));
#28179=CARTESIAN_POINT('Ctrl Pts',(-1.33368890676572,1.,1.6434717485603));
#28180=CARTESIAN_POINT('Ctrl Pts',(-1.33494590467993,1.,1.6496563728683));
#28181=CARTESIAN_POINT('Ctrl Pts',(-1.33616559745172,1.,1.65586025952593));
#28182=CARTESIAN_POINT('Ctrl Pts',(-1.33734820885262,1.,1.66208312541983));
#28183=CARTESIAN_POINT('Ctrl Pts',(-1.33849388654388,1.,1.66832460783989));
#28184=CARTESIAN_POINT('Ctrl Pts',(-1.3396027347034,1.,1.67458429426086));
#28185=CARTESIAN_POINT('Ctrl Pts',(-1.34067485185203,1.,1.68086176030362));
#28186=CARTESIAN_POINT('Ctrl Pts',(-1.341710374848,1.,1.68715660868764));
#28187=CARTESIAN_POINT('Ctrl Pts',(-1.34270948206319,1.,1.6934684849687));
#28188=CARTESIAN_POINT('Ctrl Pts',(-1.34367237124483,1.,1.69979707754427));
#28189=CARTESIAN_POINT('Ctrl Pts',(-1.34459924533831,1.,1.70614212266738));
#28190=CARTESIAN_POINT('Ctrl Pts',(-1.34549029589416,1.,1.71250340686822));
#28191=CARTESIAN_POINT('Ctrl Pts',(-1.34634568653227,1.,1.7188807715049));
#28192=CARTESIAN_POINT('Ctrl Pts',(-1.34716554819527,1.,1.72527410680674));
#28193=CARTESIAN_POINT('Ctrl Pts',(-1.34779309152035,1.,1.7304014965394));
#28194=CARTESIAN_POINT('Ctrl Pts',(-1.34824783112887,1.,1.73425417885907));
#28195=CARTESIAN_POINT('Ctrl Pts',(-1.34854391898045,1.,1.73682580585691));
#28196=CARTESIAN_POINT('Ctrl Pts',(-1.34869019493419,1.,1.73811241238545));
#28197=CARTESIAN_POINT('',(-1.15624053661742,0.,1.31362392696032));
#28198=CARTESIAN_POINT('Origin',(0.,0.,0.));
#28199=CARTESIAN_POINT('',(-1.31362392696033,1.,1.15624053661742));
#28200=CARTESIAN_POINT('Origin',(0.,1.,0.));
#28201=CARTESIAN_POINT('',(-1.31362392696033,0.,1.15624053661742));
#28202=CARTESIAN_POINT('Ctrl Pts',(-1.73811241238545,-1.,1.34869019493419));
#28203=CARTESIAN_POINT('Ctrl Pts',(-1.73811241238545,1.,1.34869019493419));
#28204=CARTESIAN_POINT('Ctrl Pts',(-1.73682580585819,-1.,1.34854391898145));
#28205=CARTESIAN_POINT('Ctrl Pts',(-1.73682580585819,1.,1.34854391898145));
#28206=CARTESIAN_POINT('Ctrl Pts',(-1.73425417886255,-1.,1.34824783113158));
#28207=CARTESIAN_POINT('Ctrl Pts',(-1.73425417886255,1.,1.34824783113158));
#28208=CARTESIAN_POINT('Ctrl Pts',(-1.73040149654497,-1.,1.3477930915247));
#28209=CARTESIAN_POINT('Ctrl Pts',(-1.73040149654497,1.,1.3477930915247));
#28210=CARTESIAN_POINT('Ctrl Pts',(-1.72527410681298,-1.,1.34716554820013));
#28211=CARTESIAN_POINT('Ctrl Pts',(-1.72527410681298,1.,1.34716554820013));
#28212=CARTESIAN_POINT('Ctrl Pts',(-1.7188807715095,-1.,1.34634568653586));
#28213=CARTESIAN_POINT('Ctrl Pts',(-1.7188807715095,1.,1.34634568653586));
#28214=CARTESIAN_POINT('Ctrl Pts',(-1.71250340687011,-1.,1.34549029589563));
#28215=CARTESIAN_POINT('Ctrl Pts',(-1.71250340687011,1.,1.34549029589563));
#28216=CARTESIAN_POINT('Ctrl Pts',(-1.70614212266676,-1.,1.34459924533783));
#28217=CARTESIAN_POINT('Ctrl Pts',(-1.70614212266676,1.,1.34459924533783));
#28218=CARTESIAN_POINT('Ctrl Pts',(-1.69979707754221,-1.,1.34367237124322));
#28219=CARTESIAN_POINT('Ctrl Pts',(-1.69979707754221,1.,1.34367237124322));
#28220=CARTESIAN_POINT('Ctrl Pts',(-1.6934684849664,-1.,1.34270948206139));
#28221=CARTESIAN_POINT('Ctrl Pts',(-1.6934684849664,1.,1.34270948206139));
#28222=CARTESIAN_POINT('Ctrl Pts',(-1.68715660868602,-1.,1.34171037484673));
#28223=CARTESIAN_POINT('Ctrl Pts',(-1.68715660868602,1.,1.34171037484673));
#28224=CARTESIAN_POINT('Ctrl Pts',(-1.68086176030308,-1.,1.3406748518516));
#28225=CARTESIAN_POINT('Ctrl Pts',(-1.68086176030308,1.,1.3406748518516));
#28226=CARTESIAN_POINT('Ctrl Pts',(-1.67458429426126,-1.,1.33960273470372));
#28227=CARTESIAN_POINT('Ctrl Pts',(-1.67458429426126,1.,1.33960273470372));
#28228=CARTESIAN_POINT('Ctrl Pts',(-1.66832460784078,-1.,1.33849388654458));
#28229=CARTESIAN_POINT('Ctrl Pts',(-1.66832460784078,1.,1.33849388654458));
#28230=CARTESIAN_POINT('Ctrl Pts',(-1.66208312542073,-1.,1.33734820885331));
#28231=CARTESIAN_POINT('Ctrl Pts',(-1.66208312542073,1.,1.33734820885331));
#28232=CARTESIAN_POINT('Ctrl Pts',(-1.65586025952651,-1.,1.33616559745217));
#28233=CARTESIAN_POINT('Ctrl Pts',(-1.65586025952651,1.,1.33616559745217));
#28234=CARTESIAN_POINT('Ctrl Pts',(-1.64965637286843,-1.,1.33494590468003));
#28235=CARTESIAN_POINT('Ctrl Pts',(-1.64965637286843,1.,1.33494590468003));
#28236=CARTESIAN_POINT('Ctrl Pts',(-1.64347174856007,-1.,1.33368890676554));
#28237=CARTESIAN_POINT('Ctrl Pts',(-1.64347174856007,1.,1.33368890676554));
#28238=CARTESIAN_POINT('Ctrl Pts',(-1.6373065347505,-1.,1.33239425103694));
#28239=CARTESIAN_POINT('Ctrl Pts',(-1.6373065347505,1.,1.33239425103694));
#28240=CARTESIAN_POINT('Ctrl Pts',(-1.63116079730887,-1.,1.33106149345618));
#28241=CARTESIAN_POINT('Ctrl Pts',(-1.63116079730887,1.,1.33106149345618));
#28242=CARTESIAN_POINT('Ctrl Pts',(-1.62503464209777,-1.,1.32969019505665));
#28243=CARTESIAN_POINT('Ctrl Pts',(-1.62503464209777,1.,1.32969019505665));
#28244=CARTESIAN_POINT('Ctrl Pts',(-1.61892832270723,-1.,1.32828000610448));
#28245=CARTESIAN_POINT('Ctrl Pts',(-1.61892832270723,1.,1.32828000610448));
#28246=CARTESIAN_POINT('Ctrl Pts',(-1.61284234015762,-1.,1.32683074483365));
#28247=CARTESIAN_POINT('Ctrl Pts',(-1.61284234015762,1.,1.32683074483365));
#28248=CARTESIAN_POINT('Ctrl Pts',(-1.6067775829097,-1.,1.32534250785794));
#28249=CARTESIAN_POINT('Ctrl Pts',(-1.6067775829097,1.,1.32534250785794));
#28250=CARTESIAN_POINT('Ctrl Pts',(-1.600735118587,-1.,1.32381550858266));
#28251=CARTESIAN_POINT('Ctrl Pts',(-1.600735118587,1.,1.32381550858266));
#28252=CARTESIAN_POINT('Ctrl Pts',(-1.59471591079408,-1.,1.32224985747686));
#28253=CARTESIAN_POINT('Ctrl Pts',(-1.59471591079408,1.,1.32224985747686));
#28254=CARTESIAN_POINT('Ctrl Pts',(-1.58872057258244,-1.,1.32064537110891));
#28255=CARTESIAN_POINT('Ctrl Pts',(-1.58872057258244,1.,1.32064537110891));
#28256=CARTESIAN_POINT('Ctrl Pts',(-1.58274907898829,-1.,1.31900135021428));
#28257=CARTESIAN_POINT('Ctrl Pts',(-1.58274907898829,1.,1.31900135021428));
#28258=CARTESIAN_POINT('Ctrl Pts',(-1.57680056505585,-1.,1.31731642317183));
#28259=CARTESIAN_POINT('Ctrl Pts',(-1.57680056505585,1.,1.31731642317183));
#28260=CARTESIAN_POINT('Ctrl Pts',(-1.57087397835721,-1.,1.31558903860015));
#28261=CARTESIAN_POINT('Ctrl Pts',(-1.57087397835721,1.,1.31558903860015));
#28262=CARTESIAN_POINT('Ctrl Pts',(-1.56496872402352,-1.,1.31381795281002));
#28263=CARTESIAN_POINT('Ctrl Pts',(-1.56496872402352,1.,1.31381795281002));
#28264=CARTESIAN_POINT('Ctrl Pts',(-1.55908521254822,-1.,1.31200264341696));
#28265=CARTESIAN_POINT('Ctrl Pts',(-1.55908521254822,1.,1.31200264341696));
#28266=CARTESIAN_POINT('Ctrl Pts',(-1.55322568759481,-1.,1.31014393684221));
#28267=CARTESIAN_POINT('Ctrl Pts',(-1.55322568759481,1.,1.31014393684221));
#28268=CARTESIAN_POINT('Ctrl Pts',(-1.54739413957183,-1.,1.30824393907471));
#28269=CARTESIAN_POINT('Ctrl Pts',(-1.54739413957183,1.,1.30824393907471));
#28270=CARTESIAN_POINT('Ctrl Pts',(-1.54159462645428,-1.,1.30630475189553));
#28271=CARTESIAN_POINT('Ctrl Pts',(-1.54159462645428,1.,1.30630475189553));
#28272=CARTESIAN_POINT('Ctrl Pts',(-1.53582981268976,-1.,1.30432735639487));
#28273=CARTESIAN_POINT('Ctrl Pts',(-1.53582981268976,1.,1.30432735639487));
#28274=CARTESIAN_POINT('Ctrl Pts',(-1.53009970283893,-1.,1.3023106439557));
#28275=CARTESIAN_POINT('Ctrl Pts',(-1.53009970283893,1.,1.3023106439557));
#28276=CARTESIAN_POINT('Ctrl Pts',(-1.5243995786107,-1.,1.30024984366334));
#28277=CARTESIAN_POINT('Ctrl Pts',(-1.5243995786107,1.,1.30024984366334));
#28278=CARTESIAN_POINT('Ctrl Pts',(-1.51872184912735,-1.,1.29813791800757));
#28279=CARTESIAN_POINT('Ctrl Pts',(-1.51872184912735,1.,1.29813791800757));
#28280=CARTESIAN_POINT('Ctrl Pts',(-1.51305994241412,-1.,1.29596850710518));
#28281=CARTESIAN_POINT('Ctrl Pts',(-1.51305994241412,1.,1.29596850710518));
#28282=CARTESIAN_POINT('Ctrl Pts',(-1.50741159078367,-1.,1.29373841372843));
#28283=CARTESIAN_POINT('Ctrl Pts',(-1.50741159078367,1.,1.29373841372843));
#28284=CARTESIAN_POINT('Ctrl Pts',(-1.50178230149764,-1.,1.29145022885171));
#28285=CARTESIAN_POINT('Ctrl Pts',(-1.50178230149764,1.,1.29145022885171));
#28286=CARTESIAN_POINT('Ctrl Pts',(-1.49618896881729,-1.,1.28911506584232));
#28287=CARTESIAN_POINT('Ctrl Pts',(-1.49618896881729,1.,1.28911506584232));
#28288=CARTESIAN_POINT('Ctrl Pts',(-1.4906522831275,-1.,1.28674676116415));
#28289=CARTESIAN_POINT('Ctrl Pts',(-1.4906522831275,1.,1.28674676116415));
#28290=CARTESIAN_POINT('Ctrl Pts',(-1.48518817118891,-1.,1.28435533880184));
#28291=CARTESIAN_POINT('Ctrl Pts',(-1.48518817118891,1.,1.28435533880184));
#28292=CARTESIAN_POINT('Ctrl Pts',(-1.47980070347102,-1.,1.28194158939522));
#28293=CARTESIAN_POINT('Ctrl Pts',(-1.47980070347102,1.,1.28194158939522));
#28294=CARTESIAN_POINT('Ctrl Pts',(-1.4744717526711,-1.,1.27948918248524));
#28295=CARTESIAN_POINT('Ctrl Pts',(-1.4744717526711,1.,1.27948918248524));
#28296=CARTESIAN_POINT('Ctrl Pts',(-1.46916035917197,-1.,1.27696414831144));
#28297=CARTESIAN_POINT('Ctrl Pts',(-1.46916035917197,1.,1.27696414831144));
#28298=CARTESIAN_POINT('Ctrl Pts',(-1.4638243133254,-1.,1.27433119897877));
#28299=CARTESIAN_POINT('Ctrl Pts',(-1.4638243133254,1.,1.27433119897877));
#28300=CARTESIAN_POINT('Ctrl Pts',(-1.45843906294725,-1.,1.27156805265312));
#28301=CARTESIAN_POINT('Ctrl Pts',(-1.45843906294725,1.,1.27156805265312));
#28302=CARTESIAN_POINT('Ctrl Pts',(-1.45301422764205,-1.,1.26867786804854));
#28303=CARTESIAN_POINT('Ctrl Pts',(-1.45301422764205,1.,1.26867786804854));
#28304=CARTESIAN_POINT('Ctrl Pts',(-1.44761985001544,-1.,1.26570925118767));
#28305=CARTESIAN_POINT('Ctrl Pts',(-1.44761985001544,1.,1.26570925118767));
#28306=CARTESIAN_POINT('Ctrl Pts',(-1.44236470511145,-1.,1.26273903323723));
#28307=CARTESIAN_POINT('Ctrl Pts',(-1.44236470511145,1.,1.26273903323723));
#28308=CARTESIAN_POINT('Ctrl Pts',(-1.43734919180719,-1.,1.25983531011894));
#28309=CARTESIAN_POINT('Ctrl Pts',(-1.43734919180719,1.,1.25983531011894));
#28310=CARTESIAN_POINT('Ctrl Pts',(-1.43262645609679,-1.,1.25702687965744));
#28311=CARTESIAN_POINT('Ctrl Pts',(-1.43262645609679,1.,1.25702687965744));
#28312=CARTESIAN_POINT('Ctrl Pts',(-1.42815938799555,-1.,1.25426945222783));
#28313=CARTESIAN_POINT('Ctrl Pts',(-1.42815938799555,1.,1.25426945222783));
#28314=CARTESIAN_POINT('Ctrl Pts',(-1.42378102115911,-1.,1.25141455570299));
#28315=CARTESIAN_POINT('Ctrl Pts',(-1.42378102115911,1.,1.25141455570299));
#28316=CARTESIAN_POINT('Ctrl Pts',(-1.41923722596421,-1.,1.24824430986911));
#28317=CARTESIAN_POINT('Ctrl Pts',(-1.41923722596421,1.,1.24824430986911));
#28318=CARTESIAN_POINT('Ctrl Pts',(-1.41422913175437,-1.,1.24450600513278));
#28319=CARTESIAN_POINT('Ctrl Pts',(-1.41422913175437,1.,1.24450600513278));
#28320=CARTESIAN_POINT('Ctrl Pts',(-1.40845295531151,-1.,1.23994455029421));
#28321=CARTESIAN_POINT('Ctrl Pts',(-1.40845295531151,1.,1.23994455029421));
#28322=CARTESIAN_POINT('Ctrl Pts',(-1.40164708205345,-1.,1.23434087289768));
#28323=CARTESIAN_POINT('Ctrl Pts',(-1.40164708205345,1.,1.23434087289768));
#28324=CARTESIAN_POINT('Ctrl Pts',(-1.39361389567257,-1.,1.22752961898063));
#28325=CARTESIAN_POINT('Ctrl Pts',(-1.39361389567257,1.,1.22752961898063));
#28326=CARTESIAN_POINT('Ctrl Pts',(-1.38420564525391,-1.,1.21938737278853));
#28327=CARTESIAN_POINT('Ctrl Pts',(-1.38420564525391,1.,1.21938737278853));
#28328=CARTESIAN_POINT('Ctrl Pts',(-1.37331915604962,-1.,1.20982812923113));
#28329=CARTESIAN_POINT('Ctrl Pts',(-1.37331915604962,1.,1.20982812923113));
#28330=CARTESIAN_POINT('Ctrl Pts',(-1.36088705040677,-1.,1.1987959077656));
#28331=CARTESIAN_POINT('Ctrl Pts',(-1.36088705040677,1.,1.1987959077656));
#28332=CARTESIAN_POINT('Ctrl Pts',(-1.34687053998157,-1.,1.18625865664915));
#28333=CARTESIAN_POINT('Ctrl Pts',(-1.34687053998157,1.,1.18625865664915));
#28334=CARTESIAN_POINT('Ctrl Pts',(-1.33437539344842,-1.,1.17501305787994));
#28335=CARTESIAN_POINT('Ctrl Pts',(-1.33437539344842,1.,1.17501305787994));
#28336=CARTESIAN_POINT('Ctrl Pts',(-1.32428080720544,-1.,1.16589330092532));
#28337=CARTESIAN_POINT('Ctrl Pts',(-1.32428080720544,1.,1.16589330092532));
#28338=CARTESIAN_POINT('Ctrl Pts',(-1.3172297721596,-1.,1.15950888730433));
#28339=CARTESIAN_POINT('Ctrl Pts',(-1.3172297721596,1.,1.15950888730433));
#28340=CARTESIAN_POINT('Ctrl Pts',(-1.31362392696033,-1.,1.15624053661742));
#28341=CARTESIAN_POINT('Ctrl Pts',(-1.31362392696033,1.,1.15624053661742));
#28342=CARTESIAN_POINT('',(-1.73811241238545,1.,1.34869019493419));
#28343=CARTESIAN_POINT('Ctrl Pts',(-1.73811241238545,1.,1.34869019493419));
#28344=CARTESIAN_POINT('Ctrl Pts',(-1.73682580585819,1.,1.34854391898145));
#28345=CARTESIAN_POINT('Ctrl Pts',(-1.73425417886255,1.,1.34824783113158));
#28346=CARTESIAN_POINT('Ctrl Pts',(-1.73040149654497,1.,1.3477930915247));
#28347=CARTESIAN_POINT('Ctrl Pts',(-1.72527410681298,1.,1.34716554820013));
#28348=CARTESIAN_POINT('Ctrl Pts',(-1.7188807715095,1.,1.34634568653586));
#28349=CARTESIAN_POINT('Ctrl Pts',(-1.71250340687011,1.,1.34549029589563));
#28350=CARTESIAN_POINT('Ctrl Pts',(-1.70614212266676,1.,1.34459924533783));
#28351=CARTESIAN_POINT('Ctrl Pts',(-1.69979707754221,1.,1.34367237124322));
#28352=CARTESIAN_POINT('Ctrl Pts',(-1.6934684849664,1.,1.34270948206139));
#28353=CARTESIAN_POINT('Ctrl Pts',(-1.68715660868602,1.,1.34171037484673));
#28354=CARTESIAN_POINT('Ctrl Pts',(-1.68086176030308,1.,1.3406748518516));
#28355=CARTESIAN_POINT('Ctrl Pts',(-1.67458429426126,1.,1.33960273470372));
#28356=CARTESIAN_POINT('Ctrl Pts',(-1.66832460784078,1.,1.33849388654458));
#28357=CARTESIAN_POINT('Ctrl Pts',(-1.66208312542073,1.,1.33734820885331));
#28358=CARTESIAN_POINT('Ctrl Pts',(-1.65586025952651,1.,1.33616559745217));
#28359=CARTESIAN_POINT('Ctrl Pts',(-1.64965637286843,1.,1.33494590468003));
#28360=CARTESIAN_POINT('Ctrl Pts',(-1.64347174856007,1.,1.33368890676554));
#28361=CARTESIAN_POINT('Ctrl Pts',(-1.6373065347505,1.,1.33239425103694));
#28362=CARTESIAN_POINT('Ctrl Pts',(-1.63116079730887,1.,1.33106149345618));
#28363=CARTESIAN_POINT('Ctrl Pts',(-1.62503464209777,1.,1.32969019505665));
#28364=CARTESIAN_POINT('Ctrl Pts',(-1.61892832270723,1.,1.32828000610448));
#28365=CARTESIAN_POINT('Ctrl Pts',(-1.61284234015762,1.,1.32683074483365));
#28366=CARTESIAN_POINT('Ctrl Pts',(-1.6067775829097,1.,1.32534250785794));
#28367=CARTESIAN_POINT('Ctrl Pts',(-1.600735118587,1.,1.32381550858266));
#28368=CARTESIAN_POINT('Ctrl Pts',(-1.59471591079408,1.,1.32224985747686));
#28369=CARTESIAN_POINT('Ctrl Pts',(-1.58872057258244,1.,1.32064537110891));
#28370=CARTESIAN_POINT('Ctrl Pts',(-1.58274907898829,1.,1.31900135021428));
#28371=CARTESIAN_POINT('Ctrl Pts',(-1.57680056505585,1.,1.31731642317183));
#28372=CARTESIAN_POINT('Ctrl Pts',(-1.57087397835721,1.,1.31558903860015));
#28373=CARTESIAN_POINT('Ctrl Pts',(-1.56496872402352,1.,1.31381795281002));
#28374=CARTESIAN_POINT('Ctrl Pts',(-1.55908521254822,1.,1.31200264341696));
#28375=CARTESIAN_POINT('Ctrl Pts',(-1.55322568759481,1.,1.31014393684221));
#28376=CARTESIAN_POINT('Ctrl Pts',(-1.54739413957183,1.,1.30824393907471));
#28377=CARTESIAN_POINT('Ctrl Pts',(-1.54159462645428,1.,1.30630475189553));
#28378=CARTESIAN_POINT('Ctrl Pts',(-1.53582981268976,1.,1.30432735639487));
#28379=CARTESIAN_POINT('Ctrl Pts',(-1.53009970283893,1.,1.3023106439557));
#28380=CARTESIAN_POINT('Ctrl Pts',(-1.5243995786107,1.,1.30024984366334));
#28381=CARTESIAN_POINT('Ctrl Pts',(-1.51872184912735,1.,1.29813791800757));
#28382=CARTESIAN_POINT('Ctrl Pts',(-1.51305994241412,1.,1.29596850710518));
#28383=CARTESIAN_POINT('Ctrl Pts',(-1.50741159078367,1.,1.29373841372843));
#28384=CARTESIAN_POINT('Ctrl Pts',(-1.50178230149764,1.,1.29145022885171));
#28385=CARTESIAN_POINT('Ctrl Pts',(-1.49618896881729,1.,1.28911506584232));
#28386=CARTESIAN_POINT('Ctrl Pts',(-1.4906522831275,1.,1.28674676116415));
#28387=CARTESIAN_POINT('Ctrl Pts',(-1.48518817118891,1.,1.28435533880184));
#28388=CARTESIAN_POINT('Ctrl Pts',(-1.47980070347102,1.,1.28194158939522));
#28389=CARTESIAN_POINT('Ctrl Pts',(-1.4744717526711,1.,1.27948918248524));
#28390=CARTESIAN_POINT('Ctrl Pts',(-1.46916035917197,1.,1.27696414831144));
#28391=CARTESIAN_POINT('Ctrl Pts',(-1.4638243133254,1.,1.27433119897877));
#28392=CARTESIAN_POINT('Ctrl Pts',(-1.45843906294725,1.,1.27156805265312));
#28393=CARTESIAN_POINT('Ctrl Pts',(-1.45301422764205,1.,1.26867786804854));
#28394=CARTESIAN_POINT('Ctrl Pts',(-1.44761985001544,1.,1.26570925118767));
#28395=CARTESIAN_POINT('Ctrl Pts',(-1.44236470511145,1.,1.26273903323723));
#28396=CARTESIAN_POINT('Ctrl Pts',(-1.43734919180719,1.,1.25983531011894));
#28397=CARTESIAN_POINT('Ctrl Pts',(-1.43262645609679,1.,1.25702687965744));
#28398=CARTESIAN_POINT('Ctrl Pts',(-1.42815938799555,1.,1.25426945222783));
#28399=CARTESIAN_POINT('Ctrl Pts',(-1.42378102115911,1.,1.25141455570299));
#28400=CARTESIAN_POINT('Ctrl Pts',(-1.41923722596421,1.,1.24824430986911));
#28401=CARTESIAN_POINT('Ctrl Pts',(-1.41422913175437,1.,1.24450600513278));
#28402=CARTESIAN_POINT('Ctrl Pts',(-1.40845295531151,1.,1.23994455029421));
#28403=CARTESIAN_POINT('Ctrl Pts',(-1.40164708205345,1.,1.23434087289768));
#28404=CARTESIAN_POINT('Ctrl Pts',(-1.39361389567257,1.,1.22752961898063));
#28405=CARTESIAN_POINT('Ctrl Pts',(-1.38420564525391,1.,1.21938737278853));
#28406=CARTESIAN_POINT('Ctrl Pts',(-1.37331915604962,1.,1.20982812923113));
#28407=CARTESIAN_POINT('Ctrl Pts',(-1.36088705040677,1.,1.1987959077656));
#28408=CARTESIAN_POINT('Ctrl Pts',(-1.34687053998157,1.,1.18625865664915));
#28409=CARTESIAN_POINT('Ctrl Pts',(-1.33437539344842,1.,1.17501305787994));
#28410=CARTESIAN_POINT('Ctrl Pts',(-1.32428080720544,1.,1.16589330092532));
#28411=CARTESIAN_POINT('Ctrl Pts',(-1.3172297721596,1.,1.15950888730433));
#28412=CARTESIAN_POINT('Ctrl Pts',(-1.31362392696033,1.,1.15624053661742));
#28413=CARTESIAN_POINT('',(-1.73811241238545,0.,1.34869019493419));
#28414=CARTESIAN_POINT('Origin',(-1.81978687191668,0.,1.23627494547115));
#28415=CARTESIAN_POINT('',(-1.81978687191668,1.,1.23627494547115));
#28416=CARTESIAN_POINT('',(-1.73811241238545,1.,1.34869019493419));
#28417=CARTESIAN_POINT('',(-1.81978687191668,0.,1.23627494547115));
#28418=CARTESIAN_POINT('Ctrl Pts',(-1.5055822144029,-1.,0.892032620296855));
#28419=CARTESIAN_POINT('Ctrl Pts',(-1.5055822144029,1.,0.892032620296855));
#28420=CARTESIAN_POINT('Ctrl Pts',(-1.50980486807181,-1.,0.894452006967538));
#28421=CARTESIAN_POINT('Ctrl Pts',(-1.50980486807181,1.,0.894452006967538));
#28422=CARTESIAN_POINT('Ctrl Pts',(-1.51805569591479,-1.,0.89918504749193));
#28423=CARTESIAN_POINT('Ctrl Pts',(-1.51805569591479,1.,0.89918504749193));
#28424=CARTESIAN_POINT('Ctrl Pts',(-1.52984849890434,-1.,0.905967409640499));
#28425=CARTESIAN_POINT('Ctrl Pts',(-1.52984849890434,1.,0.905967409640499));
#28426=CARTESIAN_POINT('Ctrl Pts',(-1.54440491152808,-1.,0.91437591904658));
#28427=CARTESIAN_POINT('Ctrl Pts',(-1.54440491152808,1.,0.91437591904658));
#28428=CARTESIAN_POINT('Ctrl Pts',(-1.56065988582509,-1.,0.923832188966322));
#28429=CARTESIAN_POINT('Ctrl Pts',(-1.56065988582509,1.,0.923832188966322));
#28430=CARTESIAN_POINT('Ctrl Pts',(-1.57499388385561,-1.,0.932246680128849));
#28431=CARTESIAN_POINT('Ctrl Pts',(-1.57499388385561,1.,0.932246680128849));
#28432=CARTESIAN_POINT('Ctrl Pts',(-1.58744937489796,-1.,0.939646377909319));
#28433=CARTESIAN_POINT('Ctrl Pts',(-1.58744937489796,1.,0.939646377909319));
#28434=CARTESIAN_POINT('Ctrl Pts',(-1.59810042045408,-1.,0.946078063325796));
#28435=CARTESIAN_POINT('Ctrl Pts',(-1.59810042045408,1.,0.946078063325796));
#28436=CARTESIAN_POINT('Ctrl Pts',(-1.60706069897794,-1.,0.951613284361248));
#28437=CARTESIAN_POINT('Ctrl Pts',(-1.60706069897794,1.,0.951613284361248));
#28438=CARTESIAN_POINT('Ctrl Pts',(-1.61449324337233,-1.,0.956354422921573));
#28439=CARTESIAN_POINT('Ctrl Pts',(-1.61449324337233,1.,0.956354422921573));
#28440=CARTESIAN_POINT('Ctrl Pts',(-1.62061638139929,-1.,0.960438326099958));
#28441=CARTESIAN_POINT('Ctrl Pts',(-1.62061638139929,1.,0.960438326099958));
#28442=CARTESIAN_POINT('Ctrl Pts',(-1.6257193066974,-1.,0.964046107037821));
#28443=CARTESIAN_POINT('Ctrl Pts',(-1.6257193066974,1.,0.964046107037821));
#28444=CARTESIAN_POINT('Ctrl Pts',(-1.63013849959083,-1.,0.967387853228041));
#28445=CARTESIAN_POINT('Ctrl Pts',(-1.63013849959083,1.,0.967387853228041));
#28446=CARTESIAN_POINT('Ctrl Pts',(-1.63420665729609,-1.,0.970669715996356));
#28447=CARTESIAN_POINT('Ctrl Pts',(-1.63420665729609,1.,0.970669715996356));
#28448=CARTESIAN_POINT('Ctrl Pts',(-1.63820952658157,-1.,0.974066058287501));
#28449=CARTESIAN_POINT('Ctrl Pts',(-1.63820952658157,1.,0.974066058287501));
#28450=CARTESIAN_POINT('Ctrl Pts',(-1.64233990826831,-1.,0.977689794120297));
#28451=CARTESIAN_POINT('Ctrl Pts',(-1.64233990826831,1.,0.977689794120297));
#28452=CARTESIAN_POINT('Ctrl Pts',(-1.64665139190834,-1.,0.981562530940574));
#28453=CARTESIAN_POINT('Ctrl Pts',(-1.64665139190834,1.,0.981562530940574));
#28454=CARTESIAN_POINT('Ctrl Pts',(-1.6511001661277,-1.,0.985642622921626));
#28455=CARTESIAN_POINT('Ctrl Pts',(-1.6511001661277,1.,0.985642622921626));
#28456=CARTESIAN_POINT('Ctrl Pts',(-1.65559044289746,-1.,0.98985562785445));
#28457=CARTESIAN_POINT('Ctrl Pts',(-1.65559044289746,1.,0.98985562785445));
#28458=CARTESIAN_POINT('Ctrl Pts',(-1.66001553809916,-1.,0.994121836661116));
#28459=CARTESIAN_POINT('Ctrl Pts',(-1.66001553809916,1.,0.994121836661116));
#28460=CARTESIAN_POINT('Ctrl Pts',(-1.66430758030304,-1.,0.998389654952317));
#28461=CARTESIAN_POINT('Ctrl Pts',(-1.66430758030304,1.,0.998389654952317));
#28462=CARTESIAN_POINT('Ctrl Pts',(-1.66846059277231,-1.,1.00265091003682));
#28463=CARTESIAN_POINT('Ctrl Pts',(-1.66846059277231,1.,1.00265091003682));
#28464=CARTESIAN_POINT('Ctrl Pts',(-1.67250335383248,-1.,1.00692206696387));
#28465=CARTESIAN_POINT('Ctrl Pts',(-1.67250335383248,1.,1.00692206696387));
#28466=CARTESIAN_POINT('Ctrl Pts',(-1.67648246776457,-1.,1.01123236493507));
#28467=CARTESIAN_POINT('Ctrl Pts',(-1.67648246776457,1.,1.01123236493507));
#28468=CARTESIAN_POINT('Ctrl Pts',(-1.6804428989482,-1.,1.01561026162787));
#28469=CARTESIAN_POINT('Ctrl Pts',(-1.6804428989482,1.,1.01561026162787));
#28470=CARTESIAN_POINT('Ctrl Pts',(-1.68440578021739,-1.,1.02006795074222));
#28471=CARTESIAN_POINT('Ctrl Pts',(-1.68440578021739,1.,1.02006795074222));
#28472=CARTESIAN_POINT('Ctrl Pts',(-1.68836910178475,-1.,1.02460180535272));
#28473=CARTESIAN_POINT('Ctrl Pts',(-1.68836910178475,1.,1.02460180535272));
#28474=CARTESIAN_POINT('Ctrl Pts',(-1.69231840863471,-1.,1.02919977579155));
#28475=CARTESIAN_POINT('Ctrl Pts',(-1.69231840863471,1.,1.02919977579155));
#28476=CARTESIAN_POINT('Ctrl Pts',(-1.69623414782769,-1.,1.03384646003587));
#28477=CARTESIAN_POINT('Ctrl Pts',(-1.69623414782769,1.,1.03384646003587));
#28478=CARTESIAN_POINT('Ctrl Pts',(-1.70010052930951,-1.,1.03852922490782));
#28479=CARTESIAN_POINT('Ctrl Pts',(-1.70010052930951,1.,1.03852922490782));
#28480=CARTESIAN_POINT('Ctrl Pts',(-1.70391338707969,-1.,1.04324363334546));
#28481=CARTESIAN_POINT('Ctrl Pts',(-1.70391338707969,1.,1.04324363334546));
#28482=CARTESIAN_POINT('Ctrl Pts',(-1.70767646263641,-1.,1.0479908540499));
#28483=CARTESIAN_POINT('Ctrl Pts',(-1.70767646263641,1.,1.0479908540499));
#28484=CARTESIAN_POINT('Ctrl Pts',(-1.71139783543986,-1.,1.05277517202854));
#28485=CARTESIAN_POINT('Ctrl Pts',(-1.71139783543986,1.,1.05277517202854));
#28486=CARTESIAN_POINT('Ctrl Pts',(-1.71508654427022,-1.,1.05760163192481));
#28487=CARTESIAN_POINT('Ctrl Pts',(-1.71508654427022,1.,1.05760163192481));
#28488=CARTESIAN_POINT('Ctrl Pts',(-1.71874858456908,-1.,1.0624732468065));
#28489=CARTESIAN_POINT('Ctrl Pts',(-1.71874858456908,1.,1.0624732468065));
#28490=CARTESIAN_POINT('Ctrl Pts',(-1.72238500928456,-1.,1.06738966975463));
#28491=CARTESIAN_POINT('Ctrl Pts',(-1.72238500928456,1.,1.06738966975463));
#28492=CARTESIAN_POINT('Ctrl Pts',(-1.72599406198489,-1.,1.07234866990252));
#28493=CARTESIAN_POINT('Ctrl Pts',(-1.72599406198489,1.,1.07234866990252));
#28494=CARTESIAN_POINT('Ctrl Pts',(-1.72957248977424,-1.,1.0773470373727));
#28495=CARTESIAN_POINT('Ctrl Pts',(-1.72957248977424,1.,1.0773470373727));
#28496=CARTESIAN_POINT('Ctrl Pts',(-1.73311705663407,-1.,1.08238162784749));
#28497=CARTESIAN_POINT('Ctrl Pts',(-1.73311705663407,1.,1.08238162784749));
#28498=CARTESIAN_POINT('Ctrl Pts',(-1.73662628326093,-1.,1.08745056285429));
#28499=CARTESIAN_POINT('Ctrl Pts',(-1.73662628326093,1.,1.08745056285429));
#28500=CARTESIAN_POINT('Ctrl Pts',(-1.74010053962252,-1.,1.09255329056496));
#28501=CARTESIAN_POINT('Ctrl Pts',(-1.74010053962252,1.,1.09255329056496));
#28502=CARTESIAN_POINT('Ctrl Pts',(-1.74354119236212,-1.,1.09768999241229));
#28503=CARTESIAN_POINT('Ctrl Pts',(-1.74354119236212,1.,1.09768999241229));
#28504=CARTESIAN_POINT('Ctrl Pts',(-1.74695004214924,-1.,1.10286118991144));
#28505=CARTESIAN_POINT('Ctrl Pts',(-1.74695004214924,1.,1.10286118991144));
#28506=CARTESIAN_POINT('Ctrl Pts',(-1.75032866075914,-1.,1.10806728183003));
#28507=CARTESIAN_POINT('Ctrl Pts',(-1.75032866075914,1.,1.10806728183003));
#28508=CARTESIAN_POINT('Ctrl Pts',(-1.75367772094617,-1.,1.11330807582542));
#28509=CARTESIAN_POINT('Ctrl Pts',(-1.75367772094617,1.,1.11330807582542));
#28510=CARTESIAN_POINT('Ctrl Pts',(-1.75699720772089,-1.,1.11858293216752));
#28511=CARTESIAN_POINT('Ctrl Pts',(-1.75699720772089,1.,1.11858293216752));
#28512=CARTESIAN_POINT('Ctrl Pts',(-1.76028671825084,-1.,1.12389096855078));
#28513=CARTESIAN_POINT('Ctrl Pts',(-1.76028671825084,1.,1.12389096855078));
#28514=CARTESIAN_POINT('Ctrl Pts',(-1.76354571966171,-1.,1.12923123555076));
#28515=CARTESIAN_POINT('Ctrl Pts',(-1.76354571966171,1.,1.12923123555076));
#28516=CARTESIAN_POINT('Ctrl Pts',(-1.76677384551883,-1.,1.13460291804635));
#28517=CARTESIAN_POINT('Ctrl Pts',(-1.76677384551883,1.,1.13460291804635));
#28518=CARTESIAN_POINT('Ctrl Pts',(-1.76997111386806,-1.,1.14000548337));
#28519=CARTESIAN_POINT('Ctrl Pts',(-1.76997111386806,1.,1.14000548337));
#28520=CARTESIAN_POINT('Ctrl Pts',(-1.77313777896234,-1.,1.14543858226948));
#28521=CARTESIAN_POINT('Ctrl Pts',(-1.77313777896234,1.,1.14543858226948));
#28522=CARTESIAN_POINT('Ctrl Pts',(-1.77627422557034,-1.,1.15090197841531));
#28523=CARTESIAN_POINT('Ctrl Pts',(-1.77627422557034,1.,1.15090197841531));
#28524=CARTESIAN_POINT('Ctrl Pts',(-1.77938085564261,-1.,1.15639547194689));
#28525=CARTESIAN_POINT('Ctrl Pts',(-1.77938085564261,1.,1.15639547194689));
#28526=CARTESIAN_POINT('Ctrl Pts',(-1.78245795880949,-1.,1.16191881298458));
#28527=CARTESIAN_POINT('Ctrl Pts',(-1.78245795880949,1.,1.16191881298458));
#28528=CARTESIAN_POINT('Ctrl Pts',(-1.78550566040349,-1.,1.16747166312239));
#28529=CARTESIAN_POINT('Ctrl Pts',(-1.78550566040349,1.,1.16747166312239));
#28530=CARTESIAN_POINT('Ctrl Pts',(-1.78852398877523,-1.,1.17305363177265));
#28531=CARTESIAN_POINT('Ctrl Pts',(-1.78852398877523,1.,1.17305363177265));
#28532=CARTESIAN_POINT('Ctrl Pts',(-1.79151291552646,-1.,1.17866429440781));
#28533=CARTESIAN_POINT('Ctrl Pts',(-1.79151291552646,1.,1.17866429440781));
#28534=CARTESIAN_POINT('Ctrl Pts',(-1.79447240321572,-1.,1.18430321697471));
#28535=CARTESIAN_POINT('Ctrl Pts',(-1.79447240321572,1.,1.18430321697471));
#28536=CARTESIAN_POINT('Ctrl Pts',(-1.79740245923649,-1.,1.1899699793456));
#28537=CARTESIAN_POINT('Ctrl Pts',(-1.79740245923649,1.,1.1899699793456));
#28538=CARTESIAN_POINT('Ctrl Pts',(-1.80030314370121,-1.,1.19566418930405));
#28539=CARTESIAN_POINT('Ctrl Pts',(-1.80030314370121,1.,1.19566418930405));
#28540=CARTESIAN_POINT('Ctrl Pts',(-1.8031745483882,-1.,1.2013854893912));
#28541=CARTESIAN_POINT('Ctrl Pts',(-1.8031745483882,1.,1.2013854893912));
#28542=CARTESIAN_POINT('Ctrl Pts',(-1.80601678480772,-1.,1.20713356605519));
#28543=CARTESIAN_POINT('Ctrl Pts',(-1.80601678480772,1.,1.20713356605519));
#28544=CARTESIAN_POINT('Ctrl Pts',(-1.80882996916931,-1.,1.2129081570818));
#28545=CARTESIAN_POINT('Ctrl Pts',(-1.80882996916931,1.,1.2129081570818));
#28546=CARTESIAN_POINT('Ctrl Pts',(-1.81161420806172,-1.,1.2187090610323));
#28547=CARTESIAN_POINT('Ctrl Pts',(-1.81161420806172,1.,1.2187090610323));
#28548=CARTESIAN_POINT('Ctrl Pts',(-1.81436959209778,-1.,1.22453613304507));
#28549=CARTESIAN_POINT('Ctrl Pts',(-1.81436959209778,1.,1.22453613304507));
#28550=CARTESIAN_POINT('Ctrl Pts',(-1.81655087183054,-1.,1.22921864890975));
#28551=CARTESIAN_POINT('Ctrl Pts',(-1.81655087183054,1.,1.22921864890975));
#28552=CARTESIAN_POINT('Ctrl Pts',(-1.81817389920914,-1.,1.23274224526804));
#28553=CARTESIAN_POINT('Ctrl Pts',(-1.81817389920914,1.,1.23274224526804));
#28554=CARTESIAN_POINT('Ctrl Pts',(-1.81925017193531,-1.,1.23509651170384));
#28555=CARTESIAN_POINT('Ctrl Pts',(-1.81925017193531,1.,1.23509651170384));
#28556=CARTESIAN_POINT('Ctrl Pts',(-1.81978687191668,-1.,1.23627494547115));
#28557=CARTESIAN_POINT('Ctrl Pts',(-1.81978687191668,1.,1.23627494547115));
#28558=CARTESIAN_POINT('',(-1.5055822144029,1.,0.892032620296855));
#28559=CARTESIAN_POINT('Ctrl Pts',(-1.5055822144029,1.,0.892032620296855));
#28560=CARTESIAN_POINT('Ctrl Pts',(-1.50980486807181,1.,0.894452006967538));
#28561=CARTESIAN_POINT('Ctrl Pts',(-1.51805569591479,1.,0.89918504749193));
#28562=CARTESIAN_POINT('Ctrl Pts',(-1.52984849890434,1.,0.905967409640499));
#28563=CARTESIAN_POINT('Ctrl Pts',(-1.54440491152808,1.,0.91437591904658));
#28564=CARTESIAN_POINT('Ctrl Pts',(-1.56065988582509,1.,0.923832188966322));
#28565=CARTESIAN_POINT('Ctrl Pts',(-1.57499388385561,1.,0.932246680128849));
#28566=CARTESIAN_POINT('Ctrl Pts',(-1.58744937489796,1.,0.939646377909319));
#28567=CARTESIAN_POINT('Ctrl Pts',(-1.59810042045408,1.,0.946078063325796));
#28568=CARTESIAN_POINT('Ctrl Pts',(-1.60706069897794,1.,0.951613284361248));
#28569=CARTESIAN_POINT('Ctrl Pts',(-1.61449324337233,1.,0.956354422921573));
#28570=CARTESIAN_POINT('Ctrl Pts',(-1.62061638139929,1.,0.960438326099958));
#28571=CARTESIAN_POINT('Ctrl Pts',(-1.6257193066974,1.,0.964046107037821));
#28572=CARTESIAN_POINT('Ctrl Pts',(-1.63013849959083,1.,0.967387853228041));
#28573=CARTESIAN_POINT('Ctrl Pts',(-1.63420665729609,1.,0.970669715996356));
#28574=CARTESIAN_POINT('Ctrl Pts',(-1.63820952658157,1.,0.974066058287501));
#28575=CARTESIAN_POINT('Ctrl Pts',(-1.64233990826831,1.,0.977689794120297));
#28576=CARTESIAN_POINT('Ctrl Pts',(-1.64665139190834,1.,0.981562530940574));
#28577=CARTESIAN_POINT('Ctrl Pts',(-1.6511001661277,1.,0.985642622921626));
#28578=CARTESIAN_POINT('Ctrl Pts',(-1.65559044289746,1.,0.98985562785445));
#28579=CARTESIAN_POINT('Ctrl Pts',(-1.66001553809916,1.,0.994121836661116));
#28580=CARTESIAN_POINT('Ctrl Pts',(-1.66430758030304,1.,0.998389654952317));
#28581=CARTESIAN_POINT('Ctrl Pts',(-1.66846059277231,1.,1.00265091003682));
#28582=CARTESIAN_POINT('Ctrl Pts',(-1.67250335383248,1.,1.00692206696387));
#28583=CARTESIAN_POINT('Ctrl Pts',(-1.67648246776457,1.,1.01123236493507));
#28584=CARTESIAN_POINT('Ctrl Pts',(-1.6804428989482,1.,1.01561026162787));
#28585=CARTESIAN_POINT('Ctrl Pts',(-1.68440578021739,1.,1.02006795074222));
#28586=CARTESIAN_POINT('Ctrl Pts',(-1.68836910178475,1.,1.02460180535272));
#28587=CARTESIAN_POINT('Ctrl Pts',(-1.69231840863471,1.,1.02919977579155));
#28588=CARTESIAN_POINT('Ctrl Pts',(-1.69623414782769,1.,1.03384646003587));
#28589=CARTESIAN_POINT('Ctrl Pts',(-1.70010052930951,1.,1.03852922490782));
#28590=CARTESIAN_POINT('Ctrl Pts',(-1.70391338707969,1.,1.04324363334546));
#28591=CARTESIAN_POINT('Ctrl Pts',(-1.70767646263641,1.,1.0479908540499));
#28592=CARTESIAN_POINT('Ctrl Pts',(-1.71139783543986,1.,1.05277517202854));
#28593=CARTESIAN_POINT('Ctrl Pts',(-1.71508654427022,1.,1.05760163192481));
#28594=CARTESIAN_POINT('Ctrl Pts',(-1.71874858456908,1.,1.0624732468065));
#28595=CARTESIAN_POINT('Ctrl Pts',(-1.72238500928456,1.,1.06738966975463));
#28596=CARTESIAN_POINT('Ctrl Pts',(-1.72599406198489,1.,1.07234866990252));
#28597=CARTESIAN_POINT('Ctrl Pts',(-1.72957248977424,1.,1.0773470373727));
#28598=CARTESIAN_POINT('Ctrl Pts',(-1.73311705663407,1.,1.08238162784749));
#28599=CARTESIAN_POINT('Ctrl Pts',(-1.73662628326093,1.,1.08745056285429));
#28600=CARTESIAN_POINT('Ctrl Pts',(-1.74010053962252,1.,1.09255329056496));
#28601=CARTESIAN_POINT('Ctrl Pts',(-1.74354119236212,1.,1.09768999241229));
#28602=CARTESIAN_POINT('Ctrl Pts',(-1.74695004214924,1.,1.10286118991144));
#28603=CARTESIAN_POINT('Ctrl Pts',(-1.75032866075914,1.,1.10806728183003));
#28604=CARTESIAN_POINT('Ctrl Pts',(-1.75367772094617,1.,1.11330807582542));
#28605=CARTESIAN_POINT('Ctrl Pts',(-1.75699720772089,1.,1.11858293216752));
#28606=CARTESIAN_POINT('Ctrl Pts',(-1.76028671825084,1.,1.12389096855078));
#28607=CARTESIAN_POINT('Ctrl Pts',(-1.76354571966171,1.,1.12923123555076));
#28608=CARTESIAN_POINT('Ctrl Pts',(-1.76677384551883,1.,1.13460291804635));
#28609=CARTESIAN_POINT('Ctrl Pts',(-1.76997111386806,1.,1.14000548337));
#28610=CARTESIAN_POINT('Ctrl Pts',(-1.77313777896234,1.,1.14543858226948));
#28611=CARTESIAN_POINT('Ctrl Pts',(-1.77627422557034,1.,1.15090197841531));
#28612=CARTESIAN_POINT('Ctrl Pts',(-1.77938085564261,1.,1.15639547194689));
#28613=CARTESIAN_POINT('Ctrl Pts',(-1.78245795880949,1.,1.16191881298458));
#28614=CARTESIAN_POINT('Ctrl Pts',(-1.78550566040349,1.,1.16747166312239));
#28615=CARTESIAN_POINT('Ctrl Pts',(-1.78852398877523,1.,1.17305363177265));
#28616=CARTESIAN_POINT('Ctrl Pts',(-1.79151291552646,1.,1.17866429440781));
#28617=CARTESIAN_POINT('Ctrl Pts',(-1.79447240321572,1.,1.18430321697471));
#28618=CARTESIAN_POINT('Ctrl Pts',(-1.79740245923649,1.,1.1899699793456));
#28619=CARTESIAN_POINT('Ctrl Pts',(-1.80030314370121,1.,1.19566418930405));
#28620=CARTESIAN_POINT('Ctrl Pts',(-1.8031745483882,1.,1.2013854893912));
#28621=CARTESIAN_POINT('Ctrl Pts',(-1.80601678480772,1.,1.20713356605519));
#28622=CARTESIAN_POINT('Ctrl Pts',(-1.80882996916931,1.,1.2129081570818));
#28623=CARTESIAN_POINT('Ctrl Pts',(-1.81161420806172,1.,1.2187090610323));
#28624=CARTESIAN_POINT('Ctrl Pts',(-1.81436959209778,1.,1.22453613304507));
#28625=CARTESIAN_POINT('Ctrl Pts',(-1.81655087183054,1.,1.22921864890975));
#28626=CARTESIAN_POINT('Ctrl Pts',(-1.81817389920914,1.,1.23274224526804));
#28627=CARTESIAN_POINT('Ctrl Pts',(-1.81925017193531,1.,1.23509651170384));
#28628=CARTESIAN_POINT('Ctrl Pts',(-1.81978687191668,1.,1.23627494547115));
#28629=CARTESIAN_POINT('',(-1.5055822144029,0.,0.892032620296856));
#28630=CARTESIAN_POINT('Origin',(0.,0.,0.));
#28631=CARTESIAN_POINT('',(-1.60662857109684,1.,0.693717979106305));
#28632=CARTESIAN_POINT('Origin',(0.,1.,0.));
#28633=CARTESIAN_POINT('',(-1.60662857109684,0.,0.693717979106306));
#28634=CARTESIAN_POINT('Ctrl Pts',(-2.0698113262342,-1.,0.7455743247944));
#28635=CARTESIAN_POINT('Ctrl Pts',(-2.0698113262342,1.,0.7455743247944));
#28636=CARTESIAN_POINT('Ctrl Pts',(-2.06854248895728,-1.,0.745832791378367));
#28637=CARTESIAN_POINT('Ctrl Pts',(-2.06854248895728,1.,0.745832791378367));
#28638=CARTESIAN_POINT('Ctrl Pts',(-2.06600523016815,-1.,0.7463458715442));
#28639=CARTESIAN_POINT('Ctrl Pts',(-2.06600523016815,1.,0.7463458715442));
#28640=CARTESIAN_POINT('Ctrl Pts',(-2.06220058927826,-1.,0.747103932787919));
#28641=CARTESIAN_POINT('Ctrl Pts',(-2.06220058927826,1.,0.747103932787919));
#28642=CARTESIAN_POINT('Ctrl Pts',(-2.05713023031006,-1.,0.748091554183802));
#28643=CARTESIAN_POINT('Ctrl Pts',(-2.05713023031006,1.,0.748091554183802));
#28644=CARTESIAN_POINT('Ctrl Pts',(-2.05079645592154,-1.,0.749287468665046));
#28645=CARTESIAN_POINT('Ctrl Pts',(-2.05079645592154,1.,0.749287468665046));
#28646=CARTESIAN_POINT('Ctrl Pts',(-2.04446689147979,-1.,0.750444657875576));
#28647=CARTESIAN_POINT('Ctrl Pts',(-2.04446689147979,1.,0.750444657875576));
#28648=CARTESIAN_POINT('Ctrl Pts',(-2.03814160092099,-1.,0.751562963361115));
#28649=CARTESIAN_POINT('Ctrl Pts',(-2.03814160092099,1.,0.751562963361115));
#28650=CARTESIAN_POINT('Ctrl Pts',(-2.03182068456221,-1.,0.752642180487211));
#28651=CARTESIAN_POINT('Ctrl Pts',(-2.03182068456221,1.,0.752642180487211));
#28652=CARTESIAN_POINT('Ctrl Pts',(-2.02550428623313,-1.,0.753682061112768));
#28653=CARTESIAN_POINT('Ctrl Pts',(-2.02550428623313,1.,0.753682061112768));
#28654=CARTESIAN_POINT('Ctrl Pts',(-2.01919259405809,-1.,0.754682330722816));
#28655=CARTESIAN_POINT('Ctrl Pts',(-2.01919259405809,1.,0.754682330722816));
#28656=CARTESIAN_POINT('Ctrl Pts',(-2.01288584328084,-1.,0.755642704957865));
#28657=CARTESIAN_POINT('Ctrl Pts',(-2.01288584328084,1.,0.755642704957865));
#28658=CARTESIAN_POINT('Ctrl Pts',(-2.0065843158773,-1.,0.75656290464667));
#28659=CARTESIAN_POINT('Ctrl Pts',(-2.0065843158773,1.,0.75656290464667));
#28660=CARTESIAN_POINT('Ctrl Pts',(-2.00028834739178,-1.,0.757442676862724));
#28661=CARTESIAN_POINT('Ctrl Pts',(-2.00028834739178,1.,0.757442676862724));
#28662=CARTESIAN_POINT('Ctrl Pts',(-1.99399831098817,-1.,0.758281796766761));
#28663=CARTESIAN_POINT('Ctrl Pts',(-1.99399831098817,1.,0.758281796766761));
#28664=CARTESIAN_POINT('Ctrl Pts',(-1.98771456680874,-1.,0.759080037802488));
#28665=CARTESIAN_POINT('Ctrl Pts',(-1.98771456680874,1.,0.759080037802488));
#28666=CARTESIAN_POINT('Ctrl Pts',(-1.98143741418172,-1.,0.75983714745219));
#28667=CARTESIAN_POINT('Ctrl Pts',(-1.98143741418172,1.,0.75983714745219));
#28668=CARTESIAN_POINT('Ctrl Pts',(-1.97516705321494,-1.,0.760552825409757));
#28669=CARTESIAN_POINT('Ctrl Pts',(-1.97516705321494,1.,0.760552825409757));
#28670=CARTESIAN_POINT('Ctrl Pts',(-1.96890351582499,-1.,0.76122669048382));
#28671=CARTESIAN_POINT('Ctrl Pts',(-1.96890351582499,1.,0.76122669048382));
#28672=CARTESIAN_POINT('Ctrl Pts',(-1.96264672744186,-1.,0.761858300014423));
#28673=CARTESIAN_POINT('Ctrl Pts',(-1.96264672744186,1.,0.761858300014423));
#28674=CARTESIAN_POINT('Ctrl Pts',(-1.95639665309869,-1.,0.762447203806179));
#28675=CARTESIAN_POINT('Ctrl Pts',(-1.95639665309869,1.,0.762447203806179));
#28676=CARTESIAN_POINT('Ctrl Pts',(-1.95015342590024,-1.,0.762992990878769));
#28677=CARTESIAN_POINT('Ctrl Pts',(-1.95015342590024,1.,0.762992990878769));
#28678=CARTESIAN_POINT('Ctrl Pts',(-1.9439174661764,-1.,0.763495333538629));
#28679=CARTESIAN_POINT('Ctrl Pts',(-1.9439174661764,1.,0.763495333538629));
#28680=CARTESIAN_POINT('Ctrl Pts',(-1.93768964875886,-1.,0.763954049121458));
#28681=CARTESIAN_POINT('Ctrl Pts',(-1.93768964875886,1.,0.763954049121458));
#28682=CARTESIAN_POINT('Ctrl Pts',(-1.93147105496382,-1.,0.76436901067394));
#28683=CARTESIAN_POINT('Ctrl Pts',(-1.93147105496382,1.,0.76436901067394));
#28684=CARTESIAN_POINT('Ctrl Pts',(-1.92526263537048,-1.,0.764740025488211));
#28685=CARTESIAN_POINT('Ctrl Pts',(-1.92526263537048,1.,0.764740025488211));
#28686=CARTESIAN_POINT('Ctrl Pts',(-1.91906491634196,-1.,0.765066729667088));
#28687=CARTESIAN_POINT('Ctrl Pts',(-1.91906491634196,1.,0.765066729667088));
#28688=CARTESIAN_POINT('Ctrl Pts',(-1.91287765805169,-1.,0.765348465884722));
#28689=CARTESIAN_POINT('Ctrl Pts',(-1.91287765805169,1.,0.765348465884722));
#28690=CARTESIAN_POINT('Ctrl Pts',(-1.90669961402356,-1.,0.765584196937919));
#28691=CARTESIAN_POINT('Ctrl Pts',(-1.90669961402356,1.,0.765584196937919));
#28692=CARTESIAN_POINT('Ctrl Pts',(-1.90052930393596,-1.,0.765772772593386));
#28693=CARTESIAN_POINT('Ctrl Pts',(-1.90052930393596,1.,0.765772772593386));
#28694=CARTESIAN_POINT('Ctrl Pts',(-1.89436577771388,-1.,0.765913193856978));
#28695=CARTESIAN_POINT('Ctrl Pts',(-1.89436577771388,1.,0.765913193856978));
#28696=CARTESIAN_POINT('Ctrl Pts',(-1.88820926433409,-1.,0.766004837062091));
#28697=CARTESIAN_POINT('Ctrl Pts',(-1.88820926433409,1.,0.766004837062091));
#28698=CARTESIAN_POINT('Ctrl Pts',(-1.88206215302561,-1.,0.766047794851864));
#28699=CARTESIAN_POINT('Ctrl Pts',(-1.88206215302561,1.,0.766047794851864));
#28700=CARTESIAN_POINT('Ctrl Pts',(-1.87592888967883,-1.,0.766042837036744));
#28701=CARTESIAN_POINT('Ctrl Pts',(-1.87592888967883,1.,0.766042837036744));
#28702=CARTESIAN_POINT('Ctrl Pts',(-1.86981398314341,-1.,0.765990708546091));
#28703=CARTESIAN_POINT('Ctrl Pts',(-1.86981398314341,1.,0.765990708546091));
#28704=CARTESIAN_POINT('Ctrl Pts',(-1.86372027063312,-1.,0.765891519092547));
#28705=CARTESIAN_POINT('Ctrl Pts',(-1.86372027063312,1.,0.765891519092547));
#28706=CARTESIAN_POINT('Ctrl Pts',(-1.85764741390394,-1.,0.765744212909318));
#28707=CARTESIAN_POINT('Ctrl Pts',(-1.85764741390394,1.,0.765744212909318));
#28708=CARTESIAN_POINT('Ctrl Pts',(-1.85158945130063,-1.,0.765545710619062));
#28709=CARTESIAN_POINT('Ctrl Pts',(-1.85158945130063,1.,0.765545710619062));
#28710=CARTESIAN_POINT('Ctrl Pts',(-1.84553698875924,-1.,0.765291664862029));
#28711=CARTESIAN_POINT('Ctrl Pts',(-1.84553698875924,1.,0.765291664862029));
#28712=CARTESIAN_POINT('Ctrl Pts',(-1.83948181064835,-1.,0.764978057881737));
#28713=CARTESIAN_POINT('Ctrl Pts',(-1.83948181064835,1.,0.764978057881737));
#28714=CARTESIAN_POINT('Ctrl Pts',(-1.83342077227142,-1.,0.764602549687853));
#28715=CARTESIAN_POINT('Ctrl Pts',(-1.83342077227142,1.,0.764602549687853));
#28716=CARTESIAN_POINT('Ctrl Pts',(-1.82735991200065,-1.,0.764165902605995));
#28717=CARTESIAN_POINT('Ctrl Pts',(-1.82735991200065,1.,0.764165902605995));
#28718=CARTESIAN_POINT('Ctrl Pts',(-1.82131873145266,-1.,0.763673465462726));
#28719=CARTESIAN_POINT('Ctrl Pts',(-1.82131873145266,1.,0.763673465462726));
#28720=CARTESIAN_POINT('Ctrl Pts',(-1.8153211840553,-1.,0.763132003836634));
#28721=CARTESIAN_POINT('Ctrl Pts',(-1.8153211840553,1.,0.763132003836634));
#28722=CARTESIAN_POINT('Ctrl Pts',(-1.80938551463965,-1.,0.762546129463938));
#28723=CARTESIAN_POINT('Ctrl Pts',(-1.80938551463965,1.,0.762546129463938));
#28724=CARTESIAN_POINT('Ctrl Pts',(-1.80351583877342,-1.,0.761915336443547));
#28725=CARTESIAN_POINT('Ctrl Pts',(-1.80351583877342,1.,0.761915336443547));
#28726=CARTESIAN_POINT('Ctrl Pts',(-1.79768986997783,-1.,0.761229695230558));
#28727=CARTESIAN_POINT('Ctrl Pts',(-1.79768986997783,1.,0.761229695230558));
#28728=CARTESIAN_POINT('Ctrl Pts',(-1.7918581561088,-1.,0.760469555880749));
#28729=CARTESIAN_POINT('Ctrl Pts',(-1.7918581561088,1.,0.760469555880749));
#28730=CARTESIAN_POINT('Ctrl Pts',(-1.78596964884604,-1.,0.759614401110189));
#28731=CARTESIAN_POINT('Ctrl Pts',(-1.78596964884604,1.,0.759614401110189));
#28732=CARTESIAN_POINT('Ctrl Pts',(-1.77999411220945,-1.,0.758650626677518));
#28733=CARTESIAN_POINT('Ctrl Pts',(-1.77999411220945,1.,0.758650626677518));
#28734=CARTESIAN_POINT('Ctrl Pts',(-1.77394167108292,-1.,0.757578264077029));
#28735=CARTESIAN_POINT('Ctrl Pts',(-1.77394167108292,1.,0.757578264077029));
#28736=CARTESIAN_POINT('Ctrl Pts',(-1.76789396002998,-1.,0.75642189602781));
#28737=CARTESIAN_POINT('Ctrl Pts',(-1.76789396002998,1.,0.75642189602781));
#28738=CARTESIAN_POINT('Ctrl Pts',(-1.76197817240128,-1.,0.755220979974461));
#28739=CARTESIAN_POINT('Ctrl Pts',(-1.76197817240128,1.,0.755220979974461));
#28740=CARTESIAN_POINT('Ctrl Pts',(-1.75631083600019,-1.,0.754009254027829));
#28741=CARTESIAN_POINT('Ctrl Pts',(-1.75631083600019,1.,0.754009254027829));
#28742=CARTESIAN_POINT('Ctrl Pts',(-1.75095139468794,-1.,0.752797683531314));
#28743=CARTESIAN_POINT('Ctrl Pts',(-1.75095139468794,1.,0.752797683531314));
#28744=CARTESIAN_POINT('Ctrl Pts',(-1.74585086852502,-1.,0.751555614164482));
#28745=CARTESIAN_POINT('Ctrl Pts',(-1.74585086852502,1.,0.751555614164482));
#28746=CARTESIAN_POINT('Ctrl Pts',(-1.74080458267114,-1.,0.750193435981249));
#28747=CARTESIAN_POINT('Ctrl Pts',(-1.74080458267114,1.,0.750193435981249));
#28748=CARTESIAN_POINT('Ctrl Pts',(-1.7355035168033,-1.,0.74858246295687));
#28749=CARTESIAN_POINT('Ctrl Pts',(-1.7355035168033,1.,0.74858246295687));
#28750=CARTESIAN_POINT('Ctrl Pts',(-1.72958533647714,-1.,0.746574710097752));
#28751=CARTESIAN_POINT('Ctrl Pts',(-1.72958533647714,1.,0.746574710097752));
#28752=CARTESIAN_POINT('Ctrl Pts',(-1.72268229916769,-1.,0.744021445433093));
#28753=CARTESIAN_POINT('Ctrl Pts',(-1.72268229916769,1.,0.744021445433093));
#28754=CARTESIAN_POINT('Ctrl Pts',(-1.71447789751001,-1.,0.74079516202821));
#28755=CARTESIAN_POINT('Ctrl Pts',(-1.71447789751001,1.,0.74079516202821));
#28756=CARTESIAN_POINT('Ctrl Pts',(-1.70473309004249,-1.,0.736799665716932));
#28757=CARTESIAN_POINT('Ctrl Pts',(-1.70473309004249,1.,0.736799665716932));
#28758=CARTESIAN_POINT('Ctrl Pts',(-1.69326921972915,-1.,0.731963238685357));
#28759=CARTESIAN_POINT('Ctrl Pts',(-1.69326921972915,1.,0.731963238685357));
#28760=CARTESIAN_POINT('Ctrl Pts',(-1.67996158451922,-1.,0.726235967982445));
#28761=CARTESIAN_POINT('Ctrl Pts',(-1.67996158451922,1.,0.726235967982445));
#28762=CARTESIAN_POINT('Ctrl Pts',(-1.66472880551777,-1.,0.71958543378795));
#28763=CARTESIAN_POINT('Ctrl Pts',(-1.66472880551777,1.,0.71958543378795));
#28764=CARTESIAN_POINT('Ctrl Pts',(-1.64752408828442,-1.,0.711993139340447));
#28765=CARTESIAN_POINT('Ctrl Pts',(-1.64752408828442,1.,0.711993139340447));
#28766=CARTESIAN_POINT('Ctrl Pts',(-1.6321654166204,-1.,0.705159151977294));
#28767=CARTESIAN_POINT('Ctrl Pts',(-1.6321654166204,1.,0.705159151977294));
#28768=CARTESIAN_POINT('Ctrl Pts',(-1.61974673471117,-1.,0.699605146398837));
#28769=CARTESIAN_POINT('Ctrl Pts',(-1.61974673471117,1.,0.699605146398837));
#28770=CARTESIAN_POINT('Ctrl Pts',(-1.61106790957619,-1.,0.69571209787897));
#28771=CARTESIAN_POINT('Ctrl Pts',(-1.61106790957619,1.,0.69571209787897));
#28772=CARTESIAN_POINT('Ctrl Pts',(-1.60662857109684,-1.,0.693717979106305));
#28773=CARTESIAN_POINT('Ctrl Pts',(-1.60662857109684,1.,0.693717979106305));
#28774=CARTESIAN_POINT('',(-2.0698113262342,1.,0.7455743247944));
#28775=CARTESIAN_POINT('Ctrl Pts',(-2.0698113262342,1.,0.7455743247944));
#28776=CARTESIAN_POINT('Ctrl Pts',(-2.06854248895728,1.,0.745832791378367));
#28777=CARTESIAN_POINT('Ctrl Pts',(-2.06600523016815,1.,0.7463458715442));
#28778=CARTESIAN_POINT('Ctrl Pts',(-2.06220058927826,1.,0.747103932787919));
#28779=CARTESIAN_POINT('Ctrl Pts',(-2.05713023031006,1.,0.748091554183802));
#28780=CARTESIAN_POINT('Ctrl Pts',(-2.05079645592154,1.,0.749287468665046));
#28781=CARTESIAN_POINT('Ctrl Pts',(-2.04446689147979,1.,0.750444657875576));
#28782=CARTESIAN_POINT('Ctrl Pts',(-2.03814160092099,1.,0.751562963361115));
#28783=CARTESIAN_POINT('Ctrl Pts',(-2.03182068456221,1.,0.752642180487211));
#28784=CARTESIAN_POINT('Ctrl Pts',(-2.02550428623313,1.,0.753682061112768));
#28785=CARTESIAN_POINT('Ctrl Pts',(-2.01919259405809,1.,0.754682330722816));
#28786=CARTESIAN_POINT('Ctrl Pts',(-2.01288584328084,1.,0.755642704957865));
#28787=CARTESIAN_POINT('Ctrl Pts',(-2.0065843158773,1.,0.75656290464667));
#28788=CARTESIAN_POINT('Ctrl Pts',(-2.00028834739178,1.,0.757442676862724));
#28789=CARTESIAN_POINT('Ctrl Pts',(-1.99399831098817,1.,0.758281796766761));
#28790=CARTESIAN_POINT('Ctrl Pts',(-1.98771456680874,1.,0.759080037802488));
#28791=CARTESIAN_POINT('Ctrl Pts',(-1.98143741418172,1.,0.75983714745219));
#28792=CARTESIAN_POINT('Ctrl Pts',(-1.97516705321494,1.,0.760552825409757));
#28793=CARTESIAN_POINT('Ctrl Pts',(-1.96890351582499,1.,0.76122669048382));
#28794=CARTESIAN_POINT('Ctrl Pts',(-1.96264672744186,1.,0.761858300014423));
#28795=CARTESIAN_POINT('Ctrl Pts',(-1.95639665309869,1.,0.762447203806179));
#28796=CARTESIAN_POINT('Ctrl Pts',(-1.95015342590024,1.,0.762992990878769));
#28797=CARTESIAN_POINT('Ctrl Pts',(-1.9439174661764,1.,0.763495333538629));
#28798=CARTESIAN_POINT('Ctrl Pts',(-1.93768964875886,1.,0.763954049121458));
#28799=CARTESIAN_POINT('Ctrl Pts',(-1.93147105496382,1.,0.76436901067394));
#28800=CARTESIAN_POINT('Ctrl Pts',(-1.92526263537048,1.,0.764740025488211));
#28801=CARTESIAN_POINT('Ctrl Pts',(-1.91906491634196,1.,0.765066729667088));
#28802=CARTESIAN_POINT('Ctrl Pts',(-1.91287765805169,1.,0.765348465884722));
#28803=CARTESIAN_POINT('Ctrl Pts',(-1.90669961402356,1.,0.765584196937919));
#28804=CARTESIAN_POINT('Ctrl Pts',(-1.90052930393596,1.,0.765772772593386));
#28805=CARTESIAN_POINT('Ctrl Pts',(-1.89436577771388,1.,0.765913193856978));
#28806=CARTESIAN_POINT('Ctrl Pts',(-1.88820926433409,1.,0.766004837062091));
#28807=CARTESIAN_POINT('Ctrl Pts',(-1.88206215302561,1.,0.766047794851864));
#28808=CARTESIAN_POINT('Ctrl Pts',(-1.87592888967883,1.,0.766042837036744));
#28809=CARTESIAN_POINT('Ctrl Pts',(-1.86981398314341,1.,0.765990708546091));
#28810=CARTESIAN_POINT('Ctrl Pts',(-1.86372027063312,1.,0.765891519092547));
#28811=CARTESIAN_POINT('Ctrl Pts',(-1.85764741390394,1.,0.765744212909318));
#28812=CARTESIAN_POINT('Ctrl Pts',(-1.85158945130063,1.,0.765545710619062));
#28813=CARTESIAN_POINT('Ctrl Pts',(-1.84553698875924,1.,0.765291664862029));
#28814=CARTESIAN_POINT('Ctrl Pts',(-1.83948181064835,1.,0.764978057881737));
#28815=CARTESIAN_POINT('Ctrl Pts',(-1.83342077227142,1.,0.764602549687853));
#28816=CARTESIAN_POINT('Ctrl Pts',(-1.82735991200065,1.,0.764165902605995));
#28817=CARTESIAN_POINT('Ctrl Pts',(-1.82131873145266,1.,0.763673465462726));
#28818=CARTESIAN_POINT('Ctrl Pts',(-1.8153211840553,1.,0.763132003836634));
#28819=CARTESIAN_POINT('Ctrl Pts',(-1.80938551463965,1.,0.762546129463938));
#28820=CARTESIAN_POINT('Ctrl Pts',(-1.80351583877342,1.,0.761915336443547));
#28821=CARTESIAN_POINT('Ctrl Pts',(-1.79768986997783,1.,0.761229695230558));
#28822=CARTESIAN_POINT('Ctrl Pts',(-1.7918581561088,1.,0.760469555880749));
#28823=CARTESIAN_POINT('Ctrl Pts',(-1.78596964884604,1.,0.759614401110189));
#28824=CARTESIAN_POINT('Ctrl Pts',(-1.77999411220945,1.,0.758650626677518));
#28825=CARTESIAN_POINT('Ctrl Pts',(-1.77394167108292,1.,0.757578264077029));
#28826=CARTESIAN_POINT('Ctrl Pts',(-1.76789396002998,1.,0.75642189602781));
#28827=CARTESIAN_POINT('Ctrl Pts',(-1.76197817240128,1.,0.755220979974461));
#28828=CARTESIAN_POINT('Ctrl Pts',(-1.75631083600019,1.,0.754009254027829));
#28829=CARTESIAN_POINT('Ctrl Pts',(-1.75095139468794,1.,0.752797683531314));
#28830=CARTESIAN_POINT('Ctrl Pts',(-1.74585086852502,1.,0.751555614164482));
#28831=CARTESIAN_POINT('Ctrl Pts',(-1.74080458267114,1.,0.750193435981249));
#28832=CARTESIAN_POINT('Ctrl Pts',(-1.7355035168033,1.,0.74858246295687));
#28833=CARTESIAN_POINT('Ctrl Pts',(-1.72958533647714,1.,0.746574710097752));
#28834=CARTESIAN_POINT('Ctrl Pts',(-1.72268229916769,1.,0.744021445433093));
#28835=CARTESIAN_POINT('Ctrl Pts',(-1.71447789751001,1.,0.74079516202821));
#28836=CARTESIAN_POINT('Ctrl Pts',(-1.70473309004249,1.,0.736799665716932));
#28837=CARTESIAN_POINT('Ctrl Pts',(-1.69326921972915,1.,0.731963238685357));
#28838=CARTESIAN_POINT('Ctrl Pts',(-1.67996158451922,1.,0.726235967982445));
#28839=CARTESIAN_POINT('Ctrl Pts',(-1.66472880551777,1.,0.71958543378795));
#28840=CARTESIAN_POINT('Ctrl Pts',(-1.64752408828442,1.,0.711993139340447));
#28841=CARTESIAN_POINT('Ctrl Pts',(-1.6321654166204,1.,0.705159151977294));
#28842=CARTESIAN_POINT('Ctrl Pts',(-1.61974673471117,1.,0.699605146398837));
#28843=CARTESIAN_POINT('Ctrl Pts',(-1.61106790957619,1.,0.69571209787897));
#28844=CARTESIAN_POINT('Ctrl Pts',(-1.60662857109684,1.,0.693717979106305));
#28845=CARTESIAN_POINT('',(-2.0698113262342,0.,0.7455743247944));
#28846=CARTESIAN_POINT('Origin',(-2.11275013067528,0.,0.61342227326009));
#28847=CARTESIAN_POINT('',(-2.11275013067528,1.,0.61342227326009));
#28848=CARTESIAN_POINT('',(-2.0698113262342,1.,0.7455743247944));
#28849=CARTESIAN_POINT('',(-2.11275013067528,0.,0.61342227326009));
#28850=CARTESIAN_POINT('Ctrl Pts',(-1.7075470150345,-1.,0.383122945602004));
#28851=CARTESIAN_POINT('Ctrl Pts',(-1.7075470150345,1.,0.383122945602004));
#28852=CARTESIAN_POINT('Ctrl Pts',(-1.71231062891958,-1.,0.384119047315542));
#28853=CARTESIAN_POINT('Ctrl Pts',(-1.71231062891958,1.,0.384119047315542));
#28854=CARTESIAN_POINT('Ctrl Pts',(-1.72162022246158,-1.,0.38607079032701));
#28855=CARTESIAN_POINT('Ctrl Pts',(-1.72162022246158,1.,0.38607079032701));
#28856=CARTESIAN_POINT('Ctrl Pts',(-1.7349317097561,-1.,0.388877023509191));
#28857=CARTESIAN_POINT('Ctrl Pts',(-1.7349317097561,1.,0.388877023509191));
#28858=CARTESIAN_POINT('Ctrl Pts',(-1.75137405313962,-1.,0.392375812294307));
#28859=CARTESIAN_POINT('Ctrl Pts',(-1.75137405313962,1.,0.392375812294307));
#28860=CARTESIAN_POINT('Ctrl Pts',(-1.7697556004756,-1.,0.39634619612042));
#28861=CARTESIAN_POINT('Ctrl Pts',(-1.7697556004756,1.,0.39634619612042));
#28862=CARTESIAN_POINT('Ctrl Pts',(-1.78598826347533,-1.,0.39991940378308));
#28863=CARTESIAN_POINT('Ctrl Pts',(-1.78598826347533,1.,0.39991940378308));
#28864=CARTESIAN_POINT('Ctrl Pts',(-1.80012077176221,-1.,0.403107976170441));
#28865=CARTESIAN_POINT('Ctrl Pts',(-1.80012077176221,1.,0.403107976170441));
#28866=CARTESIAN_POINT('Ctrl Pts',(-1.81223801813988,-1.,0.405933518411838));
#28867=CARTESIAN_POINT('Ctrl Pts',(-1.81223801813988,1.,0.405933518411838));
#28868=CARTESIAN_POINT('Ctrl Pts',(-1.8224702267854,-1.,0.408428948108533));
#28869=CARTESIAN_POINT('Ctrl Pts',(-1.8224702267854,1.,0.408428948108533));
#28870=CARTESIAN_POINT('Ctrl Pts',(-1.83100408895216,-1.,0.410641256301675));
#28871=CARTESIAN_POINT('Ctrl Pts',(-1.83100408895216,1.,0.410641256301675));
#28872=CARTESIAN_POINT('Ctrl Pts',(-1.83808953475839,-1.,0.412633125322161));
#28873=CARTESIAN_POINT('Ctrl Pts',(-1.83808953475839,1.,0.412633125322161));
#28874=CARTESIAN_POINT('Ctrl Pts',(-1.8440575707371,-1.,0.41448743825434));
#28875=CARTESIAN_POINT('Ctrl Pts',(-1.8440575707371,1.,0.41448743825434));
#28876=CARTESIAN_POINT('Ctrl Pts',(-1.84929312929882,-1.,0.416300022038864));
#28877=CARTESIAN_POINT('Ctrl Pts',(-1.84929312929882,1.,0.416300022038864));
#28878=CARTESIAN_POINT('Ctrl Pts',(-1.85417632856234,-1.,0.418164129143534));
#28879=CARTESIAN_POINT('Ctrl Pts',(-1.85417632856234,1.,0.418164129143534));
#28880=CARTESIAN_POINT('Ctrl Pts',(-1.85903281096686,-1.,0.420157287975619));
#28881=CARTESIAN_POINT('Ctrl Pts',(-1.85903281096686,1.,0.420157287975619));
#28882=CARTESIAN_POINT('Ctrl Pts',(-1.86408083334028,-1.,0.422327307418275));
#28883=CARTESIAN_POINT('Ctrl Pts',(-1.86408083334028,1.,0.422327307418275));
#28884=CARTESIAN_POINT('Ctrl Pts',(-1.86937803944323,-1.,0.424678177291359));
#28885=CARTESIAN_POINT('Ctrl Pts',(-1.86937803944323,1.,0.424678177291359));
#28886=CARTESIAN_POINT('Ctrl Pts',(-1.87486989291484,-1.,0.427183828519102));
#28887=CARTESIAN_POINT('Ctrl Pts',(-1.87486989291484,1.,0.427183828519102));
#28888=CARTESIAN_POINT('Ctrl Pts',(-1.88044229001832,-1.,0.429803062482344));
#28889=CARTESIAN_POINT('Ctrl Pts',(-1.88044229001832,1.,0.429803062482344));
#28890=CARTESIAN_POINT('Ctrl Pts',(-1.88596913666793,-1.,0.432493038548748));
#28891=CARTESIAN_POINT('Ctrl Pts',(-1.88596913666793,1.,0.432493038548748));
#28892=CARTESIAN_POINT('Ctrl Pts',(-1.89136993975504,-1.,0.435225660963383));
#28893=CARTESIAN_POINT('Ctrl Pts',(-1.89136993975504,1.,0.435225660963383));
#28894=CARTESIAN_POINT('Ctrl Pts',(-1.89663648956466,-1.,0.437995003948244));
#28895=CARTESIAN_POINT('Ctrl Pts',(-1.89663648956466,1.,0.437995003948244));
#28896=CARTESIAN_POINT('Ctrl Pts',(-1.90180124389086,-1.,0.440807833704038));
#28897=CARTESIAN_POINT('Ctrl Pts',(-1.90180124389086,1.,0.440807833704038));
#28898=CARTESIAN_POINT('Ctrl Pts',(-1.90691756144898,-1.,0.44367755684915));
#28899=CARTESIAN_POINT('Ctrl Pts',(-1.90691756144898,1.,0.44367755684915));
#28900=CARTESIAN_POINT('Ctrl Pts',(-1.9120369998112,-1.,0.446617343485711));
#28901=CARTESIAN_POINT('Ctrl Pts',(-1.9120369998112,1.,0.446617343485711));
#28902=CARTESIAN_POINT('Ctrl Pts',(-1.91718342555755,-1.,0.449632260106662));
#28903=CARTESIAN_POINT('Ctrl Pts',(-1.91718342555755,1.,0.449632260106662));
#28904=CARTESIAN_POINT('Ctrl Pts',(-1.92235380648502,-1.,0.452719478359432));
#28905=CARTESIAN_POINT('Ctrl Pts',(-1.92235380648502,1.,0.452719478359432));
#28906=CARTESIAN_POINT('Ctrl Pts',(-1.92753067150476,-1.,0.455872005174371));
#28907=CARTESIAN_POINT('Ctrl Pts',(-1.92753067150476,1.,0.455872005174371));
#28908=CARTESIAN_POINT('Ctrl Pts',(-1.93269066517934,-1.,0.459081234547926));
#28909=CARTESIAN_POINT('Ctrl Pts',(-1.93269066517934,1.,0.459081234547926));
#28910=CARTESIAN_POINT('Ctrl Pts',(-1.93781486640821,-1.,0.462340031009056));
#28911=CARTESIAN_POINT('Ctrl Pts',(-1.93781486640821,1.,0.462340031009056));
#28912=CARTESIAN_POINT('Ctrl Pts',(-1.9428979419619,-1.,0.46564546202603));
#28913=CARTESIAN_POINT('Ctrl Pts',(-1.9428979419619,1.,0.46564546202603));
#28914=CARTESIAN_POINT('Ctrl Pts',(-1.94794381136514,-1.,0.468997482913135));
#28915=CARTESIAN_POINT('Ctrl Pts',(-1.94794381136514,1.,0.468997482913135));
#28916=CARTESIAN_POINT('Ctrl Pts',(-1.95296148278133,-1.,0.472397672264072));
#28917=CARTESIAN_POINT('Ctrl Pts',(-1.95296148278133,1.,0.472397672264072));
#28918=CARTESIAN_POINT('Ctrl Pts',(-1.95796111148177,-1.,0.475848034683176));
#28919=CARTESIAN_POINT('Ctrl Pts',(-1.95796111148177,1.,0.475848034683176));
#28920=CARTESIAN_POINT('Ctrl Pts',(-1.96294933055943,-1.,0.479349583074855));
#28921=CARTESIAN_POINT('Ctrl Pts',(-1.96294933055943,1.,0.479349583074855));
#28922=CARTESIAN_POINT('Ctrl Pts',(-1.96792703422362,-1.,0.48290166212069));
#28923=CARTESIAN_POINT('Ctrl Pts',(-1.96792703422362,1.,0.48290166212069));
#28924=CARTESIAN_POINT('Ctrl Pts',(-1.97289186263272,-1.,0.486502692907659));
#28925=CARTESIAN_POINT('Ctrl Pts',(-1.97289186263272,1.,0.486502692907659));
#28926=CARTESIAN_POINT('Ctrl Pts',(-1.97783973019229,-1.,0.490150627860952));
#28927=CARTESIAN_POINT('Ctrl Pts',(-1.97783973019229,1.,0.490150627860952));
#28928=CARTESIAN_POINT('Ctrl Pts',(-1.98276658761821,-1.,0.493843476541494));
#28929=CARTESIAN_POINT('Ctrl Pts',(-1.98276658761821,1.,0.493843476541494));
#28930=CARTESIAN_POINT('Ctrl Pts',(-1.98767044752932,-1.,0.497579909545574));
#28931=CARTESIAN_POINT('Ctrl Pts',(-1.98767044752932,1.,0.497579909545574));
#28932=CARTESIAN_POINT('Ctrl Pts',(-1.99255149126155,-1.,0.501359287727146));
#28933=CARTESIAN_POINT('Ctrl Pts',(-1.99255149126155,1.,0.501359287727146));
#28934=CARTESIAN_POINT('Ctrl Pts',(-1.99741107463572,-1.,0.505181361323026));
#28935=CARTESIAN_POINT('Ctrl Pts',(-1.99741107463572,1.,0.505181361323026));
#28936=CARTESIAN_POINT('Ctrl Pts',(-2.00225107134734,-1.,0.509046069886157));
#28937=CARTESIAN_POINT('Ctrl Pts',(-2.00225107134734,1.,0.509046069886157));
#28938=CARTESIAN_POINT('Ctrl Pts',(-2.00707309946949,-1.,0.512953306961792));
#28939=CARTESIAN_POINT('Ctrl Pts',(-2.00707309946949,1.,0.512953306961792));
#28940=CARTESIAN_POINT('Ctrl Pts',(-2.01187773939242,-1.,0.516902681728687));
#28941=CARTESIAN_POINT('Ctrl Pts',(-2.01187773939242,1.,0.516902681728687));
#28942=CARTESIAN_POINT('Ctrl Pts',(-2.01666477917286,-1.,0.52089359039937));
#28943=CARTESIAN_POINT('Ctrl Pts',(-2.01666477917286,1.,0.52089359039937));
#28944=CARTESIAN_POINT('Ctrl Pts',(-2.02143356304698,-1.,0.524925318333476));
#28945=CARTESIAN_POINT('Ctrl Pts',(-2.02143356304698,1.,0.524925318333476));
#28946=CARTESIAN_POINT('Ctrl Pts',(-2.0261832908329,-1.,0.528997127241914));
#28947=CARTESIAN_POINT('Ctrl Pts',(-2.0261832908329,1.,0.528997127241914));
#28948=CARTESIAN_POINT('Ctrl Pts',(-2.03091336214426,-1.,0.533108355132976));
#28949=CARTESIAN_POINT('Ctrl Pts',(-2.03091336214426,1.,0.533108355132976));
#28950=CARTESIAN_POINT('Ctrl Pts',(-2.03562362954037,-1.,0.537258489833262));
#28951=CARTESIAN_POINT('Ctrl Pts',(-2.03562362954037,1.,0.537258489833262));
#28952=CARTESIAN_POINT('Ctrl Pts',(-2.04031422690527,-1.,0.541447120615659));
#28953=CARTESIAN_POINT('Ctrl Pts',(-2.04031422690527,1.,0.541447120615659));
#28954=CARTESIAN_POINT('Ctrl Pts',(-2.04498544714588,-1.,0.54567390381743));
#28955=CARTESIAN_POINT('Ctrl Pts',(-2.04498544714588,1.,0.54567390381743));
#28956=CARTESIAN_POINT('Ctrl Pts',(-2.04963761077958,-1.,0.549938525150295));
#28957=CARTESIAN_POINT('Ctrl Pts',(-2.04963761077958,1.,0.549938525150295));
#28958=CARTESIAN_POINT('Ctrl Pts',(-2.05427091604413,-1.,0.554240657463906));
#28959=CARTESIAN_POINT('Ctrl Pts',(-2.05427091604413,1.,0.554240657463906));
#28960=CARTESIAN_POINT('Ctrl Pts',(-2.05888537756462,-1.,0.558579940185151));
#28961=CARTESIAN_POINT('Ctrl Pts',(-2.05888537756462,1.,0.558579940185151));
#28962=CARTESIAN_POINT('Ctrl Pts',(-2.06348090160589,-1.,0.562955993082261));
#28963=CARTESIAN_POINT('Ctrl Pts',(-2.06348090160589,1.,0.562955993082261));
#28964=CARTESIAN_POINT('Ctrl Pts',(-2.06805732997334,-1.,0.567368421181087));
#28965=CARTESIAN_POINT('Ctrl Pts',(-2.06805732997334,1.,0.567368421181087));
#28966=CARTESIAN_POINT('Ctrl Pts',(-2.07261449292824,-1.,0.571816823242603));
#28967=CARTESIAN_POINT('Ctrl Pts',(-2.07261449292824,1.,0.571816823242603));
#28968=CARTESIAN_POINT('Ctrl Pts',(-2.07715226767559,-1.,0.576300797416844));
#28969=CARTESIAN_POINT('Ctrl Pts',(-2.07715226767559,1.,0.576300797416844));
#28970=CARTESIAN_POINT('Ctrl Pts',(-2.08167059018418,-1.,0.580819952108063));
#28971=CARTESIAN_POINT('Ctrl Pts',(-2.08167059018418,1.,0.580819952108063));
#28972=CARTESIAN_POINT('Ctrl Pts',(-2.08616943727951,-1.,0.585373918991617));
#28973=CARTESIAN_POINT('Ctrl Pts',(-2.08616943727951,1.,0.585373918991617));
#28974=CARTESIAN_POINT('Ctrl Pts',(-2.09064881812129,-1.,0.589962365403406));
#28975=CARTESIAN_POINT('Ctrl Pts',(-2.09064881812129,1.,0.589962365403406));
#28976=CARTESIAN_POINT('Ctrl Pts',(-2.0951087622027,-1.,0.594585006052162));
#28977=CARTESIAN_POINT('Ctrl Pts',(-2.0951087622027,1.,0.594585006052162));
#28978=CARTESIAN_POINT('Ctrl Pts',(-2.0995493086477,-1.,0.599241616420533));
#28979=CARTESIAN_POINT('Ctrl Pts',(-2.0995493086477,1.,0.599241616420533));
#28980=CARTESIAN_POINT('Ctrl Pts',(-2.10397049886949,-1.,0.60393203073603));
#28981=CARTESIAN_POINT('Ctrl Pts',(-2.10397049886949,1.,0.60393203073603));
#28982=CARTESIAN_POINT('Ctrl Pts',(-2.1074919961518,-1.,0.607711315454876));
#28983=CARTESIAN_POINT('Ctrl Pts',(-2.1074919961518,1.,0.607711315454876));
#28984=CARTESIAN_POINT('Ctrl Pts',(-2.11012443807238,-1.,0.610560911689899));
#28985=CARTESIAN_POINT('Ctrl Pts',(-2.11012443807238,1.,0.610560911689899));
#28986=CARTESIAN_POINT('Ctrl Pts',(-2.11187554259986,-1.,0.6124673655618));
#28987=CARTESIAN_POINT('Ctrl Pts',(-2.11187554259986,1.,0.6124673655618));
#28988=CARTESIAN_POINT('Ctrl Pts',(-2.11275013067528,-1.,0.61342227326009));
#28989=CARTESIAN_POINT('Ctrl Pts',(-2.11275013067528,1.,0.61342227326009));
#28990=CARTESIAN_POINT('',(-1.7075470150345,1.,0.383122945602004));
#28991=CARTESIAN_POINT('Ctrl Pts',(-1.7075470150345,1.,0.383122945602004));
#28992=CARTESIAN_POINT('Ctrl Pts',(-1.71231062891958,1.,0.384119047315542));
#28993=CARTESIAN_POINT('Ctrl Pts',(-1.72162022246158,1.,0.38607079032701));
#28994=CARTESIAN_POINT('Ctrl Pts',(-1.7349317097561,1.,0.388877023509191));
#28995=CARTESIAN_POINT('Ctrl Pts',(-1.75137405313962,1.,0.392375812294307));
#28996=CARTESIAN_POINT('Ctrl Pts',(-1.7697556004756,1.,0.39634619612042));
#28997=CARTESIAN_POINT('Ctrl Pts',(-1.78598826347533,1.,0.39991940378308));
#28998=CARTESIAN_POINT('Ctrl Pts',(-1.80012077176221,1.,0.403107976170441));
#28999=CARTESIAN_POINT('Ctrl Pts',(-1.81223801813988,1.,0.405933518411838));
#29000=CARTESIAN_POINT('Ctrl Pts',(-1.8224702267854,1.,0.408428948108533));
#29001=CARTESIAN_POINT('Ctrl Pts',(-1.83100408895216,1.,0.410641256301675));
#29002=CARTESIAN_POINT('Ctrl Pts',(-1.83808953475839,1.,0.412633125322161));
#29003=CARTESIAN_POINT('Ctrl Pts',(-1.8440575707371,1.,0.41448743825434));
#29004=CARTESIAN_POINT('Ctrl Pts',(-1.84929312929882,1.,0.416300022038864));
#29005=CARTESIAN_POINT('Ctrl Pts',(-1.85417632856234,1.,0.418164129143534));
#29006=CARTESIAN_POINT('Ctrl Pts',(-1.85903281096686,1.,0.420157287975619));
#29007=CARTESIAN_POINT('Ctrl Pts',(-1.86408083334028,1.,0.422327307418275));
#29008=CARTESIAN_POINT('Ctrl Pts',(-1.86937803944323,1.,0.424678177291359));
#29009=CARTESIAN_POINT('Ctrl Pts',(-1.87486989291484,1.,0.427183828519102));
#29010=CARTESIAN_POINT('Ctrl Pts',(-1.88044229001832,1.,0.429803062482344));
#29011=CARTESIAN_POINT('Ctrl Pts',(-1.88596913666793,1.,0.432493038548748));
#29012=CARTESIAN_POINT('Ctrl Pts',(-1.89136993975504,1.,0.435225660963383));
#29013=CARTESIAN_POINT('Ctrl Pts',(-1.89663648956466,1.,0.437995003948244));
#29014=CARTESIAN_POINT('Ctrl Pts',(-1.90180124389086,1.,0.440807833704038));
#29015=CARTESIAN_POINT('Ctrl Pts',(-1.90691756144898,1.,0.44367755684915));
#29016=CARTESIAN_POINT('Ctrl Pts',(-1.9120369998112,1.,0.446617343485711));
#29017=CARTESIAN_POINT('Ctrl Pts',(-1.91718342555755,1.,0.449632260106662));
#29018=CARTESIAN_POINT('Ctrl Pts',(-1.92235380648502,1.,0.452719478359432));
#29019=CARTESIAN_POINT('Ctrl Pts',(-1.92753067150476,1.,0.455872005174371));
#29020=CARTESIAN_POINT('Ctrl Pts',(-1.93269066517934,1.,0.459081234547926));
#29021=CARTESIAN_POINT('Ctrl Pts',(-1.93781486640821,1.,0.462340031009056));
#29022=CARTESIAN_POINT('Ctrl Pts',(-1.9428979419619,1.,0.46564546202603));
#29023=CARTESIAN_POINT('Ctrl Pts',(-1.94794381136514,1.,0.468997482913135));
#29024=CARTESIAN_POINT('Ctrl Pts',(-1.95296148278133,1.,0.472397672264072));
#29025=CARTESIAN_POINT('Ctrl Pts',(-1.95796111148177,1.,0.475848034683176));
#29026=CARTESIAN_POINT('Ctrl Pts',(-1.96294933055943,1.,0.479349583074855));
#29027=CARTESIAN_POINT('Ctrl Pts',(-1.96792703422362,1.,0.48290166212069));
#29028=CARTESIAN_POINT('Ctrl Pts',(-1.97289186263272,1.,0.486502692907659));
#29029=CARTESIAN_POINT('Ctrl Pts',(-1.97783973019229,1.,0.490150627860952));
#29030=CARTESIAN_POINT('Ctrl Pts',(-1.98276658761821,1.,0.493843476541494));
#29031=CARTESIAN_POINT('Ctrl Pts',(-1.98767044752932,1.,0.497579909545574));
#29032=CARTESIAN_POINT('Ctrl Pts',(-1.99255149126155,1.,0.501359287727146));
#29033=CARTESIAN_POINT('Ctrl Pts',(-1.99741107463572,1.,0.505181361323026));
#29034=CARTESIAN_POINT('Ctrl Pts',(-2.00225107134734,1.,0.509046069886157));
#29035=CARTESIAN_POINT('Ctrl Pts',(-2.00707309946949,1.,0.512953306961792));
#29036=CARTESIAN_POINT('Ctrl Pts',(-2.01187773939242,1.,0.516902681728687));
#29037=CARTESIAN_POINT('Ctrl Pts',(-2.01666477917286,1.,0.52089359039937));
#29038=CARTESIAN_POINT('Ctrl Pts',(-2.02143356304698,1.,0.524925318333476));
#29039=CARTESIAN_POINT('Ctrl Pts',(-2.0261832908329,1.,0.528997127241914));
#29040=CARTESIAN_POINT('Ctrl Pts',(-2.03091336214426,1.,0.533108355132976));
#29041=CARTESIAN_POINT('Ctrl Pts',(-2.03562362954037,1.,0.537258489833262));
#29042=CARTESIAN_POINT('Ctrl Pts',(-2.04031422690527,1.,0.541447120615659));
#29043=CARTESIAN_POINT('Ctrl Pts',(-2.04498544714588,1.,0.54567390381743));
#29044=CARTESIAN_POINT('Ctrl Pts',(-2.04963761077958,1.,0.549938525150295));
#29045=CARTESIAN_POINT('Ctrl Pts',(-2.05427091604413,1.,0.554240657463906));
#29046=CARTESIAN_POINT('Ctrl Pts',(-2.05888537756462,1.,0.558579940185151));
#29047=CARTESIAN_POINT('Ctrl Pts',(-2.06348090160589,1.,0.562955993082261));
#29048=CARTESIAN_POINT('Ctrl Pts',(-2.06805732997334,1.,0.567368421181087));
#29049=CARTESIAN_POINT('Ctrl Pts',(-2.07261449292824,1.,0.571816823242603));
#29050=CARTESIAN_POINT('Ctrl Pts',(-2.07715226767559,1.,0.576300797416844));
#29051=CARTESIAN_POINT('Ctrl Pts',(-2.08167059018418,1.,0.580819952108063));
#29052=CARTESIAN_POINT('Ctrl Pts',(-2.08616943727951,1.,0.585373918991617));
#29053=CARTESIAN_POINT('Ctrl Pts',(-2.09064881812129,1.,0.589962365403406));
#29054=CARTESIAN_POINT('Ctrl Pts',(-2.0951087622027,1.,0.594585006052162));
#29055=CARTESIAN_POINT('Ctrl Pts',(-2.0995493086477,1.,0.599241616420533));
#29056=CARTESIAN_POINT('Ctrl Pts',(-2.10397049886949,1.,0.60393203073603));
#29057=CARTESIAN_POINT('Ctrl Pts',(-2.1074919961518,1.,0.607711315454876));
#29058=CARTESIAN_POINT('Ctrl Pts',(-2.11012443807238,1.,0.610560911689899));
#29059=CARTESIAN_POINT('Ctrl Pts',(-2.11187554259986,1.,0.6124673655618));
#29060=CARTESIAN_POINT('Ctrl Pts',(-2.11275013067528,1.,0.61342227326009));
#29061=CARTESIAN_POINT('',(-1.7075470150345,0.,0.383122945602003));
#29062=CARTESIAN_POINT('Origin',(0.,0.,0.));
#29063=CARTESIAN_POINT('',(-1.74236521665491,1.,0.163289472382896));
#29064=CARTESIAN_POINT('Origin',(0.,1.,0.));
#29065=CARTESIAN_POINT('',(-1.74236521665491,0.,0.163289472382896));
#29066=CARTESIAN_POINT('Ctrl Pts',(-2.19890268624765,-1.,0.069476445021958));
#29067=CARTESIAN_POINT('Ctrl Pts',(-2.19890268624765,1.,0.069476445021958));
#29068=CARTESIAN_POINT('Ctrl Pts',(-2.19777582085423,-1.,0.0701143536325489));
#29069=CARTESIAN_POINT('Ctrl Pts',(-2.19777582085423,1.,0.0701143536325489));
#29070=CARTESIAN_POINT('Ctrl Pts',(-2.19552129484002,-1.,0.0713863779526153));
#29071=CARTESIAN_POINT('Ctrl Pts',(-2.19552129484002,1.,0.0713863779526153));
#29072=CARTESIAN_POINT('Ctrl Pts',(-2.19213712013662,-1.,0.0732830357306724));
#29073=CARTESIAN_POINT('Ctrl Pts',(-2.19213712013662,1.,0.0732830357306724));
#29074=CARTESIAN_POINT('Ctrl Pts',(-2.1876201139953,-1.,0.0757891465836146));
#29075=CARTESIAN_POINT('Ctrl Pts',(-2.1876201139953,1.,0.0757891465836146));
#29076=CARTESIAN_POINT('Ctrl Pts',(-2.18196589448887,-1.,0.0788837727685241));
#29077=CARTESIAN_POINT('Ctrl Pts',(-2.18196589448887,1.,0.0788837727685241));
#29078=CARTESIAN_POINT('Ctrl Pts',(-2.176303712113,-1.,0.0819402680872764));
#29079=CARTESIAN_POINT('Ctrl Pts',(-2.176303712113,1.,0.0819402680872764));
#29080=CARTESIAN_POINT('Ctrl Pts',(-2.17063357870952,-1.,0.0849584620835371));
#29081=CARTESIAN_POINT('Ctrl Pts',(-2.17063357870952,1.,0.0849584620835371));
#29082=CARTESIAN_POINT('Ctrl Pts',(-2.16495552645014,-1.,0.0879381291386921));
#29083=CARTESIAN_POINT('Ctrl Pts',(-2.16495552645014,1.,0.0879381291386921));
#29084=CARTESIAN_POINT('Ctrl Pts',(-2.15926961544516,-1.,0.0908789888107264));
#29085=CARTESIAN_POINT('Ctrl Pts',(-2.15926961544516,1.,0.0908789888107264));
#29086=CARTESIAN_POINT('Ctrl Pts',(-2.1535759397817,-1.,0.0937807218867642));
#29087=CARTESIAN_POINT('Ctrl Pts',(-2.1535759397817,1.,0.0937807218867642));
#29088=CARTESIAN_POINT('Ctrl Pts',(-2.14787463531795,-1.,0.0966429852305457));
#29089=CARTESIAN_POINT('Ctrl Pts',(-2.14787463531795,1.,0.0966429852305457));
#29090=CARTESIAN_POINT('Ctrl Pts',(-2.14216588396025,-1.,0.0994654261990914));
#29091=CARTESIAN_POINT('Ctrl Pts',(-2.14216588396025,1.,0.0994654261990914));
#29092=CARTESIAN_POINT('Ctrl Pts',(-2.13644992667165,-1.,0.1022477005561));
#29093=CARTESIAN_POINT('Ctrl Pts',(-2.13644992667165,1.,0.1022477005561));
#29094=CARTESIAN_POINT('Ctrl Pts',(-2.13072704887293,-1.,0.104989479152739));
#29095=CARTESIAN_POINT('Ctrl Pts',(-2.13072704887293,1.,0.104989479152739));
#29096=CARTESIAN_POINT('Ctrl Pts',(-2.12499752307,-1.,0.10769043523109));
#29097=CARTESIAN_POINT('Ctrl Pts',(-2.12499752307,1.,0.10769043523109));
#29098=CARTESIAN_POINT('Ctrl Pts',(-2.11926155590865,-1.,0.110350236135025));
#29099=CARTESIAN_POINT('Ctrl Pts',(-2.11926155590865,1.,0.110350236135025));
#29100=CARTESIAN_POINT('Ctrl Pts',(-2.11351924490306,-1.,0.112968534419737));
#29101=CARTESIAN_POINT('Ctrl Pts',(-2.11351924490306,1.,0.112968534419737));
#29102=CARTESIAN_POINT('Ctrl Pts',(-2.10777050261309,-1.,0.115544957687926));
#29103=CARTESIAN_POINT('Ctrl Pts',(-2.10777050261309,1.,0.115544957687926));
#29104=CARTESIAN_POINT('Ctrl Pts',(-2.102015121329,-1.,0.118079107988355));
#29105=CARTESIAN_POINT('Ctrl Pts',(-2.102015121329,1.,0.118079107988355));
#29106=CARTESIAN_POINT('Ctrl Pts',(-2.0962529286773,-1.,0.120570567965122));
#29107=CARTESIAN_POINT('Ctrl Pts',(-2.0962529286773,1.,0.120570567965122));
#29108=CARTESIAN_POINT('Ctrl Pts',(-2.09048392424825,-1.,0.123018905621083));
#29109=CARTESIAN_POINT('Ctrl Pts',(-2.09048392424825,1.,0.123018905621083));
#29110=CARTESIAN_POINT('Ctrl Pts',(-2.08470840653643,-1.,0.125423679412061));
#29111=CARTESIAN_POINT('Ctrl Pts',(-2.08470840653643,1.,0.125423679412061));
#29112=CARTESIAN_POINT('Ctrl Pts',(-2.07892715110987,-1.,0.12778444527612));
#29113=CARTESIAN_POINT('Ctrl Pts',(-2.07892715110987,1.,0.12778444527612));
#29114=CARTESIAN_POINT('Ctrl Pts',(-2.07314114713063,-1.,0.130100748328403));
#29115=CARTESIAN_POINT('Ctrl Pts',(-2.07314114713063,1.,0.130100748328403));
#29116=CARTESIAN_POINT('Ctrl Pts',(-2.06735123910326,-1.,0.13237211154771));
#29117=CARTESIAN_POINT('Ctrl Pts',(-2.06735123910326,1.,0.13237211154771));
#29118=CARTESIAN_POINT('Ctrl Pts',(-2.06155781517842,-1.,0.134598026192106));
#29119=CARTESIAN_POINT('Ctrl Pts',(-2.06155781517842,1.,0.134598026192106));
#29120=CARTESIAN_POINT('Ctrl Pts',(-2.05576044414264,-1.,0.136777941218043));
#29121=CARTESIAN_POINT('Ctrl Pts',(-2.05576044414264,1.,0.136777941218043));
#29122=CARTESIAN_POINT('Ctrl Pts',(-2.04995762001328,-1.,0.138911255368966));
#29123=CARTESIAN_POINT('Ctrl Pts',(-2.04995762001328,1.,0.138911255368966));
#29124=CARTESIAN_POINT('Ctrl Pts',(-2.04414757947916,-1.,0.140997332152546));
#29125=CARTESIAN_POINT('Ctrl Pts',(-2.04414757947916,1.,0.140997332152546));
#29126=CARTESIAN_POINT('Ctrl Pts',(-2.03832911025912,-1.,0.143035515058209));
#29127=CARTESIAN_POINT('Ctrl Pts',(-2.03832911025912,1.,0.143035515058209));
#29128=CARTESIAN_POINT('Ctrl Pts',(-2.03250223739942,-1.,0.145025140186057));
#29129=CARTESIAN_POINT('Ctrl Pts',(-2.03250223739942,1.,0.145025140186057));
#29130=CARTESIAN_POINT('Ctrl Pts',(-2.02666926182017,-1.,0.146965557332583));
#29131=CARTESIAN_POINT('Ctrl Pts',(-2.02666926182017,1.,0.146965557332583));
#29132=CARTESIAN_POINT('Ctrl Pts',(-2.02083464969894,-1.,0.148856124775337));
#29133=CARTESIAN_POINT('Ctrl Pts',(-2.02083464969894,1.,0.148856124775337));
#29134=CARTESIAN_POINT('Ctrl Pts',(-2.01500291940238,-1.,0.150696157673078));
#29135=CARTESIAN_POINT('Ctrl Pts',(-2.01500291940238,1.,0.150696157673078));
#29136=CARTESIAN_POINT('Ctrl Pts',(-2.00917680318424,-1.,0.15248488362145));
#29137=CARTESIAN_POINT('Ctrl Pts',(-2.00917680318424,1.,0.15248488362145));
#29138=CARTESIAN_POINT('Ctrl Pts',(-2.00335565310543,-1.,0.154221403049722));
#29139=CARTESIAN_POINT('Ctrl Pts',(-2.00335565310543,1.,0.154221403049722));
#29140=CARTESIAN_POINT('Ctrl Pts',(-1.99753284771497,-1.,0.155904629548783));
#29141=CARTESIAN_POINT('Ctrl Pts',(-1.99753284771497,1.,0.155904629548783));
#29142=CARTESIAN_POINT('Ctrl Pts',(-1.99169810931908,-1.,0.157533331459227));
#29143=CARTESIAN_POINT('Ctrl Pts',(-1.99169810931908,1.,0.157533331459227));
#29144=CARTESIAN_POINT('Ctrl Pts',(-1.98584238283292,-1.,0.159106226437299));
#29145=CARTESIAN_POINT('Ctrl Pts',(-1.98584238283292,1.,0.159106226437299));
#29146=CARTESIAN_POINT('Ctrl Pts',(-1.97996195437559,-1.,0.160622060784611));
#29147=CARTESIAN_POINT('Ctrl Pts',(-1.97996195437559,1.,0.160622060784611));
#29148=CARTESIAN_POINT('Ctrl Pts',(-1.97406280235188,-1.,0.162079693556288));
#29149=CARTESIAN_POINT('Ctrl Pts',(-1.97406280235188,1.,0.162079693556288));
#29150=CARTESIAN_POINT('Ctrl Pts',(-1.96816512677967,-1.,0.163478185457734));
#29151=CARTESIAN_POINT('Ctrl Pts',(-1.96816512677967,1.,0.163478185457734));
#29152=CARTESIAN_POINT('Ctrl Pts',(-1.96229379940136,-1.,0.164816568920269));
#29153=CARTESIAN_POINT('Ctrl Pts',(-1.96229379940136,1.,0.164816568920269));
#29154=CARTESIAN_POINT('Ctrl Pts',(-1.9564675971873,-1.,0.166093592002812));
#29155=CARTESIAN_POINT('Ctrl Pts',(-1.9564675971873,1.,0.166093592002812));
#29156=CARTESIAN_POINT('Ctrl Pts',(-1.95069027794294,-1.,0.167307501784475));
#29157=CARTESIAN_POINT('Ctrl Pts',(-1.95069027794294,1.,0.167307501784475));
#29158=CARTESIAN_POINT('Ctrl Pts',(-1.94493757756931,-1.,0.168455741607556));
#29159=CARTESIAN_POINT('Ctrl Pts',(-1.94493757756931,1.,0.168455741607556));
#29160=CARTESIAN_POINT('Ctrl Pts',(-1.93915639211581,-1.,0.169534904817491));
#29161=CARTESIAN_POINT('Ctrl Pts',(-1.93915639211581,1.,0.169534904817491));
#29162=CARTESIAN_POINT('Ctrl Pts',(-1.93329183155539,-1.,0.170541253116201));
#29163=CARTESIAN_POINT('Ctrl Pts',(-1.93329183155539,1.,0.170541253116201));
#29164=CARTESIAN_POINT('Ctrl Pts',(-1.92731093582036,-1.,0.171471191532988));
#29165=CARTESIAN_POINT('Ctrl Pts',(-1.92731093582036,1.,0.171471191532988));
#29166=CARTESIAN_POINT('Ctrl Pts',(-1.9212233439798,-1.,0.172321621259514));
#29167=CARTESIAN_POINT('Ctrl Pts',(-1.9212233439798,1.,0.172321621259514));
#29168=CARTESIAN_POINT('Ctrl Pts',(-1.91511429159527,-1.,0.173090695383496));
#29169=CARTESIAN_POINT('Ctrl Pts',(-1.91511429159527,1.,0.173090695383496));
#29170=CARTESIAN_POINT('Ctrl Pts',(-1.90911693975267,-1.,0.173776635257817));
#29171=CARTESIAN_POINT('Ctrl Pts',(-1.90911693975267,1.,0.173776635257817));
#29172=CARTESIAN_POINT('Ctrl Pts',(-1.90335253862834,-1.,0.174375518661085));
#29173=CARTESIAN_POINT('Ctrl Pts',(-1.90335253862834,1.,0.174375518661085));
#29174=CARTESIAN_POINT('Ctrl Pts',(-1.89788101117132,-1.,0.174879405091263));
#29175=CARTESIAN_POINT('Ctrl Pts',(-1.89788101117132,1.,0.174879405091263));
#29176=CARTESIAN_POINT('Ctrl Pts',(-1.892646301985,-1.,0.175274276190844));
#29177=CARTESIAN_POINT('Ctrl Pts',(-1.892646301985,1.,0.175274276190844));
#29178=CARTESIAN_POINT('Ctrl Pts',(-1.88742606273259,-1.,0.175538155840648));
#29179=CARTESIAN_POINT('Ctrl Pts',(-1.88742606273259,1.,0.175538155840648));
#29180=CARTESIAN_POINT('Ctrl Pts',(-1.88188663145367,-1.,0.175644148889698));
#29181=CARTESIAN_POINT('Ctrl Pts',(-1.88188663145367,1.,0.175644148889698));
#29182=CARTESIAN_POINT('Ctrl Pts',(-1.87563767773588,-1.,0.175563480746485));
#29183=CARTESIAN_POINT('Ctrl Pts',(-1.87563767773588,1.,0.175563480746485));
#29184=CARTESIAN_POINT('Ctrl Pts',(-1.86828349694799,-1.,0.175268337590758));
#29185=CARTESIAN_POINT('Ctrl Pts',(-1.86828349694799,1.,0.175268337590758));
#29186=CARTESIAN_POINT('Ctrl Pts',(-1.85948367088837,-1.,0.17473525927603));
#29187=CARTESIAN_POINT('Ctrl Pts',(-1.85948367088837,1.,0.17473525927603));
#29188=CARTESIAN_POINT('Ctrl Pts',(-1.8489811319852,-1.,0.173946627587731));
#29189=CARTESIAN_POINT('Ctrl Pts',(-1.8489811319852,1.,0.173946627587731));
#29190=CARTESIAN_POINT('Ctrl Pts',(-1.83658380527692,-1.,0.1728894428919));
#29191=CARTESIAN_POINT('Ctrl Pts',(-1.83658380527692,1.,0.1728894428919));
#29192=CARTESIAN_POINT('Ctrl Pts',(-1.82215766811545,-1.,0.171554770204119));
#29193=CARTESIAN_POINT('Ctrl Pts',(-1.82215766811545,1.,0.171554770204119));
#29194=CARTESIAN_POINT('Ctrl Pts',(-1.80561530629706,-1.,0.169936923904608));
#29195=CARTESIAN_POINT('Ctrl Pts',(-1.80561530629706,1.,0.169936923904608));
#29196=CARTESIAN_POINT('Ctrl Pts',(-1.7869064998507,-1.,0.168032772805197));
#29197=CARTESIAN_POINT('Ctrl Pts',(-1.7869064998507,1.,0.168032772805197));
#29198=CARTESIAN_POINT('Ctrl Pts',(-1.77018771684844,-1.,0.1662793551464));
#29199=CARTESIAN_POINT('Ctrl Pts',(-1.77018771684844,1.,0.1662793551464));
#29200=CARTESIAN_POINT('Ctrl Pts',(-1.75666056638427,-1.,0.164834765707158));
#29201=CARTESIAN_POINT('Ctrl Pts',(-1.75666056638427,1.,0.164834765707158));
#29202=CARTESIAN_POINT('Ctrl Pts',(-1.7472034950333,-1.,0.163814161002002));
#29203=CARTESIAN_POINT('Ctrl Pts',(-1.7472034950333,1.,0.163814161002002));
#29204=CARTESIAN_POINT('Ctrl Pts',(-1.74236521665491,-1.,0.163289472382896));
#29205=CARTESIAN_POINT('Ctrl Pts',(-1.74236521665491,1.,0.163289472382896));
#29206=CARTESIAN_POINT('',(-2.19890268624765,1.,0.069476445021958));
#29207=CARTESIAN_POINT('Ctrl Pts',(-2.19890268624765,1.,0.069476445021958));
#29208=CARTESIAN_POINT('Ctrl Pts',(-2.19777582085423,1.,0.0701143536325489));
#29209=CARTESIAN_POINT('Ctrl Pts',(-2.19552129484002,1.,0.0713863779526153));
#29210=CARTESIAN_POINT('Ctrl Pts',(-2.19213712013662,1.,0.0732830357306724));
#29211=CARTESIAN_POINT('Ctrl Pts',(-2.1876201139953,1.,0.0757891465836146));
#29212=CARTESIAN_POINT('Ctrl Pts',(-2.18196589448887,1.,0.0788837727685241));
#29213=CARTESIAN_POINT('Ctrl Pts',(-2.176303712113,1.,0.0819402680872764));
#29214=CARTESIAN_POINT('Ctrl Pts',(-2.17063357870952,1.,0.0849584620835371));
#29215=CARTESIAN_POINT('Ctrl Pts',(-2.16495552645014,1.,0.0879381291386921));
#29216=CARTESIAN_POINT('Ctrl Pts',(-2.15926961544516,1.,0.0908789888107264));
#29217=CARTESIAN_POINT('Ctrl Pts',(-2.1535759397817,1.,0.0937807218867642));
#29218=CARTESIAN_POINT('Ctrl Pts',(-2.14787463531795,1.,0.0966429852305457));
#29219=CARTESIAN_POINT('Ctrl Pts',(-2.14216588396025,1.,0.0994654261990914));
#29220=CARTESIAN_POINT('Ctrl Pts',(-2.13644992667165,1.,0.1022477005561));
#29221=CARTESIAN_POINT('Ctrl Pts',(-2.13072704887293,1.,0.104989479152739));
#29222=CARTESIAN_POINT('Ctrl Pts',(-2.12499752307,1.,0.10769043523109));
#29223=CARTESIAN_POINT('Ctrl Pts',(-2.11926155590865,1.,0.110350236135025));
#29224=CARTESIAN_POINT('Ctrl Pts',(-2.11351924490306,1.,0.112968534419737));
#29225=CARTESIAN_POINT('Ctrl Pts',(-2.10777050261309,1.,0.115544957687926));
#29226=CARTESIAN_POINT('Ctrl Pts',(-2.102015121329,1.,0.118079107988355));
#29227=CARTESIAN_POINT('Ctrl Pts',(-2.0962529286773,1.,0.120570567965122));
#29228=CARTESIAN_POINT('Ctrl Pts',(-2.09048392424825,1.,0.123018905621083));
#29229=CARTESIAN_POINT('Ctrl Pts',(-2.08470840653643,1.,0.125423679412061));
#29230=CARTESIAN_POINT('Ctrl Pts',(-2.07892715110987,1.,0.12778444527612));
#29231=CARTESIAN_POINT('Ctrl Pts',(-2.07314114713063,1.,0.130100748328403));
#29232=CARTESIAN_POINT('Ctrl Pts',(-2.06735123910326,1.,0.13237211154771));
#29233=CARTESIAN_POINT('Ctrl Pts',(-2.06155781517842,1.,0.134598026192106));
#29234=CARTESIAN_POINT('Ctrl Pts',(-2.05576044414264,1.,0.136777941218043));
#29235=CARTESIAN_POINT('Ctrl Pts',(-2.04995762001328,1.,0.138911255368966));
#29236=CARTESIAN_POINT('Ctrl Pts',(-2.04414757947916,1.,0.140997332152546));
#29237=CARTESIAN_POINT('Ctrl Pts',(-2.03832911025912,1.,0.143035515058209));
#29238=CARTESIAN_POINT('Ctrl Pts',(-2.03250223739942,1.,0.145025140186057));
#29239=CARTESIAN_POINT('Ctrl Pts',(-2.02666926182017,1.,0.146965557332583));
#29240=CARTESIAN_POINT('Ctrl Pts',(-2.02083464969894,1.,0.148856124775337));
#29241=CARTESIAN_POINT('Ctrl Pts',(-2.01500291940238,1.,0.150696157673078));
#29242=CARTESIAN_POINT('Ctrl Pts',(-2.00917680318424,1.,0.15248488362145));
#29243=CARTESIAN_POINT('Ctrl Pts',(-2.00335565310543,1.,0.154221403049722));
#29244=CARTESIAN_POINT('Ctrl Pts',(-1.99753284771497,1.,0.155904629548783));
#29245=CARTESIAN_POINT('Ctrl Pts',(-1.99169810931908,1.,0.157533331459227));
#29246=CARTESIAN_POINT('Ctrl Pts',(-1.98584238283292,1.,0.159106226437299));
#29247=CARTESIAN_POINT('Ctrl Pts',(-1.97996195437559,1.,0.160622060784611));
#29248=CARTESIAN_POINT('Ctrl Pts',(-1.97406280235188,1.,0.162079693556288));
#29249=CARTESIAN_POINT('Ctrl Pts',(-1.96816512677967,1.,0.163478185457734));
#29250=CARTESIAN_POINT('Ctrl Pts',(-1.96229379940136,1.,0.164816568920269));
#29251=CARTESIAN_POINT('Ctrl Pts',(-1.9564675971873,1.,0.166093592002812));
#29252=CARTESIAN_POINT('Ctrl Pts',(-1.95069027794294,1.,0.167307501784475));
#29253=CARTESIAN_POINT('Ctrl Pts',(-1.94493757756931,1.,0.168455741607556));
#29254=CARTESIAN_POINT('Ctrl Pts',(-1.93915639211581,1.,0.169534904817491));
#29255=CARTESIAN_POINT('Ctrl Pts',(-1.93329183155539,1.,0.170541253116201));
#29256=CARTESIAN_POINT('Ctrl Pts',(-1.92731093582036,1.,0.171471191532988));
#29257=CARTESIAN_POINT('Ctrl Pts',(-1.9212233439798,1.,0.172321621259514));
#29258=CARTESIAN_POINT('Ctrl Pts',(-1.91511429159527,1.,0.173090695383496));
#29259=CARTESIAN_POINT('Ctrl Pts',(-1.90911693975267,1.,0.173776635257817));
#29260=CARTESIAN_POINT('Ctrl Pts',(-1.90335253862834,1.,0.174375518661085));
#29261=CARTESIAN_POINT('Ctrl Pts',(-1.89788101117132,1.,0.174879405091263));
#29262=CARTESIAN_POINT('Ctrl Pts',(-1.892646301985,1.,0.175274276190844));
#29263=CARTESIAN_POINT('Ctrl Pts',(-1.88742606273259,1.,0.175538155840648));
#29264=CARTESIAN_POINT('Ctrl Pts',(-1.88188663145367,1.,0.175644148889698));
#29265=CARTESIAN_POINT('Ctrl Pts',(-1.87563767773588,1.,0.175563480746485));
#29266=CARTESIAN_POINT('Ctrl Pts',(-1.86828349694799,1.,0.175268337590758));
#29267=CARTESIAN_POINT('Ctrl Pts',(-1.85948367088837,1.,0.17473525927603));
#29268=CARTESIAN_POINT('Ctrl Pts',(-1.8489811319852,1.,0.173946627587731));
#29269=CARTESIAN_POINT('Ctrl Pts',(-1.83658380527692,1.,0.1728894428919));
#29270=CARTESIAN_POINT('Ctrl Pts',(-1.82215766811545,1.,0.171554770204119));
#29271=CARTESIAN_POINT('Ctrl Pts',(-1.80561530629706,1.,0.169936923904608));
#29272=CARTESIAN_POINT('Ctrl Pts',(-1.7869064998507,1.,0.168032772805197));
#29273=CARTESIAN_POINT('Ctrl Pts',(-1.77018771684844,1.,0.1662793551464));
#29274=CARTESIAN_POINT('Ctrl Pts',(-1.75666056638427,1.,0.164834765707158));
#29275=CARTESIAN_POINT('Ctrl Pts',(-1.7472034950333,1.,0.163814161002002));
#29276=CARTESIAN_POINT('Ctrl Pts',(-1.74236521665491,1.,0.163289472382896));
#29277=CARTESIAN_POINT('',(-2.19890268624765,0.,0.069476445021958));
#29278=CARTESIAN_POINT('Origin',(-2.19890268624765,0.,-0.0694764450219585));
#29279=CARTESIAN_POINT('',(-2.19890268624765,1.,-0.0694764450219585));
#29280=CARTESIAN_POINT('',(-2.19890268624765,1.,0.069476445021958));
#29281=CARTESIAN_POINT('',(-2.19890268624765,0.,-0.0694764450219585));
#29282=CARTESIAN_POINT('Ctrl Pts',(-1.74236521665491,-1.,-0.163289472382896));
#29283=CARTESIAN_POINT('Ctrl Pts',(-1.74236521665491,1.,-0.163289472382896));
#29284=CARTESIAN_POINT('Ctrl Pts',(-1.74720349503904,-1.,-0.163814161002474));
#29285=CARTESIAN_POINT('Ctrl Pts',(-1.74720349503904,1.,-0.163814161002474));
#29286=CARTESIAN_POINT('Ctrl Pts',(-1.75666056640041,-1.,-0.164834765708484));
#29287=CARTESIAN_POINT('Ctrl Pts',(-1.75666056640041,1.,-0.164834765708484));
#29288=CARTESIAN_POINT('Ctrl Pts',(-1.77018771687692,-1.,-0.166279355148738));
#29289=CARTESIAN_POINT('Ctrl Pts',(-1.77018771687692,1.,-0.166279355148738));
#29290=CARTESIAN_POINT('Ctrl Pts',(-1.78690649988931,-1.,-0.16803277280837));
#29291=CARTESIAN_POINT('Ctrl Pts',(-1.78690649988931,1.,-0.16803277280837));
#29292=CARTESIAN_POINT('Ctrl Pts',(-1.80561530633924,-1.,-0.169936923908078));
#29293=CARTESIAN_POINT('Ctrl Pts',(-1.80561530633924,1.,-0.169936923908078));
#29294=CARTESIAN_POINT('Ctrl Pts',(-1.82215766815414,-1.,-0.171554770207306));
#29295=CARTESIAN_POINT('Ctrl Pts',(-1.82215766815414,1.,-0.171554770207306));
#29296=CARTESIAN_POINT('Ctrl Pts',(-1.83658380530747,-1.,-0.17288944289442));
#29297=CARTESIAN_POINT('Ctrl Pts',(-1.83658380530747,1.,-0.17288944289442));
#29298=CARTESIAN_POINT('Ctrl Pts',(-1.84898113200543,-1.,-0.173946627589401));
#29299=CARTESIAN_POINT('Ctrl Pts',(-1.84898113200543,1.,-0.173946627589401));
#29300=CARTESIAN_POINT('Ctrl Pts',(-1.85948367089838,-1.,-0.174735259276856));
#29301=CARTESIAN_POINT('Ctrl Pts',(-1.85948367089838,1.,-0.174735259276856));
#29302=CARTESIAN_POINT('Ctrl Pts',(-1.86828349694972,-1.,-0.175268337590901));
#29303=CARTESIAN_POINT('Ctrl Pts',(-1.86828349694972,1.,-0.175268337590901));
#29304=CARTESIAN_POINT('Ctrl Pts',(-1.87563767773249,-1.,-0.175563480746205));
#29305=CARTESIAN_POINT('Ctrl Pts',(-1.87563767773249,1.,-0.175563480746205));
#29306=CARTESIAN_POINT('Ctrl Pts',(-1.88188663144846,-1.,-0.175644148889271));
#29307=CARTESIAN_POINT('Ctrl Pts',(-1.88188663144846,1.,-0.175644148889271));
#29308=CARTESIAN_POINT('Ctrl Pts',(-1.88742606272818,-1.,-0.175538155840286));
#29309=CARTESIAN_POINT('Ctrl Pts',(-1.88742606272818,1.,-0.175538155840286));
#29310=CARTESIAN_POINT('Ctrl Pts',(-1.89264630198279,-1.,-0.175274276190664));
#29311=CARTESIAN_POINT('Ctrl Pts',(-1.89264630198279,1.,-0.175274276190664));
#29312=CARTESIAN_POINT('Ctrl Pts',(-1.89788101117148,-1.,-0.174879405091277));
#29313=CARTESIAN_POINT('Ctrl Pts',(-1.89788101117148,1.,-0.174879405091277));
#29314=CARTESIAN_POINT('Ctrl Pts',(-1.90335253863003,-1.,-0.174375518661222));
#29315=CARTESIAN_POINT('Ctrl Pts',(-1.90335253863003,1.,-0.174375518661222));
#29316=CARTESIAN_POINT('Ctrl Pts',(-1.90911693975475,-1.,-0.173776635257984));
#29317=CARTESIAN_POINT('Ctrl Pts',(-1.90911693975475,1.,-0.173776635257984));
#29318=CARTESIAN_POINT('Ctrl Pts',(-1.91511429159681,-1.,-0.173090695383619));
#29319=CARTESIAN_POINT('Ctrl Pts',(-1.91511429159681,1.,-0.173090695383619));
#29320=CARTESIAN_POINT('Ctrl Pts',(-1.92122334398034,-1.,-0.172321621259557));
#29321=CARTESIAN_POINT('Ctrl Pts',(-1.92122334398034,1.,-0.172321621259557));
#29322=CARTESIAN_POINT('Ctrl Pts',(-1.92731093582,-1.,-0.17147119153296));
#29323=CARTESIAN_POINT('Ctrl Pts',(-1.92731093582,1.,-0.17147119153296));
#29324=CARTESIAN_POINT('Ctrl Pts',(-1.93329183155455,-1.,-0.170541253116136));
#29325=CARTESIAN_POINT('Ctrl Pts',(-1.93329183155455,1.,-0.170541253116136));
#29326=CARTESIAN_POINT('Ctrl Pts',(-1.93915639211497,-1.,-0.169534904817425));
#29327=CARTESIAN_POINT('Ctrl Pts',(-1.93915639211497,1.,-0.169534904817425));
#29328=CARTESIAN_POINT('Ctrl Pts',(-1.94493757756879,-1.,-0.168455741607516));
#29329=CARTESIAN_POINT('Ctrl Pts',(-1.94493757756879,1.,-0.168455741607516));
#29330=CARTESIAN_POINT('Ctrl Pts',(-1.95069027794286,-1.,-0.167307501784469));
#29331=CARTESIAN_POINT('Ctrl Pts',(-1.95069027794286,1.,-0.167307501784469));
#29332=CARTESIAN_POINT('Ctrl Pts',(-1.95646759718755,-1.,-0.166093592002833));
#29333=CARTESIAN_POINT('Ctrl Pts',(-1.95646759718755,1.,-0.166093592002833));
#29334=CARTESIAN_POINT('Ctrl Pts',(-1.96229379940174,-1.,-0.1648165689203));
#29335=CARTESIAN_POINT('Ctrl Pts',(-1.96229379940174,1.,-0.1648165689203));
#29336=CARTESIAN_POINT('Ctrl Pts',(-1.96816512678,-1.,-0.16347818545776));
#29337=CARTESIAN_POINT('Ctrl Pts',(-1.96816512678,1.,-0.16347818545776));
#29338=CARTESIAN_POINT('Ctrl Pts',(-1.97406280235204,-1.,-0.162079693556302));
#29339=CARTESIAN_POINT('Ctrl Pts',(-1.97406280235204,1.,-0.162079693556302));
#29340=CARTESIAN_POINT('Ctrl Pts',(-1.97996195437557,-1.,-0.16062206078461));
#29341=CARTESIAN_POINT('Ctrl Pts',(-1.97996195437557,1.,-0.16062206078461));
#29342=CARTESIAN_POINT('Ctrl Pts',(-1.98584238283279,-1.,-0.159106226437289));
#29343=CARTESIAN_POINT('Ctrl Pts',(-1.98584238283279,1.,-0.159106226437289));
#29344=CARTESIAN_POINT('Ctrl Pts',(-1.99169810931893,-1.,-0.157533331459215));
#29345=CARTESIAN_POINT('Ctrl Pts',(-1.99169810931893,1.,-0.157533331459215));
#29346=CARTESIAN_POINT('Ctrl Pts',(-1.99753284771487,-1.,-0.155904629548775));
#29347=CARTESIAN_POINT('Ctrl Pts',(-1.99753284771487,1.,-0.155904629548775));
#29348=CARTESIAN_POINT('Ctrl Pts',(-2.00335565310539,-1.,-0.154221403049719));
#29349=CARTESIAN_POINT('Ctrl Pts',(-2.00335565310539,1.,-0.154221403049719));
#29350=CARTESIAN_POINT('Ctrl Pts',(-2.00917680318426,-1.,-0.152484883621452));
#29351=CARTESIAN_POINT('Ctrl Pts',(-2.00917680318426,1.,-0.152484883621452));
#29352=CARTESIAN_POINT('Ctrl Pts',(-2.01500291940243,-1.,-0.150696157673084));
#29353=CARTESIAN_POINT('Ctrl Pts',(-2.01500291940243,1.,-0.150696157673084));
#29354=CARTESIAN_POINT('Ctrl Pts',(-2.02083464969897,-1.,-0.148856124775343));
#29355=CARTESIAN_POINT('Ctrl Pts',(-2.02083464969897,1.,-0.148856124775343));
#29356=CARTESIAN_POINT('Ctrl Pts',(-2.02666926182017,-1.,-0.146965557332586));
#29357=CARTESIAN_POINT('Ctrl Pts',(-2.02666926182017,1.,-0.146965557332586));
#29358=CARTESIAN_POINT('Ctrl Pts',(-2.03250223739941,-1.,-0.145025140186058));
#29359=CARTESIAN_POINT('Ctrl Pts',(-2.03250223739941,1.,-0.145025140186058));
#29360=CARTESIAN_POINT('Ctrl Pts',(-2.03832911025913,-1.,-0.143035515058208));
#29361=CARTESIAN_POINT('Ctrl Pts',(-2.03832911025913,1.,-0.143035515058208));
#29362=CARTESIAN_POINT('Ctrl Pts',(-2.04414757947919,-1.,-0.140997332152545));
#29363=CARTESIAN_POINT('Ctrl Pts',(-2.04414757947919,1.,-0.140997332152545));
#29364=CARTESIAN_POINT('Ctrl Pts',(-2.04995762001333,-1.,-0.138911255368966));
#29365=CARTESIAN_POINT('Ctrl Pts',(-2.04995762001333,1.,-0.138911255368966));
#29366=CARTESIAN_POINT('Ctrl Pts',(-2.0557604441427,-1.,-0.136777941218044));
#29367=CARTESIAN_POINT('Ctrl Pts',(-2.0557604441427,1.,-0.136777941218044));
#29368=CARTESIAN_POINT('Ctrl Pts',(-2.06155781517844,-1.,-0.134598026192107));
#29369=CARTESIAN_POINT('Ctrl Pts',(-2.06155781517844,1.,-0.134598026192107));
#29370=CARTESIAN_POINT('Ctrl Pts',(-2.06735123910319,-1.,-0.13237211154771));
#29371=CARTESIAN_POINT('Ctrl Pts',(-2.06735123910319,1.,-0.13237211154771));
#29372=CARTESIAN_POINT('Ctrl Pts',(-2.07314114713047,-1.,-0.130100748328401));
#29373=CARTESIAN_POINT('Ctrl Pts',(-2.07314114713047,1.,-0.130100748328401));
#29374=CARTESIAN_POINT('Ctrl Pts',(-2.07892715110967,-1.,-0.127784445276116));
#29375=CARTESIAN_POINT('Ctrl Pts',(-2.07892715110967,1.,-0.127784445276116));
#29376=CARTESIAN_POINT('Ctrl Pts',(-2.08470840653628,-1.,-0.125423679412058));
#29377=CARTESIAN_POINT('Ctrl Pts',(-2.08470840653628,1.,-0.125423679412058));
#29378=CARTESIAN_POINT('Ctrl Pts',(-2.09048392424826,-1.,-0.123018905621083));
#29379=CARTESIAN_POINT('Ctrl Pts',(-2.09048392424826,1.,-0.123018905621083));
#29380=CARTESIAN_POINT('Ctrl Pts',(-2.09625292867756,-1.,-0.120570567965129));
#29381=CARTESIAN_POINT('Ctrl Pts',(-2.09625292867756,1.,-0.120570567965129));
#29382=CARTESIAN_POINT('Ctrl Pts',(-2.10201512132945,-1.,-0.118079107988368));
#29383=CARTESIAN_POINT('Ctrl Pts',(-2.10201512132945,1.,-0.118079107988368));
#29384=CARTESIAN_POINT('Ctrl Pts',(-2.10777050261359,-1.,-0.11554495768794));
#29385=CARTESIAN_POINT('Ctrl Pts',(-2.10777050261359,1.,-0.11554495768794));
#29386=CARTESIAN_POINT('Ctrl Pts',(-2.11351924490335,-1.,-0.112968534419746));
#29387=CARTESIAN_POINT('Ctrl Pts',(-2.11351924490335,1.,-0.112968534419746));
#29388=CARTESIAN_POINT('Ctrl Pts',(-2.11926155590849,-1.,-0.11035023613502));
#29389=CARTESIAN_POINT('Ctrl Pts',(-2.11926155590849,1.,-0.11035023613502));
#29390=CARTESIAN_POINT('Ctrl Pts',(-2.12499752306927,-1.,-0.107690435231068));
#29391=CARTESIAN_POINT('Ctrl Pts',(-2.12499752306927,1.,-0.107690435231068));
#29392=CARTESIAN_POINT('Ctrl Pts',(-2.1307270488718,-1.,-0.104989479152703));
#29393=CARTESIAN_POINT('Ctrl Pts',(-2.1307270488718,1.,-0.104989479152703));
#29394=CARTESIAN_POINT('Ctrl Pts',(-2.13644992667052,-1.,-0.102247700556064));
#29395=CARTESIAN_POINT('Ctrl Pts',(-2.13644992667052,1.,-0.102247700556064));
#29396=CARTESIAN_POINT('Ctrl Pts',(-2.14216588395974,-1.,-0.0994654261990744));
#29397=CARTESIAN_POINT('Ctrl Pts',(-2.14216588395974,1.,-0.0994654261990744));
#29398=CARTESIAN_POINT('Ctrl Pts',(-2.14787463531864,-1.,-0.096642985230569));
#29399=CARTESIAN_POINT('Ctrl Pts',(-2.14787463531864,1.,-0.096642985230569));
#29400=CARTESIAN_POINT('Ctrl Pts',(-2.15357593978377,-1.,-0.0937807218868346));
#29401=CARTESIAN_POINT('Ctrl Pts',(-2.15357593978377,1.,-0.0937807218868346));
#29402=CARTESIAN_POINT('Ctrl Pts',(-2.15926961544808,-1.,-0.0908789888108267));
#29403=CARTESIAN_POINT('Ctrl Pts',(-2.15926961544808,1.,-0.0908789888108267));
#29404=CARTESIAN_POINT('Ctrl Pts',(-2.16495552645275,-1.,-0.0879381291387824));
#29405=CARTESIAN_POINT('Ctrl Pts',(-2.16495552645275,1.,-0.0879381291387824));
#29406=CARTESIAN_POINT('Ctrl Pts',(-2.17063357871031,-1.,-0.0849584620835644));
#29407=CARTESIAN_POINT('Ctrl Pts',(-2.17063357871031,1.,-0.0849584620835644));
#29408=CARTESIAN_POINT('Ctrl Pts',(-2.1763037121106,-1.,-0.0819402680871941));
#29409=CARTESIAN_POINT('Ctrl Pts',(-2.1763037121106,1.,-0.0819402680871941));
#29410=CARTESIAN_POINT('Ctrl Pts',(-2.18196589448304,-1.,-0.0788837727683229));
#29411=CARTESIAN_POINT('Ctrl Pts',(-2.18196589448304,1.,-0.0788837727683229));
#29412=CARTESIAN_POINT('Ctrl Pts',(-2.1876201139874,-1.,-0.0757891465833413));
#29413=CARTESIAN_POINT('Ctrl Pts',(-2.1876201139874,1.,-0.0757891465833413));
#29414=CARTESIAN_POINT('Ctrl Pts',(-2.19213712012956,-1.,-0.0732830357304277));
#29415=CARTESIAN_POINT('Ctrl Pts',(-2.19213712012956,1.,-0.0732830357304277));
#29416=CARTESIAN_POINT('Ctrl Pts',(-2.19552129483562,-1.,-0.0713863779524629));
#29417=CARTESIAN_POINT('Ctrl Pts',(-2.19552129483562,1.,-0.0713863779524629));
#29418=CARTESIAN_POINT('Ctrl Pts',(-2.19777582085261,-1.,-0.0701143536324927));
#29419=CARTESIAN_POINT('Ctrl Pts',(-2.19777582085261,1.,-0.0701143536324927));
#29420=CARTESIAN_POINT('Ctrl Pts',(-2.19890268624765,-1.,-0.0694764450219585));
#29421=CARTESIAN_POINT('Ctrl Pts',(-2.19890268624765,1.,-0.0694764450219585));
#29422=CARTESIAN_POINT('',(-1.74236521665491,1.,-0.163289472382896));
#29423=CARTESIAN_POINT('Ctrl Pts',(-1.74236521665491,1.,-0.163289472382896));
#29424=CARTESIAN_POINT('Ctrl Pts',(-1.74720349503904,1.,-0.163814161002474));
#29425=CARTESIAN_POINT('Ctrl Pts',(-1.75666056640041,1.,-0.164834765708484));
#29426=CARTESIAN_POINT('Ctrl Pts',(-1.77018771687692,1.,-0.166279355148738));
#29427=CARTESIAN_POINT('Ctrl Pts',(-1.78690649988931,1.,-0.16803277280837));
#29428=CARTESIAN_POINT('Ctrl Pts',(-1.80561530633924,1.,-0.169936923908078));
#29429=CARTESIAN_POINT('Ctrl Pts',(-1.82215766815414,1.,-0.171554770207306));
#29430=CARTESIAN_POINT('Ctrl Pts',(-1.83658380530747,1.,-0.17288944289442));
#29431=CARTESIAN_POINT('Ctrl Pts',(-1.84898113200543,1.,-0.173946627589401));
#29432=CARTESIAN_POINT('Ctrl Pts',(-1.85948367089838,1.,-0.174735259276856));
#29433=CARTESIAN_POINT('Ctrl Pts',(-1.86828349694972,1.,-0.175268337590901));
#29434=CARTESIAN_POINT('Ctrl Pts',(-1.87563767773249,1.,-0.175563480746205));
#29435=CARTESIAN_POINT('Ctrl Pts',(-1.88188663144846,1.,-0.175644148889271));
#29436=CARTESIAN_POINT('Ctrl Pts',(-1.88742606272818,1.,-0.175538155840286));
#29437=CARTESIAN_POINT('Ctrl Pts',(-1.89264630198279,1.,-0.175274276190664));
#29438=CARTESIAN_POINT('Ctrl Pts',(-1.89788101117148,1.,-0.174879405091277));
#29439=CARTESIAN_POINT('Ctrl Pts',(-1.90335253863003,1.,-0.174375518661222));
#29440=CARTESIAN_POINT('Ctrl Pts',(-1.90911693975475,1.,-0.173776635257984));
#29441=CARTESIAN_POINT('Ctrl Pts',(-1.91511429159681,1.,-0.173090695383619));
#29442=CARTESIAN_POINT('Ctrl Pts',(-1.92122334398034,1.,-0.172321621259557));
#29443=CARTESIAN_POINT('Ctrl Pts',(-1.92731093582,1.,-0.17147119153296));
#29444=CARTESIAN_POINT('Ctrl Pts',(-1.93329183155455,1.,-0.170541253116136));
#29445=CARTESIAN_POINT('Ctrl Pts',(-1.93915639211497,1.,-0.169534904817425));
#29446=CARTESIAN_POINT('Ctrl Pts',(-1.94493757756879,1.,-0.168455741607516));
#29447=CARTESIAN_POINT('Ctrl Pts',(-1.95069027794286,1.,-0.167307501784469));
#29448=CARTESIAN_POINT('Ctrl Pts',(-1.95646759718755,1.,-0.166093592002833));
#29449=CARTESIAN_POINT('Ctrl Pts',(-1.96229379940174,1.,-0.1648165689203));
#29450=CARTESIAN_POINT('Ctrl Pts',(-1.96816512678,1.,-0.16347818545776));
#29451=CARTESIAN_POINT('Ctrl Pts',(-1.97406280235204,1.,-0.162079693556302));
#29452=CARTESIAN_POINT('Ctrl Pts',(-1.97996195437557,1.,-0.16062206078461));
#29453=CARTESIAN_POINT('Ctrl Pts',(-1.98584238283279,1.,-0.159106226437289));
#29454=CARTESIAN_POINT('Ctrl Pts',(-1.99169810931893,1.,-0.157533331459215));
#29455=CARTESIAN_POINT('Ctrl Pts',(-1.99753284771487,1.,-0.155904629548775));
#29456=CARTESIAN_POINT('Ctrl Pts',(-2.00335565310539,1.,-0.154221403049719));
#29457=CARTESIAN_POINT('Ctrl Pts',(-2.00917680318426,1.,-0.152484883621452));
#29458=CARTESIAN_POINT('Ctrl Pts',(-2.01500291940243,1.,-0.150696157673084));
#29459=CARTESIAN_POINT('Ctrl Pts',(-2.02083464969897,1.,-0.148856124775343));
#29460=CARTESIAN_POINT('Ctrl Pts',(-2.02666926182017,1.,-0.146965557332586));
#29461=CARTESIAN_POINT('Ctrl Pts',(-2.03250223739941,1.,-0.145025140186058));
#29462=CARTESIAN_POINT('Ctrl Pts',(-2.03832911025913,1.,-0.143035515058208));
#29463=CARTESIAN_POINT('Ctrl Pts',(-2.04414757947919,1.,-0.140997332152545));
#29464=CARTESIAN_POINT('Ctrl Pts',(-2.04995762001333,1.,-0.138911255368966));
#29465=CARTESIAN_POINT('Ctrl Pts',(-2.0557604441427,1.,-0.136777941218044));
#29466=CARTESIAN_POINT('Ctrl Pts',(-2.06155781517844,1.,-0.134598026192107));
#29467=CARTESIAN_POINT('Ctrl Pts',(-2.06735123910319,1.,-0.13237211154771));
#29468=CARTESIAN_POINT('Ctrl Pts',(-2.07314114713047,1.,-0.130100748328401));
#29469=CARTESIAN_POINT('Ctrl Pts',(-2.07892715110967,1.,-0.127784445276116));
#29470=CARTESIAN_POINT('Ctrl Pts',(-2.08470840653628,1.,-0.125423679412058));
#29471=CARTESIAN_POINT('Ctrl Pts',(-2.09048392424826,1.,-0.123018905621083));
#29472=CARTESIAN_POINT('Ctrl Pts',(-2.09625292867756,1.,-0.120570567965129));
#29473=CARTESIAN_POINT('Ctrl Pts',(-2.10201512132945,1.,-0.118079107988368));
#29474=CARTESIAN_POINT('Ctrl Pts',(-2.10777050261359,1.,-0.11554495768794));
#29475=CARTESIAN_POINT('Ctrl Pts',(-2.11351924490335,1.,-0.112968534419746));
#29476=CARTESIAN_POINT('Ctrl Pts',(-2.11926155590849,1.,-0.11035023613502));
#29477=CARTESIAN_POINT('Ctrl Pts',(-2.12499752306927,1.,-0.107690435231068));
#29478=CARTESIAN_POINT('Ctrl Pts',(-2.1307270488718,1.,-0.104989479152703));
#29479=CARTESIAN_POINT('Ctrl Pts',(-2.13644992667052,1.,-0.102247700556064));
#29480=CARTESIAN_POINT('Ctrl Pts',(-2.14216588395974,1.,-0.0994654261990744));
#29481=CARTESIAN_POINT('Ctrl Pts',(-2.14787463531864,1.,-0.096642985230569));
#29482=CARTESIAN_POINT('Ctrl Pts',(-2.15357593978377,1.,-0.0937807218868346));
#29483=CARTESIAN_POINT('Ctrl Pts',(-2.15926961544808,1.,-0.0908789888108267));
#29484=CARTESIAN_POINT('Ctrl Pts',(-2.16495552645275,1.,-0.0879381291387824));
#29485=CARTESIAN_POINT('Ctrl Pts',(-2.17063357871031,1.,-0.0849584620835644));
#29486=CARTESIAN_POINT('Ctrl Pts',(-2.1763037121106,1.,-0.0819402680871941));
#29487=CARTESIAN_POINT('Ctrl Pts',(-2.18196589448304,1.,-0.0788837727683229));
#29488=CARTESIAN_POINT('Ctrl Pts',(-2.1876201139874,1.,-0.0757891465833413));
#29489=CARTESIAN_POINT('Ctrl Pts',(-2.19213712012956,1.,-0.0732830357304277));
#29490=CARTESIAN_POINT('Ctrl Pts',(-2.19552129483562,1.,-0.0713863779524629));
#29491=CARTESIAN_POINT('Ctrl Pts',(-2.19777582085261,1.,-0.0701143536324927));
#29492=CARTESIAN_POINT('Ctrl Pts',(-2.19890268624765,1.,-0.0694764450219585));
#29493=CARTESIAN_POINT('',(-1.74236521665491,0.,-0.163289472382896));
#29494=CARTESIAN_POINT('Origin',(0.,0.,0.));
#29495=CARTESIAN_POINT('',(-1.7075470150345,1.,-0.383122945602004));
#29496=CARTESIAN_POINT('Origin',(0.,1.,0.));
#29497=CARTESIAN_POINT('',(-1.7075470150345,0.,-0.383122945602004));
#29498=CARTESIAN_POINT('Ctrl Pts',(-2.11275013067528,-1.,-0.61342227326009));
#29499=CARTESIAN_POINT('Ctrl Pts',(-2.11275013067528,1.,-0.61342227326009));
#29500=CARTESIAN_POINT('Ctrl Pts',(-2.11187554260142,-1.,-0.61246736556225));
#29501=CARTESIAN_POINT('Ctrl Pts',(-2.11187554260142,1.,-0.61246736556225));
#29502=CARTESIAN_POINT('Ctrl Pts',(-2.11012443807661,-1.,-0.610560911691113));
#29503=CARTESIAN_POINT('Ctrl Pts',(-2.11012443807661,1.,-0.610560911691113));
#29504=CARTESIAN_POINT('Ctrl Pts',(-2.10749199615859,-1.,-0.607711315456826));
#29505=CARTESIAN_POINT('Ctrl Pts',(-2.10749199615859,1.,-0.607711315456826));
#29506=CARTESIAN_POINT('Ctrl Pts',(-2.10397049887709,-1.,-0.603932030738212));
#29507=CARTESIAN_POINT('Ctrl Pts',(-2.10397049887709,1.,-0.603932030738212));
#29508=CARTESIAN_POINT('Ctrl Pts',(-2.09954930865331,-1.,-0.599241616422144));
#29509=CARTESIAN_POINT('Ctrl Pts',(-2.09954930865331,1.,-0.599241616422144));
#29510=CARTESIAN_POINT('Ctrl Pts',(-2.09510876220501,-1.,-0.594585006052823));
#29511=CARTESIAN_POINT('Ctrl Pts',(-2.09510876220501,1.,-0.594585006052823));
#29512=CARTESIAN_POINT('Ctrl Pts',(-2.09064881812053,-1.,-0.589962365403189));
#29513=CARTESIAN_POINT('Ctrl Pts',(-2.09064881812053,1.,-0.589962365403189));
#29514=CARTESIAN_POINT('Ctrl Pts',(-2.086169437277,-1.,-0.585373918990895));
#29515=CARTESIAN_POINT('Ctrl Pts',(-2.086169437277,1.,-0.585373918990895));
#29516=CARTESIAN_POINT('Ctrl Pts',(-2.08167059018138,-1.,-0.580819952107257));
#29517=CARTESIAN_POINT('Ctrl Pts',(-2.08167059018138,1.,-0.580819952107257));
#29518=CARTESIAN_POINT('Ctrl Pts',(-2.07715226767361,-1.,-0.576300797416274));
#29519=CARTESIAN_POINT('Ctrl Pts',(-2.07715226767361,1.,-0.576300797416274));
#29520=CARTESIAN_POINT('Ctrl Pts',(-2.07261449292757,-1.,-0.571816823242411));
#29521=CARTESIAN_POINT('Ctrl Pts',(-2.07261449292757,1.,-0.571816823242411));
#29522=CARTESIAN_POINT('Ctrl Pts',(-2.06805732997383,-1.,-0.567368421181229));
#29523=CARTESIAN_POINT('Ctrl Pts',(-2.06805732997383,1.,-0.567368421181229));
#29524=CARTESIAN_POINT('Ctrl Pts',(-2.06348090160697,-1.,-0.562955993082574));
#29525=CARTESIAN_POINT('Ctrl Pts',(-2.06348090160697,1.,-0.562955993082574));
#29526=CARTESIAN_POINT('Ctrl Pts',(-2.05888537756571,-1.,-0.558579940185467));
#29527=CARTESIAN_POINT('Ctrl Pts',(-2.05888537756571,1.,-0.558579940185467));
#29528=CARTESIAN_POINT('Ctrl Pts',(-2.05427091604482,-1.,-0.554240657464109));
#29529=CARTESIAN_POINT('Ctrl Pts',(-2.05427091604482,1.,-0.554240657464109));
#29530=CARTESIAN_POINT('Ctrl Pts',(-2.04963761077974,-1.,-0.549938525150342));
#29531=CARTESIAN_POINT('Ctrl Pts',(-2.04963761077974,1.,-0.549938525150342));
#29532=CARTESIAN_POINT('Ctrl Pts',(-2.0449854471456,-1.,-0.545673903817348));
#29533=CARTESIAN_POINT('Ctrl Pts',(-2.0449854471456,1.,-0.545673903817348));
#29534=CARTESIAN_POINT('Ctrl Pts',(-2.0403142269048,-1.,-0.54144712061552));
#29535=CARTESIAN_POINT('Ctrl Pts',(-2.0403142269048,1.,-0.54144712061552));
#29536=CARTESIAN_POINT('Ctrl Pts',(-2.03562362953993,-1.,-0.537258489833134));
#29537=CARTESIAN_POINT('Ctrl Pts',(-2.03562362953993,1.,-0.537258489833134));
#29538=CARTESIAN_POINT('Ctrl Pts',(-2.03091336214401,-1.,-0.533108355132905));
#29539=CARTESIAN_POINT('Ctrl Pts',(-2.03091336214401,1.,-0.533108355132905));
#29540=CARTESIAN_POINT('Ctrl Pts',(-2.02618329083289,-1.,-0.52899712724191));
#29541=CARTESIAN_POINT('Ctrl Pts',(-2.02618329083289,1.,-0.52899712724191));
#29542=CARTESIAN_POINT('Ctrl Pts',(-2.02143356304712,-1.,-0.524925318333518));
#29543=CARTESIAN_POINT('Ctrl Pts',(-2.02143356304712,1.,-0.524925318333518));
#29544=CARTESIAN_POINT('Ctrl Pts',(-2.01666477917305,-1.,-0.520893590399428));
#29545=CARTESIAN_POINT('Ctrl Pts',(-2.01666477917305,1.,-0.520893590399428));
#29546=CARTESIAN_POINT('Ctrl Pts',(-2.01187773939257,-1.,-0.516902681728733));
#29547=CARTESIAN_POINT('Ctrl Pts',(-2.01187773939257,1.,-0.516902681728733));
#29548=CARTESIAN_POINT('Ctrl Pts',(-2.00707309946955,-1.,-0.512953306961813));
#29549=CARTESIAN_POINT('Ctrl Pts',(-2.00707309946955,1.,-0.512953306961813));
#29550=CARTESIAN_POINT('Ctrl Pts',(-2.00225107134733,-1.,-0.509046069886152));
#29551=CARTESIAN_POINT('Ctrl Pts',(-2.00225107134733,1.,-0.509046069886152));
#29552=CARTESIAN_POINT('Ctrl Pts',(-1.99741107463567,-1.,-0.505181361323011));
#29553=CARTESIAN_POINT('Ctrl Pts',(-1.99741107463567,1.,-0.505181361323011));
#29554=CARTESIAN_POINT('Ctrl Pts',(-1.9925514912615,-1.,-0.501359287727129));
#29555=CARTESIAN_POINT('Ctrl Pts',(-1.9925514912615,1.,-0.501359287727129));
#29556=CARTESIAN_POINT('Ctrl Pts',(-1.98767044752929,-1.,-0.497579909545564));
#29557=CARTESIAN_POINT('Ctrl Pts',(-1.98767044752929,1.,-0.497579909545564));
#29558=CARTESIAN_POINT('Ctrl Pts',(-1.9827665876182,-1.,-0.493843476541492));
#29559=CARTESIAN_POINT('Ctrl Pts',(-1.9827665876182,1.,-0.493843476541492));
#29560=CARTESIAN_POINT('Ctrl Pts',(-1.97783973019229,-1.,-0.490150627860955));
#29561=CARTESIAN_POINT('Ctrl Pts',(-1.97783973019229,1.,-0.490150627860955));
#29562=CARTESIAN_POINT('Ctrl Pts',(-1.97289186263272,-1.,-0.486502692907661));
#29563=CARTESIAN_POINT('Ctrl Pts',(-1.97289186263272,1.,-0.486502692907661));
#29564=CARTESIAN_POINT('Ctrl Pts',(-1.96792703422358,-1.,-0.482901662120686));
#29565=CARTESIAN_POINT('Ctrl Pts',(-1.96792703422358,1.,-0.482901662120686));
#29566=CARTESIAN_POINT('Ctrl Pts',(-1.96294933055938,-1.,-0.479349583074846));
#29567=CARTESIAN_POINT('Ctrl Pts',(-1.96294933055938,1.,-0.479349583074846));
#29568=CARTESIAN_POINT('Ctrl Pts',(-1.95796111148175,-1.,-0.475848034683171));
#29569=CARTESIAN_POINT('Ctrl Pts',(-1.95796111148175,1.,-0.475848034683171));
#29570=CARTESIAN_POINT('Ctrl Pts',(-1.95296148278136,-1.,-0.472397672264079));
#29571=CARTESIAN_POINT('Ctrl Pts',(-1.95296148278136,1.,-0.472397672264079));
#29572=CARTESIAN_POINT('Ctrl Pts',(-1.94794381136524,-1.,-0.468997482913158));
#29573=CARTESIAN_POINT('Ctrl Pts',(-1.94794381136524,1.,-0.468997482913158));
#29574=CARTESIAN_POINT('Ctrl Pts',(-1.94289794196205,-1.,-0.465645462026064));
#29575=CARTESIAN_POINT('Ctrl Pts',(-1.94289794196205,1.,-0.465645462026064));
#29576=CARTESIAN_POINT('Ctrl Pts',(-1.93781486640834,-1.,-0.462340031009087));
#29577=CARTESIAN_POINT('Ctrl Pts',(-1.93781486640834,1.,-0.462340031009087));
#29578=CARTESIAN_POINT('Ctrl Pts',(-1.93269066517936,-1.,-0.459081234547931));
#29579=CARTESIAN_POINT('Ctrl Pts',(-1.93269066517936,1.,-0.459081234547931));
#29580=CARTESIAN_POINT('Ctrl Pts',(-1.92753067150461,-1.,-0.455872005174335));
#29581=CARTESIAN_POINT('Ctrl Pts',(-1.92753067150461,1.,-0.455872005174335));
#29582=CARTESIAN_POINT('Ctrl Pts',(-1.9223538064847,-1.,-0.452719478359356));
#29583=CARTESIAN_POINT('Ctrl Pts',(-1.9223538064847,1.,-0.452719478359356));
#29584=CARTESIAN_POINT('Ctrl Pts',(-1.91718342555717,-1.,-0.449632260106572));
#29585=CARTESIAN_POINT('Ctrl Pts',(-1.91718342555717,1.,-0.449632260106572));
#29586=CARTESIAN_POINT('Ctrl Pts',(-1.91203699981095,-1.,-0.446617343485651));
#29587=CARTESIAN_POINT('Ctrl Pts',(-1.91203699981095,1.,-0.446617343485651));
#29588=CARTESIAN_POINT('Ctrl Pts',(-1.90691756144906,-1.,-0.44367755684917));
#29589=CARTESIAN_POINT('Ctrl Pts',(-1.90691756144906,1.,-0.44367755684917));
#29590=CARTESIAN_POINT('Ctrl Pts',(-1.90180124389137,-1.,-0.44080783370416));
#29591=CARTESIAN_POINT('Ctrl Pts',(-1.90180124389137,1.,-0.44080783370416));
#29592=CARTESIAN_POINT('Ctrl Pts',(-1.89663648956549,-1.,-0.437995003948443));
#29593=CARTESIAN_POINT('Ctrl Pts',(-1.89663648956549,1.,-0.437995003948443));
#29594=CARTESIAN_POINT('Ctrl Pts',(-1.89136993975585,-1.,-0.43522566096358));
#29595=CARTESIAN_POINT('Ctrl Pts',(-1.89136993975585,1.,-0.43522566096358));
#29596=CARTESIAN_POINT('Ctrl Pts',(-1.88596913666828,-1.,-0.432493038548833));
#29597=CARTESIAN_POINT('Ctrl Pts',(-1.88596913666828,1.,-0.432493038548833));
#29598=CARTESIAN_POINT('Ctrl Pts',(-1.88044229001778,-1.,-0.429803062482217));
#29599=CARTESIAN_POINT('Ctrl Pts',(-1.88044229001778,1.,-0.429803062482217));
#29600=CARTESIAN_POINT('Ctrl Pts',(-1.87486989291333,-1.,-0.427183828518743));
#29601=CARTESIAN_POINT('Ctrl Pts',(-1.87486989291333,1.,-0.427183828518743));
#29602=CARTESIAN_POINT('Ctrl Pts',(-1.8693780394412,-1.,-0.424678177290876));
#29603=CARTESIAN_POINT('Ctrl Pts',(-1.8693780394412,1.,-0.424678177290876));
#29604=CARTESIAN_POINT('Ctrl Pts',(-1.86408083333863,-1.,-0.422327307417884));
#29605=CARTESIAN_POINT('Ctrl Pts',(-1.86408083333863,1.,-0.422327307417884));
#29606=CARTESIAN_POINT('Ctrl Pts',(-1.8590328109667,-1.,-0.420157287975583));
#29607=CARTESIAN_POINT('Ctrl Pts',(-1.8590328109667,1.,-0.420157287975583));
#29608=CARTESIAN_POINT('Ctrl Pts',(-1.8541763285645,-1.,-0.418164129144045));
#29609=CARTESIAN_POINT('Ctrl Pts',(-1.8541763285645,1.,-0.418164129144045));
#29610=CARTESIAN_POINT('Ctrl Pts',(-1.84929312930314,-1.,-0.416300022039885));
#29611=CARTESIAN_POINT('Ctrl Pts',(-1.84929312930314,1.,-0.416300022039885));
#29612=CARTESIAN_POINT('Ctrl Pts',(-1.84405757074218,-1.,-0.414487438255542));
#29613=CARTESIAN_POINT('Ctrl Pts',(-1.84405757074218,1.,-0.414487438255542));
#29614=CARTESIAN_POINT('Ctrl Pts',(-1.8380895347617,-1.,-0.412633125322945));
#29615=CARTESIAN_POINT('Ctrl Pts',(-1.8380895347617,1.,-0.412633125322945));
#29616=CARTESIAN_POINT('Ctrl Pts',(-1.83100408895047,-1.,-0.410641256301276));
#29617=CARTESIAN_POINT('Ctrl Pts',(-1.83100408895047,1.,-0.410641256301276));
#29618=CARTESIAN_POINT('Ctrl Pts',(-1.82247022677562,-1.,-0.408428948106227));
#29619=CARTESIAN_POINT('Ctrl Pts',(-1.82247022677562,1.,-0.408428948106227));
#29620=CARTESIAN_POINT('Ctrl Pts',(-1.81223801812013,-1.,-0.405933518407175));
#29621=CARTESIAN_POINT('Ctrl Pts',(-1.81223801812013,1.,-0.405933518407175));
#29622=CARTESIAN_POINT('Ctrl Pts',(-1.80012077173238,-1.,-0.403107976163396));
#29623=CARTESIAN_POINT('Ctrl Pts',(-1.80012077173238,1.,-0.403107976163396));
#29624=CARTESIAN_POINT('Ctrl Pts',(-1.78598826343754,-1.,-0.399919403774155));
#29625=CARTESIAN_POINT('Ctrl Pts',(-1.78598826343754,1.,-0.399919403774155));
#29626=CARTESIAN_POINT('Ctrl Pts',(-1.76975560043442,-1.,-0.396346196110688));
#29627=CARTESIAN_POINT('Ctrl Pts',(-1.76975560043442,1.,-0.396346196110688));
#29628=CARTESIAN_POINT('Ctrl Pts',(-1.75137405310193,-1.,-0.392375812285395));
#29629=CARTESIAN_POINT('Ctrl Pts',(-1.75137405310193,1.,-0.392375812285395));
#29630=CARTESIAN_POINT('Ctrl Pts',(-1.73493170972829,-1.,-0.388877023502615));
#29631=CARTESIAN_POINT('Ctrl Pts',(-1.73493170972829,1.,-0.388877023502615));
#29632=CARTESIAN_POINT('Ctrl Pts',(-1.72162022244582,-1.,-0.386070790323281));
#29633=CARTESIAN_POINT('Ctrl Pts',(-1.72162022244582,1.,-0.386070790323281));
#29634=CARTESIAN_POINT('Ctrl Pts',(-1.71231062891398,-1.,-0.384119047314215));
#29635=CARTESIAN_POINT('Ctrl Pts',(-1.71231062891398,1.,-0.384119047314215));
#29636=CARTESIAN_POINT('Ctrl Pts',(-1.7075470150345,-1.,-0.383122945602004));
#29637=CARTESIAN_POINT('Ctrl Pts',(-1.7075470150345,1.,-0.383122945602004));
#29638=CARTESIAN_POINT('',(-2.11275013067528,1.,-0.61342227326009));
#29639=CARTESIAN_POINT('Ctrl Pts',(-2.11275013067528,1.,-0.61342227326009));
#29640=CARTESIAN_POINT('Ctrl Pts',(-2.11187554260142,1.,-0.61246736556225));
#29641=CARTESIAN_POINT('Ctrl Pts',(-2.11012443807661,1.,-0.610560911691113));
#29642=CARTESIAN_POINT('Ctrl Pts',(-2.10749199615859,1.,-0.607711315456826));
#29643=CARTESIAN_POINT('Ctrl Pts',(-2.10397049887709,1.,-0.603932030738212));
#29644=CARTESIAN_POINT('Ctrl Pts',(-2.09954930865331,1.,-0.599241616422144));
#29645=CARTESIAN_POINT('Ctrl Pts',(-2.09510876220501,1.,-0.594585006052823));
#29646=CARTESIAN_POINT('Ctrl Pts',(-2.09064881812053,1.,-0.589962365403189));
#29647=CARTESIAN_POINT('Ctrl Pts',(-2.086169437277,1.,-0.585373918990895));
#29648=CARTESIAN_POINT('Ctrl Pts',(-2.08167059018138,1.,-0.580819952107257));
#29649=CARTESIAN_POINT('Ctrl Pts',(-2.07715226767361,1.,-0.576300797416274));
#29650=CARTESIAN_POINT('Ctrl Pts',(-2.07261449292757,1.,-0.571816823242411));
#29651=CARTESIAN_POINT('Ctrl Pts',(-2.06805732997383,1.,-0.567368421181229));
#29652=CARTESIAN_POINT('Ctrl Pts',(-2.06348090160697,1.,-0.562955993082574));
#29653=CARTESIAN_POINT('Ctrl Pts',(-2.05888537756571,1.,-0.558579940185467));
#29654=CARTESIAN_POINT('Ctrl Pts',(-2.05427091604482,1.,-0.554240657464109));
#29655=CARTESIAN_POINT('Ctrl Pts',(-2.04963761077974,1.,-0.549938525150342));
#29656=CARTESIAN_POINT('Ctrl Pts',(-2.0449854471456,1.,-0.545673903817348));
#29657=CARTESIAN_POINT('Ctrl Pts',(-2.0403142269048,1.,-0.54144712061552));
#29658=CARTESIAN_POINT('Ctrl Pts',(-2.03562362953993,1.,-0.537258489833134));
#29659=CARTESIAN_POINT('Ctrl Pts',(-2.03091336214401,1.,-0.533108355132905));
#29660=CARTESIAN_POINT('Ctrl Pts',(-2.02618329083289,1.,-0.52899712724191));
#29661=CARTESIAN_POINT('Ctrl Pts',(-2.02143356304712,1.,-0.524925318333518));
#29662=CARTESIAN_POINT('Ctrl Pts',(-2.01666477917305,1.,-0.520893590399428));
#29663=CARTESIAN_POINT('Ctrl Pts',(-2.01187773939257,1.,-0.516902681728733));
#29664=CARTESIAN_POINT('Ctrl Pts',(-2.00707309946955,1.,-0.512953306961813));
#29665=CARTESIAN_POINT('Ctrl Pts',(-2.00225107134733,1.,-0.509046069886152));
#29666=CARTESIAN_POINT('Ctrl Pts',(-1.99741107463567,1.,-0.505181361323011));
#29667=CARTESIAN_POINT('Ctrl Pts',(-1.9925514912615,1.,-0.501359287727129));
#29668=CARTESIAN_POINT('Ctrl Pts',(-1.98767044752929,1.,-0.497579909545564));
#29669=CARTESIAN_POINT('Ctrl Pts',(-1.9827665876182,1.,-0.493843476541492));
#29670=CARTESIAN_POINT('Ctrl Pts',(-1.97783973019229,1.,-0.490150627860955));
#29671=CARTESIAN_POINT('Ctrl Pts',(-1.97289186263272,1.,-0.486502692907661));
#29672=CARTESIAN_POINT('Ctrl Pts',(-1.96792703422358,1.,-0.482901662120686));
#29673=CARTESIAN_POINT('Ctrl Pts',(-1.96294933055938,1.,-0.479349583074846));
#29674=CARTESIAN_POINT('Ctrl Pts',(-1.95796111148175,1.,-0.475848034683171));
#29675=CARTESIAN_POINT('Ctrl Pts',(-1.95296148278136,1.,-0.472397672264079));
#29676=CARTESIAN_POINT('Ctrl Pts',(-1.94794381136524,1.,-0.468997482913158));
#29677=CARTESIAN_POINT('Ctrl Pts',(-1.94289794196205,1.,-0.465645462026064));
#29678=CARTESIAN_POINT('Ctrl Pts',(-1.93781486640834,1.,-0.462340031009087));
#29679=CARTESIAN_POINT('Ctrl Pts',(-1.93269066517936,1.,-0.459081234547931));
#29680=CARTESIAN_POINT('Ctrl Pts',(-1.92753067150461,1.,-0.455872005174335));
#29681=CARTESIAN_POINT('Ctrl Pts',(-1.9223538064847,1.,-0.452719478359356));
#29682=CARTESIAN_POINT('Ctrl Pts',(-1.91718342555717,1.,-0.449632260106572));
#29683=CARTESIAN_POINT('Ctrl Pts',(-1.91203699981095,1.,-0.446617343485651));
#29684=CARTESIAN_POINT('Ctrl Pts',(-1.90691756144906,1.,-0.44367755684917));
#29685=CARTESIAN_POINT('Ctrl Pts',(-1.90180124389137,1.,-0.44080783370416));
#29686=CARTESIAN_POINT('Ctrl Pts',(-1.89663648956549,1.,-0.437995003948443));
#29687=CARTESIAN_POINT('Ctrl Pts',(-1.89136993975585,1.,-0.43522566096358));
#29688=CARTESIAN_POINT('Ctrl Pts',(-1.88596913666828,1.,-0.432493038548833));
#29689=CARTESIAN_POINT('Ctrl Pts',(-1.88044229001778,1.,-0.429803062482217));
#29690=CARTESIAN_POINT('Ctrl Pts',(-1.87486989291333,1.,-0.427183828518743));
#29691=CARTESIAN_POINT('Ctrl Pts',(-1.8693780394412,1.,-0.424678177290876));
#29692=CARTESIAN_POINT('Ctrl Pts',(-1.86408083333863,1.,-0.422327307417884));
#29693=CARTESIAN_POINT('Ctrl Pts',(-1.8590328109667,1.,-0.420157287975583));
#29694=CARTESIAN_POINT('Ctrl Pts',(-1.8541763285645,1.,-0.418164129144045));
#29695=CARTESIAN_POINT('Ctrl Pts',(-1.84929312930314,1.,-0.416300022039885));
#29696=CARTESIAN_POINT('Ctrl Pts',(-1.84405757074218,1.,-0.414487438255542));
#29697=CARTESIAN_POINT('Ctrl Pts',(-1.8380895347617,1.,-0.412633125322945));
#29698=CARTESIAN_POINT('Ctrl Pts',(-1.83100408895047,1.,-0.410641256301276));
#29699=CARTESIAN_POINT('Ctrl Pts',(-1.82247022677562,1.,-0.408428948106227));
#29700=CARTESIAN_POINT('Ctrl Pts',(-1.81223801812013,1.,-0.405933518407175));
#29701=CARTESIAN_POINT('Ctrl Pts',(-1.80012077173238,1.,-0.403107976163396));
#29702=CARTESIAN_POINT('Ctrl Pts',(-1.78598826343754,1.,-0.399919403774155));
#29703=CARTESIAN_POINT('Ctrl Pts',(-1.76975560043442,1.,-0.396346196110688));
#29704=CARTESIAN_POINT('Ctrl Pts',(-1.75137405310193,1.,-0.392375812285395));
#29705=CARTESIAN_POINT('Ctrl Pts',(-1.73493170972829,1.,-0.388877023502615));
#29706=CARTESIAN_POINT('Ctrl Pts',(-1.72162022244582,1.,-0.386070790323281));
#29707=CARTESIAN_POINT('Ctrl Pts',(-1.71231062891398,1.,-0.384119047314215));
#29708=CARTESIAN_POINT('Ctrl Pts',(-1.7075470150345,1.,-0.383122945602004));
#29709=CARTESIAN_POINT('',(-2.11275013067528,0.,-0.61342227326009));
#29710=CARTESIAN_POINT('Origin',(-2.0698113262342,0.,-0.745574324794401));
#29711=CARTESIAN_POINT('',(-2.0698113262342,1.,-0.745574324794401));
#29712=CARTESIAN_POINT('',(-2.11275013067528,1.,-0.61342227326009));
#29713=CARTESIAN_POINT('',(-2.0698113262342,0.,-0.745574324794401));
#29714=CARTESIAN_POINT('Ctrl Pts',(-1.60662857109684,-1.,-0.693717979106306));
#29715=CARTESIAN_POINT('Ctrl Pts',(-1.60662857109684,1.,-0.693717979106306));
#29716=CARTESIAN_POINT('Ctrl Pts',(-1.61106790958151,-1.,-0.695712097881194));
#29717=CARTESIAN_POINT('Ctrl Pts',(-1.61106790958151,1.,-0.695712097881194));
#29718=CARTESIAN_POINT('Ctrl Pts',(-1.61974673472612,-1.,-0.699605146405088));
#29719=CARTESIAN_POINT('Ctrl Pts',(-1.61974673472612,1.,-0.699605146405088));
#29720=CARTESIAN_POINT('Ctrl Pts',(-1.63216541664676,-1.,-0.705159151988319));
#29721=CARTESIAN_POINT('Ctrl Pts',(-1.63216541664676,1.,-0.705159151988319));
#29722=CARTESIAN_POINT('Ctrl Pts',(-1.64752408832016,-1.,-0.711993139355394));
#29723=CARTESIAN_POINT('Ctrl Pts',(-1.64752408832016,1.,-0.711993139355394));
#29724=CARTESIAN_POINT('Ctrl Pts',(-1.6647288055568,-1.,-0.719585433804282));
#29725=CARTESIAN_POINT('Ctrl Pts',(-1.6647288055568,1.,-0.719585433804282));
#29726=CARTESIAN_POINT('Ctrl Pts',(-1.67996158455503,-1.,-0.726235967997433));
#29727=CARTESIAN_POINT('Ctrl Pts',(-1.67996158455503,1.,-0.726235967997433));
#29728=CARTESIAN_POINT('Ctrl Pts',(-1.69326921975743,-1.,-0.731963238697195));
#29729=CARTESIAN_POINT('Ctrl Pts',(-1.69326921975743,1.,-0.731963238697195));
#29730=CARTESIAN_POINT('Ctrl Pts',(-1.70473309006121,-1.,-0.736799665724771));
#29731=CARTESIAN_POINT('Ctrl Pts',(-1.70473309006121,1.,-0.736799665724771));
#29732=CARTESIAN_POINT('Ctrl Pts',(-1.71447789751927,-1.,-0.740795162032087));
#29733=CARTESIAN_POINT('Ctrl Pts',(-1.71447789751927,1.,-0.740795162032087));
#29734=CARTESIAN_POINT('Ctrl Pts',(-1.7226822991693,-1.,-0.744021445433764));
#29735=CARTESIAN_POINT('Ctrl Pts',(-1.7226822991693,1.,-0.744021445433764));
#29736=CARTESIAN_POINT('Ctrl Pts',(-1.72958533647399,-1.,-0.746574710096436));
#29737=CARTESIAN_POINT('Ctrl Pts',(-1.72958533647399,1.,-0.746574710096436));
#29738=CARTESIAN_POINT('Ctrl Pts',(-1.73550351679848,-1.,-0.748582462954854));
#29739=CARTESIAN_POINT('Ctrl Pts',(-1.73550351679848,1.,-0.748582462954854));
#29740=CARTESIAN_POINT('Ctrl Pts',(-1.74080458266705,-1.,-0.75019343597954));
#29741=CARTESIAN_POINT('Ctrl Pts',(-1.74080458266705,1.,-0.75019343597954));
#29742=CARTESIAN_POINT('Ctrl Pts',(-1.74585086852298,-1.,-0.751555614163629));
#29743=CARTESIAN_POINT('Ctrl Pts',(-1.74585086852298,1.,-0.751555614163629));
#29744=CARTESIAN_POINT('Ctrl Pts',(-1.75095139468809,-1.,-0.752797683531377));
#29745=CARTESIAN_POINT('Ctrl Pts',(-1.75095139468809,1.,-0.752797683531377));
#29746=CARTESIAN_POINT('Ctrl Pts',(-1.75631083600175,-1.,-0.75400925402848));
#29747=CARTESIAN_POINT('Ctrl Pts',(-1.75631083600175,1.,-0.75400925402848));
#29748=CARTESIAN_POINT('Ctrl Pts',(-1.7619781724032,-1.,-0.755220979975262));
#29749=CARTESIAN_POINT('Ctrl Pts',(-1.7619781724032,1.,-0.755220979975262));
#29750=CARTESIAN_POINT('Ctrl Pts',(-1.76789396003141,-1.,-0.756421896028403));
#29751=CARTESIAN_POINT('Ctrl Pts',(-1.76789396003141,1.,-0.756421896028403));
#29752=CARTESIAN_POINT('Ctrl Pts',(-1.77394167108342,-1.,-0.757578264077238));
#29753=CARTESIAN_POINT('Ctrl Pts',(-1.77394167108342,1.,-0.757578264077238));
#29754=CARTESIAN_POINT('Ctrl Pts',(-1.77999411220912,-1.,-0.75865062667738));
#29755=CARTESIAN_POINT('Ctrl Pts',(-1.77999411220912,1.,-0.75865062667738));
#29756=CARTESIAN_POINT('Ctrl Pts',(-1.78596964884526,-1.,-0.759614401109868));
#29757=CARTESIAN_POINT('Ctrl Pts',(-1.78596964884526,1.,-0.759614401109868));
#29758=CARTESIAN_POINT('Ctrl Pts',(-1.79185815610802,-1.,-0.760469555880425));
#29759=CARTESIAN_POINT('Ctrl Pts',(-1.79185815610802,1.,-0.760469555880425));
#29760=CARTESIAN_POINT('Ctrl Pts',(-1.79768986997735,-1.,-0.761229695230359));
#29761=CARTESIAN_POINT('Ctrl Pts',(-1.79768986997735,1.,-0.761229695230359));
#29762=CARTESIAN_POINT('Ctrl Pts',(-1.80351583877334,-1.,-0.761915336443515));
#29763=CARTESIAN_POINT('Ctrl Pts',(-1.80351583877334,1.,-0.761915336443515));
#29764=CARTESIAN_POINT('Ctrl Pts',(-1.80938551463989,-1.,-0.762546129464036));
#29765=CARTESIAN_POINT('Ctrl Pts',(-1.80938551463989,1.,-0.762546129464036));
#29766=CARTESIAN_POINT('Ctrl Pts',(-1.81532118405566,-1.,-0.763132003836783));
#29767=CARTESIAN_POINT('Ctrl Pts',(-1.81532118405566,1.,-0.763132003836783));
#29768=CARTESIAN_POINT('Ctrl Pts',(-1.82131873145297,-1.,-0.763673465462854));
#29769=CARTESIAN_POINT('Ctrl Pts',(-1.82131873145297,1.,-0.763673465462854));
#29770=CARTESIAN_POINT('Ctrl Pts',(-1.8273599120008,-1.,-0.764165902606055));
#29771=CARTESIAN_POINT('Ctrl Pts',(-1.8273599120008,1.,-0.764165902606055));
#29772=CARTESIAN_POINT('Ctrl Pts',(-1.8334207722714,-1.,-0.764602549687845));
#29773=CARTESIAN_POINT('Ctrl Pts',(-1.8334207722714,1.,-0.764602549687845));
#29774=CARTESIAN_POINT('Ctrl Pts',(-1.83948181064823,-1.,-0.764978057881687));
#29775=CARTESIAN_POINT('Ctrl Pts',(-1.83948181064823,1.,-0.764978057881687));
#29776=CARTESIAN_POINT('Ctrl Pts',(-1.8455369887591,-1.,-0.765291664861971));
#29777=CARTESIAN_POINT('Ctrl Pts',(-1.8455369887591,1.,-0.765291664861971));
#29778=CARTESIAN_POINT('Ctrl Pts',(-1.85158945130054,-1.,-0.765545710619023));
#29779=CARTESIAN_POINT('Ctrl Pts',(-1.85158945130054,1.,-0.765545710619023));
#29780=CARTESIAN_POINT('Ctrl Pts',(-1.85764741390391,-1.,-0.765744212909305));
#29781=CARTESIAN_POINT('Ctrl Pts',(-1.85764741390391,1.,-0.765744212909305));
#29782=CARTESIAN_POINT('Ctrl Pts',(-1.86372027063314,-1.,-0.765891519092557));
#29783=CARTESIAN_POINT('Ctrl Pts',(-1.86372027063314,1.,-0.765891519092557));
#29784=CARTESIAN_POINT('Ctrl Pts',(-1.86981398314345,-1.,-0.765990708546111));
#29785=CARTESIAN_POINT('Ctrl Pts',(-1.86981398314345,1.,-0.765990708546111));
#29786=CARTESIAN_POINT('Ctrl Pts',(-1.87592888967886,-1.,-0.766042837036759));
#29787=CARTESIAN_POINT('Ctrl Pts',(-1.87592888967886,1.,-0.766042837036759));
#29788=CARTESIAN_POINT('Ctrl Pts',(-1.88206215302561,-1.,-0.766047794851868));
#29789=CARTESIAN_POINT('Ctrl Pts',(-1.88206215302561,1.,-0.766047794851868));
#29790=CARTESIAN_POINT('Ctrl Pts',(-1.88820926433409,-1.,-0.76600483706209));
#29791=CARTESIAN_POINT('Ctrl Pts',(-1.88820926433409,1.,-0.76600483706209));
#29792=CARTESIAN_POINT('Ctrl Pts',(-1.89436577771389,-1.,-0.765913193856979));
#29793=CARTESIAN_POINT('Ctrl Pts',(-1.89436577771389,1.,-0.765913193856979));
#29794=CARTESIAN_POINT('Ctrl Pts',(-1.90052930393599,-1.,-0.765772772593395));
#29795=CARTESIAN_POINT('Ctrl Pts',(-1.90052930393599,1.,-0.765772772593395));
#29796=CARTESIAN_POINT('Ctrl Pts',(-1.90669961402362,-1.,-0.765584196937936));
#29797=CARTESIAN_POINT('Ctrl Pts',(-1.90669961402362,1.,-0.765584196937936));
#29798=CARTESIAN_POINT('Ctrl Pts',(-1.91287765805174,-1.,-0.765348465884739));
#29799=CARTESIAN_POINT('Ctrl Pts',(-1.91287765805174,1.,-0.765348465884739));
#29800=CARTESIAN_POINT('Ctrl Pts',(-1.91906491634197,-1.,-0.765066729667095));
#29801=CARTESIAN_POINT('Ctrl Pts',(-1.91906491634197,1.,-0.765066729667095));
#29802=CARTESIAN_POINT('Ctrl Pts',(-1.92526263537041,-1.,-0.764740025488189));
#29803=CARTESIAN_POINT('Ctrl Pts',(-1.92526263537041,1.,-0.764740025488189));
#29804=CARTESIAN_POINT('Ctrl Pts',(-1.93147105496367,-1.,-0.764369010673889));
#29805=CARTESIAN_POINT('Ctrl Pts',(-1.93147105496367,1.,-0.764369010673889));
#29806=CARTESIAN_POINT('Ctrl Pts',(-1.93768964875867,-1.,-0.763954049121393));
#29807=CARTESIAN_POINT('Ctrl Pts',(-1.93768964875867,1.,-0.763954049121393));
#29808=CARTESIAN_POINT('Ctrl Pts',(-1.94391746617626,-1.,-0.76349533353858));
#29809=CARTESIAN_POINT('Ctrl Pts',(-1.94391746617626,1.,-0.76349533353858));
#29810=CARTESIAN_POINT('Ctrl Pts',(-1.95015342590025,-1.,-0.762992990878774));
#29811=CARTESIAN_POINT('Ctrl Pts',(-1.95015342590025,1.,-0.762992990878774));
#29812=CARTESIAN_POINT('Ctrl Pts',(-1.95639665309893,-1.,-0.762447203806263));
#29813=CARTESIAN_POINT('Ctrl Pts',(-1.95639665309893,1.,-0.762447203806263));
#29814=CARTESIAN_POINT('Ctrl Pts',(-1.96264672744229,-1.,-0.761858300014575));
#29815=CARTESIAN_POINT('Ctrl Pts',(-1.96264672744229,1.,-0.761858300014575));
#29816=CARTESIAN_POINT('Ctrl Pts',(-1.96890351582545,-1.,-0.761226690483986));
#29817=CARTESIAN_POINT('Ctrl Pts',(-1.96890351582545,1.,-0.761226690483986));
#29818=CARTESIAN_POINT('Ctrl Pts',(-1.97516705321521,-1.,-0.760552825409855));
#29819=CARTESIAN_POINT('Ctrl Pts',(-1.97516705321521,1.,-0.760552825409855));
#29820=CARTESIAN_POINT('Ctrl Pts',(-1.98143741418156,-1.,-0.759837147452135));
#29821=CARTESIAN_POINT('Ctrl Pts',(-1.98143741418156,1.,-0.759837147452135));
#29822=CARTESIAN_POINT('Ctrl Pts',(-1.98771456680806,-1.,-0.759080037802242));
#29823=CARTESIAN_POINT('Ctrl Pts',(-1.98771456680806,1.,-0.759080037802242));
#29824=CARTESIAN_POINT('Ctrl Pts',(-1.9939983109871,-1.,-0.758281796766377));
#29825=CARTESIAN_POINT('Ctrl Pts',(-1.9939983109871,1.,-0.758281796766377));
#29826=CARTESIAN_POINT('Ctrl Pts',(-2.00028834739072,-1.,-0.757442676862341));
#29827=CARTESIAN_POINT('Ctrl Pts',(-2.00028834739072,1.,-0.757442676862341));
#29828=CARTESIAN_POINT('Ctrl Pts',(-2.00658431587682,-1.,-0.756562904646496));
#29829=CARTESIAN_POINT('Ctrl Pts',(-2.00658431587682,1.,-0.756562904646496));
#29830=CARTESIAN_POINT('Ctrl Pts',(-2.01288584328149,-1.,-0.7556427049581));
#29831=CARTESIAN_POINT('Ctrl Pts',(-2.01288584328149,1.,-0.7556427049581));
#29832=CARTESIAN_POINT('Ctrl Pts',(-2.01919259406003,-1.,-0.75468233072352));
#29833=CARTESIAN_POINT('Ctrl Pts',(-2.01919259406003,1.,-0.75468233072352));
#29834=CARTESIAN_POINT('Ctrl Pts',(-2.02550428623587,-1.,-0.753682061113765));
#29835=CARTESIAN_POINT('Ctrl Pts',(-2.02550428623587,1.,-0.753682061113765));
#29836=CARTESIAN_POINT('Ctrl Pts',(-2.03182068456467,-1.,-0.752642180488104));
#29837=CARTESIAN_POINT('Ctrl Pts',(-2.03182068456467,1.,-0.752642180488104));
#29838=CARTESIAN_POINT('Ctrl Pts',(-2.03814160092173,-1.,-0.751562963361383));
#29839=CARTESIAN_POINT('Ctrl Pts',(-2.03814160092173,1.,-0.751562963361383));
#29840=CARTESIAN_POINT('Ctrl Pts',(-2.04446689147754,-1.,-0.750444657874758));
#29841=CARTESIAN_POINT('Ctrl Pts',(-2.04446689147754,1.,-0.750444657874758));
#29842=CARTESIAN_POINT('Ctrl Pts',(-2.05079645591606,-1.,-0.749287468663053));
#29843=CARTESIAN_POINT('Ctrl Pts',(-2.05079645591606,1.,-0.749287468663053));
#29844=CARTESIAN_POINT('Ctrl Pts',(-2.05713023030263,-1.,-0.748091554181101));
#29845=CARTESIAN_POINT('Ctrl Pts',(-2.05713023030263,1.,-0.748091554181101));
#29846=CARTESIAN_POINT('Ctrl Pts',(-2.06220058927162,-1.,-0.747103932785504));
#29847=CARTESIAN_POINT('Ctrl Pts',(-2.06220058927162,1.,-0.747103932785504));
#29848=CARTESIAN_POINT('Ctrl Pts',(-2.06600523016401,-1.,-0.746345871542695));
#29849=CARTESIAN_POINT('Ctrl Pts',(-2.06600523016401,1.,-0.746345871542695));
#29850=CARTESIAN_POINT('Ctrl Pts',(-2.06854248895575,-1.,-0.74583279137781));
#29851=CARTESIAN_POINT('Ctrl Pts',(-2.06854248895575,1.,-0.74583279137781));
#29852=CARTESIAN_POINT('Ctrl Pts',(-2.0698113262342,-1.,-0.745574324794401));
#29853=CARTESIAN_POINT('Ctrl Pts',(-2.0698113262342,1.,-0.745574324794401));
#29854=CARTESIAN_POINT('',(-1.60662857109684,1.,-0.693717979106306));
#29855=CARTESIAN_POINT('Ctrl Pts',(-1.60662857109684,1.,-0.693717979106306));
#29856=CARTESIAN_POINT('Ctrl Pts',(-1.61106790958151,1.,-0.695712097881194));
#29857=CARTESIAN_POINT('Ctrl Pts',(-1.61974673472612,1.,-0.699605146405088));
#29858=CARTESIAN_POINT('Ctrl Pts',(-1.63216541664676,1.,-0.705159151988319));
#29859=CARTESIAN_POINT('Ctrl Pts',(-1.64752408832016,1.,-0.711993139355394));
#29860=CARTESIAN_POINT('Ctrl Pts',(-1.6647288055568,1.,-0.719585433804282));
#29861=CARTESIAN_POINT('Ctrl Pts',(-1.67996158455503,1.,-0.726235967997433));
#29862=CARTESIAN_POINT('Ctrl Pts',(-1.69326921975743,1.,-0.731963238697195));
#29863=CARTESIAN_POINT('Ctrl Pts',(-1.70473309006121,1.,-0.736799665724771));
#29864=CARTESIAN_POINT('Ctrl Pts',(-1.71447789751927,1.,-0.740795162032087));
#29865=CARTESIAN_POINT('Ctrl Pts',(-1.7226822991693,1.,-0.744021445433764));
#29866=CARTESIAN_POINT('Ctrl Pts',(-1.72958533647399,1.,-0.746574710096436));
#29867=CARTESIAN_POINT('Ctrl Pts',(-1.73550351679848,1.,-0.748582462954854));
#29868=CARTESIAN_POINT('Ctrl Pts',(-1.74080458266705,1.,-0.75019343597954));
#29869=CARTESIAN_POINT('Ctrl Pts',(-1.74585086852298,1.,-0.751555614163629));
#29870=CARTESIAN_POINT('Ctrl Pts',(-1.75095139468809,1.,-0.752797683531377));
#29871=CARTESIAN_POINT('Ctrl Pts',(-1.75631083600175,1.,-0.75400925402848));
#29872=CARTESIAN_POINT('Ctrl Pts',(-1.7619781724032,1.,-0.755220979975262));
#29873=CARTESIAN_POINT('Ctrl Pts',(-1.76789396003141,1.,-0.756421896028403));
#29874=CARTESIAN_POINT('Ctrl Pts',(-1.77394167108342,1.,-0.757578264077238));
#29875=CARTESIAN_POINT('Ctrl Pts',(-1.77999411220912,1.,-0.75865062667738));
#29876=CARTESIAN_POINT('Ctrl Pts',(-1.78596964884526,1.,-0.759614401109868));
#29877=CARTESIAN_POINT('Ctrl Pts',(-1.79185815610802,1.,-0.760469555880425));
#29878=CARTESIAN_POINT('Ctrl Pts',(-1.79768986997735,1.,-0.761229695230359));
#29879=CARTESIAN_POINT('Ctrl Pts',(-1.80351583877334,1.,-0.761915336443515));
#29880=CARTESIAN_POINT('Ctrl Pts',(-1.80938551463989,1.,-0.762546129464036));
#29881=CARTESIAN_POINT('Ctrl Pts',(-1.81532118405566,1.,-0.763132003836783));
#29882=CARTESIAN_POINT('Ctrl Pts',(-1.82131873145297,1.,-0.763673465462854));
#29883=CARTESIAN_POINT('Ctrl Pts',(-1.8273599120008,1.,-0.764165902606055));
#29884=CARTESIAN_POINT('Ctrl Pts',(-1.8334207722714,1.,-0.764602549687845));
#29885=CARTESIAN_POINT('Ctrl Pts',(-1.83948181064823,1.,-0.764978057881687));
#29886=CARTESIAN_POINT('Ctrl Pts',(-1.8455369887591,1.,-0.765291664861971));
#29887=CARTESIAN_POINT('Ctrl Pts',(-1.85158945130054,1.,-0.765545710619023));
#29888=CARTESIAN_POINT('Ctrl Pts',(-1.85764741390391,1.,-0.765744212909305));
#29889=CARTESIAN_POINT('Ctrl Pts',(-1.86372027063314,1.,-0.765891519092557));
#29890=CARTESIAN_POINT('Ctrl Pts',(-1.86981398314345,1.,-0.765990708546111));
#29891=CARTESIAN_POINT('Ctrl Pts',(-1.87592888967886,1.,-0.766042837036759));
#29892=CARTESIAN_POINT('Ctrl Pts',(-1.88206215302561,1.,-0.766047794851868));
#29893=CARTESIAN_POINT('Ctrl Pts',(-1.88820926433409,1.,-0.76600483706209));
#29894=CARTESIAN_POINT('Ctrl Pts',(-1.89436577771389,1.,-0.765913193856979));
#29895=CARTESIAN_POINT('Ctrl Pts',(-1.90052930393599,1.,-0.765772772593395));
#29896=CARTESIAN_POINT('Ctrl Pts',(-1.90669961402362,1.,-0.765584196937936));
#29897=CARTESIAN_POINT('Ctrl Pts',(-1.91287765805174,1.,-0.765348465884739));
#29898=CARTESIAN_POINT('Ctrl Pts',(-1.91906491634197,1.,-0.765066729667095));
#29899=CARTESIAN_POINT('Ctrl Pts',(-1.92526263537041,1.,-0.764740025488189));
#29900=CARTESIAN_POINT('Ctrl Pts',(-1.93147105496367,1.,-0.764369010673889));
#29901=CARTESIAN_POINT('Ctrl Pts',(-1.93768964875867,1.,-0.763954049121393));
#29902=CARTESIAN_POINT('Ctrl Pts',(-1.94391746617626,1.,-0.76349533353858));
#29903=CARTESIAN_POINT('Ctrl Pts',(-1.95015342590025,1.,-0.762992990878774));
#29904=CARTESIAN_POINT('Ctrl Pts',(-1.95639665309893,1.,-0.762447203806263));
#29905=CARTESIAN_POINT('Ctrl Pts',(-1.96264672744229,1.,-0.761858300014575));
#29906=CARTESIAN_POINT('Ctrl Pts',(-1.96890351582545,1.,-0.761226690483986));
#29907=CARTESIAN_POINT('Ctrl Pts',(-1.97516705321521,1.,-0.760552825409855));
#29908=CARTESIAN_POINT('Ctrl Pts',(-1.98143741418156,1.,-0.759837147452135));
#29909=CARTESIAN_POINT('Ctrl Pts',(-1.98771456680806,1.,-0.759080037802242));
#29910=CARTESIAN_POINT('Ctrl Pts',(-1.9939983109871,1.,-0.758281796766377));
#29911=CARTESIAN_POINT('Ctrl Pts',(-2.00028834739072,1.,-0.757442676862341));
#29912=CARTESIAN_POINT('Ctrl Pts',(-2.00658431587682,1.,-0.756562904646496));
#29913=CARTESIAN_POINT('Ctrl Pts',(-2.01288584328149,1.,-0.7556427049581));
#29914=CARTESIAN_POINT('Ctrl Pts',(-2.01919259406003,1.,-0.75468233072352));
#29915=CARTESIAN_POINT('Ctrl Pts',(-2.02550428623587,1.,-0.753682061113765));
#29916=CARTESIAN_POINT('Ctrl Pts',(-2.03182068456467,1.,-0.752642180488104));
#29917=CARTESIAN_POINT('Ctrl Pts',(-2.03814160092173,1.,-0.751562963361383));
#29918=CARTESIAN_POINT('Ctrl Pts',(-2.04446689147754,1.,-0.750444657874758));
#29919=CARTESIAN_POINT('Ctrl Pts',(-2.05079645591606,1.,-0.749287468663053));
#29920=CARTESIAN_POINT('Ctrl Pts',(-2.05713023030263,1.,-0.748091554181101));
#29921=CARTESIAN_POINT('Ctrl Pts',(-2.06220058927162,1.,-0.747103932785504));
#29922=CARTESIAN_POINT('Ctrl Pts',(-2.06600523016401,1.,-0.746345871542695));
#29923=CARTESIAN_POINT('Ctrl Pts',(-2.06854248895575,1.,-0.74583279137781));
#29924=CARTESIAN_POINT('Ctrl Pts',(-2.0698113262342,1.,-0.745574324794401));
#29925=CARTESIAN_POINT('',(-1.60662857109684,0.,-0.693717979106306));
#29926=CARTESIAN_POINT('Origin',(0.,0.,0.));
#29927=CARTESIAN_POINT('',(-1.5055822144029,1.,-0.892032620296855));
#29928=CARTESIAN_POINT('Origin',(0.,1.,0.));
#29929=CARTESIAN_POINT('',(-1.5055822144029,0.,-0.892032620296855));
#29930=CARTESIAN_POINT('Ctrl Pts',(-1.81978687191668,-1.,-1.23627494547115));
#29931=CARTESIAN_POINT('Ctrl Pts',(-1.81978687191668,1.,-1.23627494547115));
#29932=CARTESIAN_POINT('Ctrl Pts',(-1.81925017193666,-1.,-1.23509651170476));
#29933=CARTESIAN_POINT('Ctrl Pts',(-1.81925017193666,1.,-1.23509651170476));
#29934=CARTESIAN_POINT('Ctrl Pts',(-1.81817389921279,-1.,-1.2327422452705));
#29935=CARTESIAN_POINT('Ctrl Pts',(-1.81817389921279,1.,-1.2327422452705));
#29936=CARTESIAN_POINT('Ctrl Pts',(-1.8165508718364,-1.,-1.2292186489137));
#29937=CARTESIAN_POINT('Ctrl Pts',(-1.8165508718364,1.,-1.2292186489137));
#29938=CARTESIAN_POINT('Ctrl Pts',(-1.81436959210434,-1.,-1.2245361330495));
#29939=CARTESIAN_POINT('Ctrl Pts',(-1.81436959210434,1.,-1.2245361330495));
#29940=CARTESIAN_POINT('Ctrl Pts',(-1.81161420806656,-1.,-1.21870906103557));
#29941=CARTESIAN_POINT('Ctrl Pts',(-1.81161420806656,1.,-1.21870906103557));
#29942=CARTESIAN_POINT('Ctrl Pts',(-1.80882996917129,-1.,-1.21290815708314));
#29943=CARTESIAN_POINT('Ctrl Pts',(-1.80882996917129,1.,-1.21290815708314));
#29944=CARTESIAN_POINT('Ctrl Pts',(-1.80601678480707,-1.,-1.20713356605475));
#29945=CARTESIAN_POINT('Ctrl Pts',(-1.80601678480707,1.,-1.20713356605475));
#29946=CARTESIAN_POINT('Ctrl Pts',(-1.80317454838603,-1.,-1.20138548938974));
#29947=CARTESIAN_POINT('Ctrl Pts',(-1.80317454838603,1.,-1.20138548938974));
#29948=CARTESIAN_POINT('Ctrl Pts',(-1.80030314369879,-1.,-1.19566418930242));
#29949=CARTESIAN_POINT('Ctrl Pts',(-1.80030314369879,1.,-1.19566418930242));
#29950=CARTESIAN_POINT('Ctrl Pts',(-1.79740245923478,-1.,-1.18996997934445));
#29951=CARTESIAN_POINT('Ctrl Pts',(-1.79740245923478,1.,-1.18996997934445));
#29952=CARTESIAN_POINT('Ctrl Pts',(-1.79447240321515,-1.,-1.18430321697432));
#29953=CARTESIAN_POINT('Ctrl Pts',(-1.79447240321515,1.,-1.18430321697432));
#29954=CARTESIAN_POINT('Ctrl Pts',(-1.79151291552689,-1.,-1.17866429440809));
#29955=CARTESIAN_POINT('Ctrl Pts',(-1.79151291552689,1.,-1.17866429440809));
#29956=CARTESIAN_POINT('Ctrl Pts',(-1.78852398877616,-1.,-1.17305363177328));
#29957=CARTESIAN_POINT('Ctrl Pts',(-1.78852398877616,1.,-1.17305363177328));
#29958=CARTESIAN_POINT('Ctrl Pts',(-1.78550566040443,-1.,-1.16747166312303));
#29959=CARTESIAN_POINT('Ctrl Pts',(-1.78550566040443,1.,-1.16747166312303));
#29960=CARTESIAN_POINT('Ctrl Pts',(-1.78245795881009,-1.,-1.16191881298499));
#29961=CARTESIAN_POINT('Ctrl Pts',(-1.78245795881009,1.,-1.16191881298499));
#29962=CARTESIAN_POINT('Ctrl Pts',(-1.77938085564275,-1.,-1.15639547194698));
#29963=CARTESIAN_POINT('Ctrl Pts',(-1.77938085564275,1.,-1.15639547194698));
#29964=CARTESIAN_POINT('Ctrl Pts',(-1.7762742255701,-1.,-1.15090197841515));
#29965=CARTESIAN_POINT('Ctrl Pts',(-1.7762742255701,1.,-1.15090197841515));
#29966=CARTESIAN_POINT('Ctrl Pts',(-1.77313777896194,-1.,-1.1454385822692));
#29967=CARTESIAN_POINT('Ctrl Pts',(-1.77313777896194,1.,-1.1454385822692));
#29968=CARTESIAN_POINT('Ctrl Pts',(-1.76997111386769,-1.,-1.14000548336975));
#29969=CARTESIAN_POINT('Ctrl Pts',(-1.76997111386769,1.,-1.14000548336975));
#29970=CARTESIAN_POINT('Ctrl Pts',(-1.76677384551862,-1.,-1.1346029180462));
#29971=CARTESIAN_POINT('Ctrl Pts',(-1.76677384551862,1.,-1.1346029180462));
#29972=CARTESIAN_POINT('Ctrl Pts',(-1.7635457196617,-1.,-1.12923123555075));
#29973=CARTESIAN_POINT('Ctrl Pts',(-1.7635457196617,1.,-1.12923123555075));
#29974=CARTESIAN_POINT('Ctrl Pts',(-1.76028671825096,-1.,-1.12389096855086));
#29975=CARTESIAN_POINT('Ctrl Pts',(-1.76028671825096,1.,-1.12389096855086));
#29976=CARTESIAN_POINT('Ctrl Pts',(-1.75699720772105,-1.,-1.11858293216763));
#29977=CARTESIAN_POINT('Ctrl Pts',(-1.75699720772105,1.,-1.11858293216763));
#29978=CARTESIAN_POINT('Ctrl Pts',(-1.7536777209463,-1.,-1.11330807582551));
#29979=CARTESIAN_POINT('Ctrl Pts',(-1.7536777209463,1.,-1.11330807582551));
#29980=CARTESIAN_POINT('Ctrl Pts',(-1.7503286607592,-1.,-1.10806728183007));
#29981=CARTESIAN_POINT('Ctrl Pts',(-1.7503286607592,1.,-1.10806728183007));
#29982=CARTESIAN_POINT('Ctrl Pts',(-1.74695004214923,-1.,-1.10286118991143));
#29983=CARTESIAN_POINT('Ctrl Pts',(-1.74695004214923,1.,-1.10286118991143));
#29984=CARTESIAN_POINT('Ctrl Pts',(-1.74354119236208,-1.,-1.09768999241225));
#29985=CARTESIAN_POINT('Ctrl Pts',(-1.74354119236208,1.,-1.09768999241225));
#29986=CARTESIAN_POINT('Ctrl Pts',(-1.74010053962247,-1.,-1.09255329056493));
#29987=CARTESIAN_POINT('Ctrl Pts',(-1.74010053962247,1.,-1.09255329056493));
#29988=CARTESIAN_POINT('Ctrl Pts',(-1.73662628326091,-1.,-1.08745056285427));
#29989=CARTESIAN_POINT('Ctrl Pts',(-1.73662628326091,1.,-1.08745056285427));
#29990=CARTESIAN_POINT('Ctrl Pts',(-1.73311705663407,-1.,-1.08238162784749));
#29991=CARTESIAN_POINT('Ctrl Pts',(-1.73311705663407,1.,-1.08238162784749));
#29992=CARTESIAN_POINT('Ctrl Pts',(-1.72957248977424,-1.,-1.0773470373727));
#29993=CARTESIAN_POINT('Ctrl Pts',(-1.72957248977424,1.,-1.0773470373727));
#29994=CARTESIAN_POINT('Ctrl Pts',(-1.72599406198488,-1.,-1.07234866990252));
#29995=CARTESIAN_POINT('Ctrl Pts',(-1.72599406198488,1.,-1.07234866990252));
#29996=CARTESIAN_POINT('Ctrl Pts',(-1.72238500928453,-1.,-1.06738966975462));
#29997=CARTESIAN_POINT('Ctrl Pts',(-1.72238500928453,1.,-1.06738966975462));
#29998=CARTESIAN_POINT('Ctrl Pts',(-1.71874858456904,-1.,-1.06247324680647));
#29999=CARTESIAN_POINT('Ctrl Pts',(-1.71874858456904,1.,-1.06247324680647));
#30000=CARTESIAN_POINT('Ctrl Pts',(-1.7150865442702,-1.,-1.05760163192479));
#30001=CARTESIAN_POINT('Ctrl Pts',(-1.7150865442702,1.,-1.05760163192479));
#30002=CARTESIAN_POINT('Ctrl Pts',(-1.71139783543989,-1.,-1.05277517202855));
#30003=CARTESIAN_POINT('Ctrl Pts',(-1.71139783543989,1.,-1.05277517202855));
#30004=CARTESIAN_POINT('Ctrl Pts',(-1.70767646263649,-1.,-1.04799085404995));
#30005=CARTESIAN_POINT('Ctrl Pts',(-1.70767646263649,1.,-1.04799085404995));
#30006=CARTESIAN_POINT('Ctrl Pts',(-1.70391338707982,-1.,-1.04324363334554));
#30007=CARTESIAN_POINT('Ctrl Pts',(-1.70391338707982,1.,-1.04324363334554));
#30008=CARTESIAN_POINT('Ctrl Pts',(-1.70010052930962,-1.,-1.03852922490789));
#30009=CARTESIAN_POINT('Ctrl Pts',(-1.70010052930962,1.,-1.03852922490789));
#30010=CARTESIAN_POINT('Ctrl Pts',(-1.69623414782771,-1.,-1.03384646003588));
#30011=CARTESIAN_POINT('Ctrl Pts',(-1.69623414782771,1.,-1.03384646003588));
#30012=CARTESIAN_POINT('Ctrl Pts',(-1.69231840863458,-1.,-1.02919977579147));
#30013=CARTESIAN_POINT('Ctrl Pts',(-1.69231840863458,1.,-1.02919977579147));
#30014=CARTESIAN_POINT('Ctrl Pts',(-1.68836910178447,-1.,-1.02460180535255));
#30015=CARTESIAN_POINT('Ctrl Pts',(-1.68836910178447,1.,-1.02460180535255));
#30016=CARTESIAN_POINT('Ctrl Pts',(-1.68440578021706,-1.,-1.02006795074201));
#30017=CARTESIAN_POINT('Ctrl Pts',(-1.68440578021706,1.,-1.02006795074201));
#30018=CARTESIAN_POINT('Ctrl Pts',(-1.68044289894798,-1.,-1.01561026162773));
#30019=CARTESIAN_POINT('Ctrl Pts',(-1.68044289894798,1.,-1.01561026162773));
#30020=CARTESIAN_POINT('Ctrl Pts',(-1.67648246776464,-1.,-1.01123236493511));
#30021=CARTESIAN_POINT('Ctrl Pts',(-1.67648246776464,1.,-1.01123236493511));
#30022=CARTESIAN_POINT('Ctrl Pts',(-1.67250335383293,-1.,-1.00692206696414));
#30023=CARTESIAN_POINT('Ctrl Pts',(-1.67250335383293,1.,-1.00692206696414));
#30024=CARTESIAN_POINT('Ctrl Pts',(-1.66846059277303,-1.,-1.00265091003727));
#30025=CARTESIAN_POINT('Ctrl Pts',(-1.66846059277303,1.,-1.00265091003727));
#30026=CARTESIAN_POINT('Ctrl Pts',(-1.66430758030376,-1.,-0.998389654952758));
#30027=CARTESIAN_POINT('Ctrl Pts',(-1.66430758030376,1.,-0.998389654952758));
#30028=CARTESIAN_POINT('Ctrl Pts',(-1.66001553809947,-1.,-0.994121836661306));
#30029=CARTESIAN_POINT('Ctrl Pts',(-1.66001553809947,1.,-0.994121836661306));
#30030=CARTESIAN_POINT('Ctrl Pts',(-1.65559044289699,-1.,-0.989855627854165));
#30031=CARTESIAN_POINT('Ctrl Pts',(-1.65559044289699,1.,-0.989855627854165));
#30032=CARTESIAN_POINT('Ctrl Pts',(-1.65110016612638,-1.,-0.985642622920821));
#30033=CARTESIAN_POINT('Ctrl Pts',(-1.65110016612638,1.,-0.985642622920821));
#30034=CARTESIAN_POINT('Ctrl Pts',(-1.64665139190656,-1.,-0.981562530939489));
#30035=CARTESIAN_POINT('Ctrl Pts',(-1.64665139190656,1.,-0.981562530939489));
#30036=CARTESIAN_POINT('Ctrl Pts',(-1.64233990826687,-1.,-0.977689794119416));
#30037=CARTESIAN_POINT('Ctrl Pts',(-1.64233990826687,1.,-0.977689794119416));
#30038=CARTESIAN_POINT('Ctrl Pts',(-1.63820952658144,-1.,-0.974066058287418));
#30039=CARTESIAN_POINT('Ctrl Pts',(-1.63820952658144,1.,-0.974066058287418));
#30040=CARTESIAN_POINT('Ctrl Pts',(-1.63420665729798,-1.,-0.970669715997509));
#30041=CARTESIAN_POINT('Ctrl Pts',(-1.63420665729798,1.,-0.970669715997509));
#30042=CARTESIAN_POINT('Ctrl Pts',(-1.63013849959461,-1.,-0.967387853230345));
#30043=CARTESIAN_POINT('Ctrl Pts',(-1.63013849959461,1.,-0.967387853230345));
#30044=CARTESIAN_POINT('Ctrl Pts',(-1.62571930670187,-1.,-0.964046107040536));
#30045=CARTESIAN_POINT('Ctrl Pts',(-1.62571930670187,1.,-0.964046107040536));
#30046=CARTESIAN_POINT('Ctrl Pts',(-1.62061638140221,-1.,-0.960438326101729));
#30047=CARTESIAN_POINT('Ctrl Pts',(-1.62061638140221,1.,-0.960438326101729));
#30048=CARTESIAN_POINT('Ctrl Pts',(-1.61449324337085,-1.,-0.956354422920671));
#30049=CARTESIAN_POINT('Ctrl Pts',(-1.61449324337085,1.,-0.956354422920671));
#30050=CARTESIAN_POINT('Ctrl Pts',(-1.60706069896936,-1.,-0.951613284356035));
#30051=CARTESIAN_POINT('Ctrl Pts',(-1.60706069896936,1.,-0.951613284356035));
#30052=CARTESIAN_POINT('Ctrl Pts',(-1.59810042043673,-1.,-0.946078063315257));
#30053=CARTESIAN_POINT('Ctrl Pts',(-1.59810042043673,1.,-0.946078063315257));
#30054=CARTESIAN_POINT('Ctrl Pts',(-1.58744937487176,-1.,-0.939646377893399));
#30055=CARTESIAN_POINT('Ctrl Pts',(-1.58744937487176,1.,-0.939646377893399));
#30056=CARTESIAN_POINT('Ctrl Pts',(-1.57499388382243,-1.,-0.932246680108685));
#30057=CARTESIAN_POINT('Ctrl Pts',(-1.57499388382243,1.,-0.932246680108685));
#30058=CARTESIAN_POINT('Ctrl Pts',(-1.56065988578893,-1.,-0.923832188944341));
#30059=CARTESIAN_POINT('Ctrl Pts',(-1.56065988578893,1.,-0.923832188944341));
#30060=CARTESIAN_POINT('Ctrl Pts',(-1.54440491149498,-1.,-0.914375919026456));
#30061=CARTESIAN_POINT('Ctrl Pts',(-1.54440491149498,1.,-0.914375919026456));
#30062=CARTESIAN_POINT('Ctrl Pts',(-1.52984849887993,-1.,-0.905967409625651));
#30063=CARTESIAN_POINT('Ctrl Pts',(-1.52984849887993,1.,-0.905967409625651));
#30064=CARTESIAN_POINT('Ctrl Pts',(-1.51805569590094,-1.,-0.899185047483511));
#30065=CARTESIAN_POINT('Ctrl Pts',(-1.51805569590094,1.,-0.899185047483511));
#30066=CARTESIAN_POINT('Ctrl Pts',(-1.50980486806688,-1.,-0.894452006964543));
#30067=CARTESIAN_POINT('Ctrl Pts',(-1.50980486806688,1.,-0.894452006964543));
#30068=CARTESIAN_POINT('Ctrl Pts',(-1.5055822144029,-1.,-0.892032620296855));
#30069=CARTESIAN_POINT('Ctrl Pts',(-1.5055822144029,1.,-0.892032620296855));
#30070=CARTESIAN_POINT('',(-1.81978687191668,1.,-1.23627494547115));
#30071=CARTESIAN_POINT('Ctrl Pts',(-1.81978687191668,1.,-1.23627494547115));
#30072=CARTESIAN_POINT('Ctrl Pts',(-1.81925017193666,1.,-1.23509651170476));
#30073=CARTESIAN_POINT('Ctrl Pts',(-1.81817389921279,1.,-1.2327422452705));
#30074=CARTESIAN_POINT('Ctrl Pts',(-1.8165508718364,1.,-1.2292186489137));
#30075=CARTESIAN_POINT('Ctrl Pts',(-1.81436959210434,1.,-1.2245361330495));
#30076=CARTESIAN_POINT('Ctrl Pts',(-1.81161420806656,1.,-1.21870906103557));
#30077=CARTESIAN_POINT('Ctrl Pts',(-1.80882996917129,1.,-1.21290815708314));
#30078=CARTESIAN_POINT('Ctrl Pts',(-1.80601678480707,1.,-1.20713356605475));
#30079=CARTESIAN_POINT('Ctrl Pts',(-1.80317454838603,1.,-1.20138548938974));
#30080=CARTESIAN_POINT('Ctrl Pts',(-1.80030314369879,1.,-1.19566418930242));
#30081=CARTESIAN_POINT('Ctrl Pts',(-1.79740245923478,1.,-1.18996997934445));
#30082=CARTESIAN_POINT('Ctrl Pts',(-1.79447240321515,1.,-1.18430321697432));
#30083=CARTESIAN_POINT('Ctrl Pts',(-1.79151291552689,1.,-1.17866429440809));
#30084=CARTESIAN_POINT('Ctrl Pts',(-1.78852398877616,1.,-1.17305363177328));
#30085=CARTESIAN_POINT('Ctrl Pts',(-1.78550566040443,1.,-1.16747166312303));
#30086=CARTESIAN_POINT('Ctrl Pts',(-1.78245795881009,1.,-1.16191881298499));
#30087=CARTESIAN_POINT('Ctrl Pts',(-1.77938085564275,1.,-1.15639547194698));
#30088=CARTESIAN_POINT('Ctrl Pts',(-1.7762742255701,1.,-1.15090197841515));
#30089=CARTESIAN_POINT('Ctrl Pts',(-1.77313777896194,1.,-1.1454385822692));
#30090=CARTESIAN_POINT('Ctrl Pts',(-1.76997111386769,1.,-1.14000548336975));
#30091=CARTESIAN_POINT('Ctrl Pts',(-1.76677384551862,1.,-1.1346029180462));
#30092=CARTESIAN_POINT('Ctrl Pts',(-1.7635457196617,1.,-1.12923123555075));
#30093=CARTESIAN_POINT('Ctrl Pts',(-1.76028671825096,1.,-1.12389096855086));
#30094=CARTESIAN_POINT('Ctrl Pts',(-1.75699720772105,1.,-1.11858293216763));
#30095=CARTESIAN_POINT('Ctrl Pts',(-1.7536777209463,1.,-1.11330807582551));
#30096=CARTESIAN_POINT('Ctrl Pts',(-1.7503286607592,1.,-1.10806728183007));
#30097=CARTESIAN_POINT('Ctrl Pts',(-1.74695004214923,1.,-1.10286118991143));
#30098=CARTESIAN_POINT('Ctrl Pts',(-1.74354119236208,1.,-1.09768999241225));
#30099=CARTESIAN_POINT('Ctrl Pts',(-1.74010053962247,1.,-1.09255329056493));
#30100=CARTESIAN_POINT('Ctrl Pts',(-1.73662628326091,1.,-1.08745056285427));
#30101=CARTESIAN_POINT('Ctrl Pts',(-1.73311705663407,1.,-1.08238162784749));
#30102=CARTESIAN_POINT('Ctrl Pts',(-1.72957248977424,1.,-1.0773470373727));
#30103=CARTESIAN_POINT('Ctrl Pts',(-1.72599406198488,1.,-1.07234866990252));
#30104=CARTESIAN_POINT('Ctrl Pts',(-1.72238500928453,1.,-1.06738966975462));
#30105=CARTESIAN_POINT('Ctrl Pts',(-1.71874858456904,1.,-1.06247324680647));
#30106=CARTESIAN_POINT('Ctrl Pts',(-1.7150865442702,1.,-1.05760163192479));
#30107=CARTESIAN_POINT('Ctrl Pts',(-1.71139783543989,1.,-1.05277517202855));
#30108=CARTESIAN_POINT('Ctrl Pts',(-1.70767646263649,1.,-1.04799085404995));
#30109=CARTESIAN_POINT('Ctrl Pts',(-1.70391338707982,1.,-1.04324363334554));
#30110=CARTESIAN_POINT('Ctrl Pts',(-1.70010052930962,1.,-1.03852922490789));
#30111=CARTESIAN_POINT('Ctrl Pts',(-1.69623414782771,1.,-1.03384646003588));
#30112=CARTESIAN_POINT('Ctrl Pts',(-1.69231840863458,1.,-1.02919977579147));
#30113=CARTESIAN_POINT('Ctrl Pts',(-1.68836910178447,1.,-1.02460180535255));
#30114=CARTESIAN_POINT('Ctrl Pts',(-1.68440578021706,1.,-1.02006795074201));
#30115=CARTESIAN_POINT('Ctrl Pts',(-1.68044289894798,1.,-1.01561026162773));
#30116=CARTESIAN_POINT('Ctrl Pts',(-1.67648246776464,1.,-1.01123236493511));
#30117=CARTESIAN_POINT('Ctrl Pts',(-1.67250335383293,1.,-1.00692206696414));
#30118=CARTESIAN_POINT('Ctrl Pts',(-1.66846059277303,1.,-1.00265091003727));
#30119=CARTESIAN_POINT('Ctrl Pts',(-1.66430758030376,1.,-0.998389654952758));
#30120=CARTESIAN_POINT('Ctrl Pts',(-1.66001553809947,1.,-0.994121836661306));
#30121=CARTESIAN_POINT('Ctrl Pts',(-1.65559044289699,1.,-0.989855627854165));
#30122=CARTESIAN_POINT('Ctrl Pts',(-1.65110016612638,1.,-0.985642622920821));
#30123=CARTESIAN_POINT('Ctrl Pts',(-1.64665139190656,1.,-0.981562530939489));
#30124=CARTESIAN_POINT('Ctrl Pts',(-1.64233990826687,1.,-0.977689794119416));
#30125=CARTESIAN_POINT('Ctrl Pts',(-1.63820952658144,1.,-0.974066058287418));
#30126=CARTESIAN_POINT('Ctrl Pts',(-1.63420665729798,1.,-0.970669715997509));
#30127=CARTESIAN_POINT('Ctrl Pts',(-1.63013849959461,1.,-0.967387853230345));
#30128=CARTESIAN_POINT('Ctrl Pts',(-1.62571930670187,1.,-0.964046107040536));
#30129=CARTESIAN_POINT('Ctrl Pts',(-1.62061638140221,1.,-0.960438326101729));
#30130=CARTESIAN_POINT('Ctrl Pts',(-1.61449324337085,1.,-0.956354422920671));
#30131=CARTESIAN_POINT('Ctrl Pts',(-1.60706069896936,1.,-0.951613284356035));
#30132=CARTESIAN_POINT('Ctrl Pts',(-1.59810042043673,1.,-0.946078063315257));
#30133=CARTESIAN_POINT('Ctrl Pts',(-1.58744937487176,1.,-0.939646377893399));
#30134=CARTESIAN_POINT('Ctrl Pts',(-1.57499388382243,1.,-0.932246680108685));
#30135=CARTESIAN_POINT('Ctrl Pts',(-1.56065988578893,1.,-0.923832188944341));
#30136=CARTESIAN_POINT('Ctrl Pts',(-1.54440491149498,1.,-0.914375919026456));
#30137=CARTESIAN_POINT('Ctrl Pts',(-1.52984849887993,1.,-0.905967409625651));
#30138=CARTESIAN_POINT('Ctrl Pts',(-1.51805569590094,1.,-0.899185047483511));
#30139=CARTESIAN_POINT('Ctrl Pts',(-1.50980486806688,1.,-0.894452006964543));
#30140=CARTESIAN_POINT('Ctrl Pts',(-1.5055822144029,1.,-0.892032620296855));
#30141=CARTESIAN_POINT('',(-1.81978687191668,0.,-1.23627494547115));
#30142=CARTESIAN_POINT('Origin',(-1.73811241238545,0.,-1.34869019493419));
#30143=CARTESIAN_POINT('',(-1.73811241238545,1.,-1.34869019493419));
#30144=CARTESIAN_POINT('',(-1.81978687191668,1.,-1.23627494547115));
#30145=CARTESIAN_POINT('',(-1.73811241238545,0.,-1.34869019493419));
#30146=CARTESIAN_POINT('Ctrl Pts',(-1.31362392696032,-1.,-1.15624053661742));
#30147=CARTESIAN_POINT('Ctrl Pts',(-1.31362392696032,1.,-1.15624053661742));
#30148=CARTESIAN_POINT('Ctrl Pts',(-1.31722977216397,-1.,-1.15950888730809));
#30149=CARTESIAN_POINT('Ctrl Pts',(-1.31722977216397,1.,-1.15950888730809));
#30150=CARTESIAN_POINT('Ctrl Pts',(-1.32428080721772,-1.,-1.16589330093588));
#30151=CARTESIAN_POINT('Ctrl Pts',(-1.32428080721772,1.,-1.16589330093588));
#30152=CARTESIAN_POINT('Ctrl Pts',(-1.33437539347008,-1.,-1.17501305789857));
#30153=CARTESIAN_POINT('Ctrl Pts',(-1.33437539347008,1.,-1.17501305789857));
#30154=CARTESIAN_POINT('Ctrl Pts',(-1.34687054001093,-1.,-1.18625865667441));
#30155=CARTESIAN_POINT('Ctrl Pts',(-1.34687054001093,1.,-1.18625865667441));
#30156=CARTESIAN_POINT('Ctrl Pts',(-1.36088705043885,-1.,-1.1987959077932));
#30157=CARTESIAN_POINT('Ctrl Pts',(-1.36088705043885,1.,-1.1987959077932));
#30158=CARTESIAN_POINT('Ctrl Pts',(-1.37331915607905,-1.,-1.20982812925645));
#30159=CARTESIAN_POINT('Ctrl Pts',(-1.37331915607905,1.,-1.20982812925645));
#30160=CARTESIAN_POINT('Ctrl Pts',(-1.38420564527715,-1.,-1.21938737280852));
#30161=CARTESIAN_POINT('Ctrl Pts',(-1.38420564527715,1.,-1.21938737280852));
#30162=CARTESIAN_POINT('Ctrl Pts',(-1.39361389568796,-1.,-1.22752961899387));
#30163=CARTESIAN_POINT('Ctrl Pts',(-1.39361389568796,1.,-1.22752961899387));
#30164=CARTESIAN_POINT('Ctrl Pts',(-1.40164708206106,-1.,-1.23434087290423));
#30165=CARTESIAN_POINT('Ctrl Pts',(-1.40164708206106,1.,-1.23434087290423));
#30166=CARTESIAN_POINT('Ctrl Pts',(-1.40845295531283,-1.,-1.23994455029534));
#30167=CARTESIAN_POINT('Ctrl Pts',(-1.40845295531283,1.,-1.23994455029534));
#30168=CARTESIAN_POINT('Ctrl Pts',(-1.41422913175179,-1.,-1.24450600513056));
#30169=CARTESIAN_POINT('Ctrl Pts',(-1.41422913175179,1.,-1.24450600513056));
#30170=CARTESIAN_POINT('Ctrl Pts',(-1.41923722596025,-1.,-1.24824430986571));
#30171=CARTESIAN_POINT('Ctrl Pts',(-1.41923722596025,1.,-1.24824430986571));
#30172=CARTESIAN_POINT('Ctrl Pts',(-1.42378102115575,-1.,-1.2514145557001));
#30173=CARTESIAN_POINT('Ctrl Pts',(-1.42378102115575,1.,-1.2514145557001));
#30174=CARTESIAN_POINT('Ctrl Pts',(-1.42815938799387,-1.,-1.25426945222639));
#30175=CARTESIAN_POINT('Ctrl Pts',(-1.42815938799387,1.,-1.25426945222639));
#30176=CARTESIAN_POINT('Ctrl Pts',(-1.43262645609691,-1.,-1.25702687965755));
#30177=CARTESIAN_POINT('Ctrl Pts',(-1.43262645609691,1.,-1.25702687965755));
#30178=CARTESIAN_POINT('Ctrl Pts',(-1.43734919180848,-1.,-1.25983531012005));
#30179=CARTESIAN_POINT('Ctrl Pts',(-1.43734919180848,1.,-1.25983531012005));
#30180=CARTESIAN_POINT('Ctrl Pts',(-1.44236470511303,-1.,-1.26273903323859));
#30181=CARTESIAN_POINT('Ctrl Pts',(-1.44236470511303,1.,-1.26273903323859));
#30182=CARTESIAN_POINT('Ctrl Pts',(-1.44761985001662,-1.,-1.26570925118868));
#30183=CARTESIAN_POINT('Ctrl Pts',(-1.44761985001662,1.,-1.26570925118868));
#30184=CARTESIAN_POINT('Ctrl Pts',(-1.45301422764247,-1.,-1.2686778680489));
#30185=CARTESIAN_POINT('Ctrl Pts',(-1.45301422764247,1.,-1.2686778680489));
#30186=CARTESIAN_POINT('Ctrl Pts',(-1.45843906294697,-1.,-1.27156805265289));
#30187=CARTESIAN_POINT('Ctrl Pts',(-1.45843906294697,1.,-1.27156805265289));
#30188=CARTESIAN_POINT('Ctrl Pts',(-1.46382431332476,-1.,-1.27433119897822));
#30189=CARTESIAN_POINT('Ctrl Pts',(-1.46382431332476,1.,-1.27433119897822));
#30190=CARTESIAN_POINT('Ctrl Pts',(-1.46916035917133,-1.,-1.27696414831089));
#30191=CARTESIAN_POINT('Ctrl Pts',(-1.46916035917133,1.,-1.27696414831089));
#30192=CARTESIAN_POINT('Ctrl Pts',(-1.4744717526707,-1.,-1.2794891824849));
#30193=CARTESIAN_POINT('Ctrl Pts',(-1.4744717526707,1.,-1.2794891824849));
#30194=CARTESIAN_POINT('Ctrl Pts',(-1.47980070347095,-1.,-1.28194158939517));
#30195=CARTESIAN_POINT('Ctrl Pts',(-1.47980070347095,1.,-1.28194158939517));
#30196=CARTESIAN_POINT('Ctrl Pts',(-1.4851881711891,-1.,-1.28435533880201));
#30197=CARTESIAN_POINT('Ctrl Pts',(-1.4851881711891,1.,-1.28435533880201));
#30198=CARTESIAN_POINT('Ctrl Pts',(-1.4906522831278,-1.,-1.2867467611644));
#30199=CARTESIAN_POINT('Ctrl Pts',(-1.4906522831278,1.,-1.2867467611644));
#30200=CARTESIAN_POINT('Ctrl Pts',(-1.49618896881754,-1.,-1.28911506584254));
#30201=CARTESIAN_POINT('Ctrl Pts',(-1.49618896881754,1.,-1.28911506584254));
#30202=CARTESIAN_POINT('Ctrl Pts',(-1.50178230149776,-1.,-1.29145022885181));
#30203=CARTESIAN_POINT('Ctrl Pts',(-1.50178230149776,1.,-1.29145022885181));
#30204=CARTESIAN_POINT('Ctrl Pts',(-1.50741159078365,-1.,-1.29373841372842));
#30205=CARTESIAN_POINT('Ctrl Pts',(-1.50741159078365,1.,-1.29373841372842));
#30206=CARTESIAN_POINT('Ctrl Pts',(-1.51305994241402,-1.,-1.29596850710509));
#30207=CARTESIAN_POINT('Ctrl Pts',(-1.51305994241402,1.,-1.29596850710509));
#30208=CARTESIAN_POINT('Ctrl Pts',(-1.51872184912724,-1.,-1.29813791800747));
#30209=CARTESIAN_POINT('Ctrl Pts',(-1.51872184912724,1.,-1.29813791800747));
#30210=CARTESIAN_POINT('Ctrl Pts',(-1.52439957861062,-1.,-1.30024984366328));
#30211=CARTESIAN_POINT('Ctrl Pts',(-1.52439957861062,1.,-1.30024984366328));
#30212=CARTESIAN_POINT('Ctrl Pts',(-1.53009970283891,-1.,-1.30231064395568));
#30213=CARTESIAN_POINT('Ctrl Pts',(-1.53009970283891,1.,-1.30231064395568));
#30214=CARTESIAN_POINT('Ctrl Pts',(-1.53582981268977,-1.,-1.30432735639489));
#30215=CARTESIAN_POINT('Ctrl Pts',(-1.53582981268977,1.,-1.30432735639489));
#30216=CARTESIAN_POINT('Ctrl Pts',(-1.54159462645432,-1.,-1.30630475189556));
#30217=CARTESIAN_POINT('Ctrl Pts',(-1.54159462645432,1.,-1.30630475189556));
#30218=CARTESIAN_POINT('Ctrl Pts',(-1.54739413957185,-1.,-1.30824393907473));
#30219=CARTESIAN_POINT('Ctrl Pts',(-1.54739413957185,1.,-1.30824393907473));
#30220=CARTESIAN_POINT('Ctrl Pts',(-1.55322568759481,-1.,-1.31014393684222));
#30221=CARTESIAN_POINT('Ctrl Pts',(-1.55322568759481,1.,-1.31014393684222));
#30222=CARTESIAN_POINT('Ctrl Pts',(-1.55908521254821,-1.,-1.31200264341696));
#30223=CARTESIAN_POINT('Ctrl Pts',(-1.55908521254821,1.,-1.31200264341696));
#30224=CARTESIAN_POINT('Ctrl Pts',(-1.56496872402353,-1.,-1.31381795281002));
#30225=CARTESIAN_POINT('Ctrl Pts',(-1.56496872402353,1.,-1.31381795281002));
#30226=CARTESIAN_POINT('Ctrl Pts',(-1.57087397835723,-1.,-1.31558903860016));
#30227=CARTESIAN_POINT('Ctrl Pts',(-1.57087397835723,1.,-1.31558903860016));
#30228=CARTESIAN_POINT('Ctrl Pts',(-1.5768005650559,-1.,-1.31731642317187));
#30229=CARTESIAN_POINT('Ctrl Pts',(-1.5768005650559,1.,-1.31731642317187));
#30230=CARTESIAN_POINT('Ctrl Pts',(-1.58274907898834,-1.,-1.31900135021432));
#30231=CARTESIAN_POINT('Ctrl Pts',(-1.58274907898834,1.,-1.31900135021432));
#30232=CARTESIAN_POINT('Ctrl Pts',(-1.58872057258245,-1.,-1.32064537110892));
#30233=CARTESIAN_POINT('Ctrl Pts',(-1.58872057258245,1.,-1.32064537110892));
#30234=CARTESIAN_POINT('Ctrl Pts',(-1.59471591079403,-1.,-1.32224985747682));
#30235=CARTESIAN_POINT('Ctrl Pts',(-1.59471591079403,1.,-1.32224985747682));
#30236=CARTESIAN_POINT('Ctrl Pts',(-1.60073511858687,-1.,-1.32381550858256));
#30237=CARTESIAN_POINT('Ctrl Pts',(-1.60073511858687,1.,-1.32381550858256));
#30238=CARTESIAN_POINT('Ctrl Pts',(-1.60677758290954,-1.,-1.32534250785782));
#30239=CARTESIAN_POINT('Ctrl Pts',(-1.60677758290954,1.,-1.32534250785782));
#30240=CARTESIAN_POINT('Ctrl Pts',(-1.6128423401575,-1.,-1.32683074483356));
#30241=CARTESIAN_POINT('Ctrl Pts',(-1.6128423401575,1.,-1.32683074483356));
#30242=CARTESIAN_POINT('Ctrl Pts',(-1.61892832270724,-1.,-1.32828000610449));
#30243=CARTESIAN_POINT('Ctrl Pts',(-1.61892832270724,1.,-1.32828000610449));
#30244=CARTESIAN_POINT('Ctrl Pts',(-1.62503464209797,-1.,-1.3296901950568));
#30245=CARTESIAN_POINT('Ctrl Pts',(-1.62503464209797,1.,-1.3296901950568));
#30246=CARTESIAN_POINT('Ctrl Pts',(-1.63116079730923,-1.,-1.33106149345645));
#30247=CARTESIAN_POINT('Ctrl Pts',(-1.63116079730923,1.,-1.33106149345645));
#30248=CARTESIAN_POINT('Ctrl Pts',(-1.63730653475089,-1.,-1.33239425103724));
#30249=CARTESIAN_POINT('Ctrl Pts',(-1.63730653475089,1.,-1.33239425103724));
#30250=CARTESIAN_POINT('Ctrl Pts',(-1.6434717485603,-1.,-1.33368890676572));
#30251=CARTESIAN_POINT('Ctrl Pts',(-1.6434717485603,1.,-1.33368890676572));
#30252=CARTESIAN_POINT('Ctrl Pts',(-1.6496563728683,-1.,-1.33494590467993));
#30253=CARTESIAN_POINT('Ctrl Pts',(-1.6496563728683,1.,-1.33494590467993));
#30254=CARTESIAN_POINT('Ctrl Pts',(-1.65586025952593,-1.,-1.33616559745172));
#30255=CARTESIAN_POINT('Ctrl Pts',(-1.65586025952593,1.,-1.33616559745172));
#30256=CARTESIAN_POINT('Ctrl Pts',(-1.66208312541983,-1.,-1.33734820885262));
#30257=CARTESIAN_POINT('Ctrl Pts',(-1.66208312541983,1.,-1.33734820885262));
#30258=CARTESIAN_POINT('Ctrl Pts',(-1.66832460783989,-1.,-1.33849388654388));
#30259=CARTESIAN_POINT('Ctrl Pts',(-1.66832460783989,1.,-1.33849388654388));
#30260=CARTESIAN_POINT('Ctrl Pts',(-1.67458429426086,-1.,-1.3396027347034));
#30261=CARTESIAN_POINT('Ctrl Pts',(-1.67458429426086,1.,-1.3396027347034));
#30262=CARTESIAN_POINT('Ctrl Pts',(-1.68086176030362,-1.,-1.34067485185203));
#30263=CARTESIAN_POINT('Ctrl Pts',(-1.68086176030362,1.,-1.34067485185203));
#30264=CARTESIAN_POINT('Ctrl Pts',(-1.68715660868764,-1.,-1.341710374848));
#30265=CARTESIAN_POINT('Ctrl Pts',(-1.68715660868764,1.,-1.341710374848));
#30266=CARTESIAN_POINT('Ctrl Pts',(-1.6934684849687,-1.,-1.34270948206319));
#30267=CARTESIAN_POINT('Ctrl Pts',(-1.6934684849687,1.,-1.34270948206319));
#30268=CARTESIAN_POINT('Ctrl Pts',(-1.69979707754427,-1.,-1.34367237124483));
#30269=CARTESIAN_POINT('Ctrl Pts',(-1.69979707754427,1.,-1.34367237124483));
#30270=CARTESIAN_POINT('Ctrl Pts',(-1.70614212266738,-1.,-1.34459924533831));
#30271=CARTESIAN_POINT('Ctrl Pts',(-1.70614212266738,1.,-1.34459924533831));
#30272=CARTESIAN_POINT('Ctrl Pts',(-1.71250340686822,-1.,-1.34549029589416));
#30273=CARTESIAN_POINT('Ctrl Pts',(-1.71250340686822,1.,-1.34549029589416));
#30274=CARTESIAN_POINT('Ctrl Pts',(-1.7188807715049,-1.,-1.34634568653227));
#30275=CARTESIAN_POINT('Ctrl Pts',(-1.7188807715049,1.,-1.34634568653227));
#30276=CARTESIAN_POINT('Ctrl Pts',(-1.72527410680674,-1.,-1.34716554819527));
#30277=CARTESIAN_POINT('Ctrl Pts',(-1.72527410680674,1.,-1.34716554819527));
#30278=CARTESIAN_POINT('Ctrl Pts',(-1.7304014965394,-1.,-1.34779309152035));
#30279=CARTESIAN_POINT('Ctrl Pts',(-1.7304014965394,1.,-1.34779309152035));
#30280=CARTESIAN_POINT('Ctrl Pts',(-1.73425417885907,-1.,-1.34824783112887));
#30281=CARTESIAN_POINT('Ctrl Pts',(-1.73425417885907,1.,-1.34824783112887));
#30282=CARTESIAN_POINT('Ctrl Pts',(-1.73682580585691,-1.,-1.34854391898045));
#30283=CARTESIAN_POINT('Ctrl Pts',(-1.73682580585691,1.,-1.34854391898045));
#30284=CARTESIAN_POINT('Ctrl Pts',(-1.73811241238545,-1.,-1.34869019493419));
#30285=CARTESIAN_POINT('Ctrl Pts',(-1.73811241238545,1.,-1.34869019493419));
#30286=CARTESIAN_POINT('',(-1.31362392696032,1.,-1.15624053661742));
#30287=CARTESIAN_POINT('Ctrl Pts',(-1.31362392696032,1.,-1.15624053661742));
#30288=CARTESIAN_POINT('Ctrl Pts',(-1.31722977216397,1.,-1.15950888730809));
#30289=CARTESIAN_POINT('Ctrl Pts',(-1.32428080721772,1.,-1.16589330093588));
#30290=CARTESIAN_POINT('Ctrl Pts',(-1.33437539347008,1.,-1.17501305789857));
#30291=CARTESIAN_POINT('Ctrl Pts',(-1.34687054001093,1.,-1.18625865667441));
#30292=CARTESIAN_POINT('Ctrl Pts',(-1.36088705043885,1.,-1.1987959077932));
#30293=CARTESIAN_POINT('Ctrl Pts',(-1.37331915607905,1.,-1.20982812925645));
#30294=CARTESIAN_POINT('Ctrl Pts',(-1.38420564527715,1.,-1.21938737280852));
#30295=CARTESIAN_POINT('Ctrl Pts',(-1.39361389568796,1.,-1.22752961899387));
#30296=CARTESIAN_POINT('Ctrl Pts',(-1.40164708206106,1.,-1.23434087290423));
#30297=CARTESIAN_POINT('Ctrl Pts',(-1.40845295531283,1.,-1.23994455029534));
#30298=CARTESIAN_POINT('Ctrl Pts',(-1.41422913175179,1.,-1.24450600513056));
#30299=CARTESIAN_POINT('Ctrl Pts',(-1.41923722596025,1.,-1.24824430986571));
#30300=CARTESIAN_POINT('Ctrl Pts',(-1.42378102115575,1.,-1.2514145557001));
#30301=CARTESIAN_POINT('Ctrl Pts',(-1.42815938799387,1.,-1.25426945222639));
#30302=CARTESIAN_POINT('Ctrl Pts',(-1.43262645609691,1.,-1.25702687965755));
#30303=CARTESIAN_POINT('Ctrl Pts',(-1.43734919180848,1.,-1.25983531012005));
#30304=CARTESIAN_POINT('Ctrl Pts',(-1.44236470511303,1.,-1.26273903323859));
#30305=CARTESIAN_POINT('Ctrl Pts',(-1.44761985001662,1.,-1.26570925118868));
#30306=CARTESIAN_POINT('Ctrl Pts',(-1.45301422764247,1.,-1.2686778680489));
#30307=CARTESIAN_POINT('Ctrl Pts',(-1.45843906294697,1.,-1.27156805265289));
#30308=CARTESIAN_POINT('Ctrl Pts',(-1.46382431332476,1.,-1.27433119897822));
#30309=CARTESIAN_POINT('Ctrl Pts',(-1.46916035917133,1.,-1.27696414831089));
#30310=CARTESIAN_POINT('Ctrl Pts',(-1.4744717526707,1.,-1.2794891824849));
#30311=CARTESIAN_POINT('Ctrl Pts',(-1.47980070347095,1.,-1.28194158939517));
#30312=CARTESIAN_POINT('Ctrl Pts',(-1.4851881711891,1.,-1.28435533880201));
#30313=CARTESIAN_POINT('Ctrl Pts',(-1.4906522831278,1.,-1.2867467611644));
#30314=CARTESIAN_POINT('Ctrl Pts',(-1.49618896881754,1.,-1.28911506584254));
#30315=CARTESIAN_POINT('Ctrl Pts',(-1.50178230149776,1.,-1.29145022885181));
#30316=CARTESIAN_POINT('Ctrl Pts',(-1.50741159078365,1.,-1.29373841372842));
#30317=CARTESIAN_POINT('Ctrl Pts',(-1.51305994241402,1.,-1.29596850710509));
#30318=CARTESIAN_POINT('Ctrl Pts',(-1.51872184912724,1.,-1.29813791800747));
#30319=CARTESIAN_POINT('Ctrl Pts',(-1.52439957861062,1.,-1.30024984366328));
#30320=CARTESIAN_POINT('Ctrl Pts',(-1.53009970283891,1.,-1.30231064395568));
#30321=CARTESIAN_POINT('Ctrl Pts',(-1.53582981268977,1.,-1.30432735639489));
#30322=CARTESIAN_POINT('Ctrl Pts',(-1.54159462645432,1.,-1.30630475189556));
#30323=CARTESIAN_POINT('Ctrl Pts',(-1.54739413957185,1.,-1.30824393907473));
#30324=CARTESIAN_POINT('Ctrl Pts',(-1.55322568759481,1.,-1.31014393684222));
#30325=CARTESIAN_POINT('Ctrl Pts',(-1.55908521254821,1.,-1.31200264341696));
#30326=CARTESIAN_POINT('Ctrl Pts',(-1.56496872402353,1.,-1.31381795281002));
#30327=CARTESIAN_POINT('Ctrl Pts',(-1.57087397835723,1.,-1.31558903860016));
#30328=CARTESIAN_POINT('Ctrl Pts',(-1.5768005650559,1.,-1.31731642317187));
#30329=CARTESIAN_POINT('Ctrl Pts',(-1.58274907898834,1.,-1.31900135021432));
#30330=CARTESIAN_POINT('Ctrl Pts',(-1.58872057258245,1.,-1.32064537110892));
#30331=CARTESIAN_POINT('Ctrl Pts',(-1.59471591079403,1.,-1.32224985747682));
#30332=CARTESIAN_POINT('Ctrl Pts',(-1.60073511858687,1.,-1.32381550858256));
#30333=CARTESIAN_POINT('Ctrl Pts',(-1.60677758290954,1.,-1.32534250785782));
#30334=CARTESIAN_POINT('Ctrl Pts',(-1.6128423401575,1.,-1.32683074483356));
#30335=CARTESIAN_POINT('Ctrl Pts',(-1.61892832270724,1.,-1.32828000610449));
#30336=CARTESIAN_POINT('Ctrl Pts',(-1.62503464209797,1.,-1.3296901950568));
#30337=CARTESIAN_POINT('Ctrl Pts',(-1.63116079730923,1.,-1.33106149345645));
#30338=CARTESIAN_POINT('Ctrl Pts',(-1.63730653475089,1.,-1.33239425103724));
#30339=CARTESIAN_POINT('Ctrl Pts',(-1.6434717485603,1.,-1.33368890676572));
#30340=CARTESIAN_POINT('Ctrl Pts',(-1.6496563728683,1.,-1.33494590467993));
#30341=CARTESIAN_POINT('Ctrl Pts',(-1.65586025952593,1.,-1.33616559745172));
#30342=CARTESIAN_POINT('Ctrl Pts',(-1.66208312541983,1.,-1.33734820885262));
#30343=CARTESIAN_POINT('Ctrl Pts',(-1.66832460783989,1.,-1.33849388654388));
#30344=CARTESIAN_POINT('Ctrl Pts',(-1.67458429426086,1.,-1.3396027347034));
#30345=CARTESIAN_POINT('Ctrl Pts',(-1.68086176030362,1.,-1.34067485185203));
#30346=CARTESIAN_POINT('Ctrl Pts',(-1.68715660868764,1.,-1.341710374848));
#30347=CARTESIAN_POINT('Ctrl Pts',(-1.6934684849687,1.,-1.34270948206319));
#30348=CARTESIAN_POINT('Ctrl Pts',(-1.69979707754427,1.,-1.34367237124483));
#30349=CARTESIAN_POINT('Ctrl Pts',(-1.70614212266738,1.,-1.34459924533831));
#30350=CARTESIAN_POINT('Ctrl Pts',(-1.71250340686822,1.,-1.34549029589416));
#30351=CARTESIAN_POINT('Ctrl Pts',(-1.7188807715049,1.,-1.34634568653227));
#30352=CARTESIAN_POINT('Ctrl Pts',(-1.72527410680674,1.,-1.34716554819527));
#30353=CARTESIAN_POINT('Ctrl Pts',(-1.7304014965394,1.,-1.34779309152035));
#30354=CARTESIAN_POINT('Ctrl Pts',(-1.73425417885907,1.,-1.34824783112887));
#30355=CARTESIAN_POINT('Ctrl Pts',(-1.73682580585691,1.,-1.34854391898045));
#30356=CARTESIAN_POINT('Ctrl Pts',(-1.73811241238545,1.,-1.34869019493419));
#30357=CARTESIAN_POINT('',(-1.31362392696032,0.,-1.15624053661742));
#30358=CARTESIAN_POINT('Origin',(0.,0.,0.));
#30359=CARTESIAN_POINT('',(-1.15624053661742,1.,-1.31362392696033));
#30360=CARTESIAN_POINT('Origin',(0.,1.,0.));
#30361=CARTESIAN_POINT('',(-1.15624053661742,0.,-1.31362392696033));
#30362=CARTESIAN_POINT('Ctrl Pts',(-1.34869019493419,-1.,-1.73811241238545));
#30363=CARTESIAN_POINT('Ctrl Pts',(-1.34869019493419,1.,-1.73811241238545));
#30364=CARTESIAN_POINT('Ctrl Pts',(-1.34854391898145,-1.,-1.73682580585819));
#30365=CARTESIAN_POINT('Ctrl Pts',(-1.34854391898145,1.,-1.73682580585819));
#30366=CARTESIAN_POINT('Ctrl Pts',(-1.34824783113158,-1.,-1.73425417886255));
#30367=CARTESIAN_POINT('Ctrl Pts',(-1.34824783113158,1.,-1.73425417886255));
#30368=CARTESIAN_POINT('Ctrl Pts',(-1.3477930915247,-1.,-1.73040149654497));
#30369=CARTESIAN_POINT('Ctrl Pts',(-1.3477930915247,1.,-1.73040149654497));
#30370=CARTESIAN_POINT('Ctrl Pts',(-1.34716554820013,-1.,-1.72527410681298));
#30371=CARTESIAN_POINT('Ctrl Pts',(-1.34716554820013,1.,-1.72527410681298));
#30372=CARTESIAN_POINT('Ctrl Pts',(-1.34634568653586,-1.,-1.7188807715095));
#30373=CARTESIAN_POINT('Ctrl Pts',(-1.34634568653586,1.,-1.7188807715095));
#30374=CARTESIAN_POINT('Ctrl Pts',(-1.34549029589563,-1.,-1.71250340687011));
#30375=CARTESIAN_POINT('Ctrl Pts',(-1.34549029589563,1.,-1.71250340687011));
#30376=CARTESIAN_POINT('Ctrl Pts',(-1.34459924533783,-1.,-1.70614212266676));
#30377=CARTESIAN_POINT('Ctrl Pts',(-1.34459924533783,1.,-1.70614212266676));
#30378=CARTESIAN_POINT('Ctrl Pts',(-1.34367237124322,-1.,-1.69979707754221));
#30379=CARTESIAN_POINT('Ctrl Pts',(-1.34367237124322,1.,-1.69979707754221));
#30380=CARTESIAN_POINT('Ctrl Pts',(-1.34270948206139,-1.,-1.6934684849664));
#30381=CARTESIAN_POINT('Ctrl Pts',(-1.34270948206139,1.,-1.6934684849664));
#30382=CARTESIAN_POINT('Ctrl Pts',(-1.34171037484673,-1.,-1.68715660868602));
#30383=CARTESIAN_POINT('Ctrl Pts',(-1.34171037484673,1.,-1.68715660868602));
#30384=CARTESIAN_POINT('Ctrl Pts',(-1.3406748518516,-1.,-1.68086176030308));
#30385=CARTESIAN_POINT('Ctrl Pts',(-1.3406748518516,1.,-1.68086176030308));
#30386=CARTESIAN_POINT('Ctrl Pts',(-1.33960273470372,-1.,-1.67458429426126));
#30387=CARTESIAN_POINT('Ctrl Pts',(-1.33960273470372,1.,-1.67458429426126));
#30388=CARTESIAN_POINT('Ctrl Pts',(-1.33849388654458,-1.,-1.66832460784078));
#30389=CARTESIAN_POINT('Ctrl Pts',(-1.33849388654458,1.,-1.66832460784078));
#30390=CARTESIAN_POINT('Ctrl Pts',(-1.33734820885331,-1.,-1.66208312542073));
#30391=CARTESIAN_POINT('Ctrl Pts',(-1.33734820885331,1.,-1.66208312542073));
#30392=CARTESIAN_POINT('Ctrl Pts',(-1.33616559745217,-1.,-1.65586025952651));
#30393=CARTESIAN_POINT('Ctrl Pts',(-1.33616559745217,1.,-1.65586025952651));
#30394=CARTESIAN_POINT('Ctrl Pts',(-1.33494590468003,-1.,-1.64965637286843));
#30395=CARTESIAN_POINT('Ctrl Pts',(-1.33494590468003,1.,-1.64965637286843));
#30396=CARTESIAN_POINT('Ctrl Pts',(-1.33368890676554,-1.,-1.64347174856007));
#30397=CARTESIAN_POINT('Ctrl Pts',(-1.33368890676554,1.,-1.64347174856007));
#30398=CARTESIAN_POINT('Ctrl Pts',(-1.33239425103694,-1.,-1.6373065347505));
#30399=CARTESIAN_POINT('Ctrl Pts',(-1.33239425103694,1.,-1.6373065347505));
#30400=CARTESIAN_POINT('Ctrl Pts',(-1.33106149345618,-1.,-1.63116079730887));
#30401=CARTESIAN_POINT('Ctrl Pts',(-1.33106149345618,1.,-1.63116079730887));
#30402=CARTESIAN_POINT('Ctrl Pts',(-1.32969019505665,-1.,-1.62503464209777));
#30403=CARTESIAN_POINT('Ctrl Pts',(-1.32969019505665,1.,-1.62503464209777));
#30404=CARTESIAN_POINT('Ctrl Pts',(-1.32828000610448,-1.,-1.61892832270723));
#30405=CARTESIAN_POINT('Ctrl Pts',(-1.32828000610448,1.,-1.61892832270723));
#30406=CARTESIAN_POINT('Ctrl Pts',(-1.32683074483365,-1.,-1.61284234015762));
#30407=CARTESIAN_POINT('Ctrl Pts',(-1.32683074483365,1.,-1.61284234015762));
#30408=CARTESIAN_POINT('Ctrl Pts',(-1.32534250785794,-1.,-1.6067775829097));
#30409=CARTESIAN_POINT('Ctrl Pts',(-1.32534250785794,1.,-1.6067775829097));
#30410=CARTESIAN_POINT('Ctrl Pts',(-1.32381550858266,-1.,-1.600735118587));
#30411=CARTESIAN_POINT('Ctrl Pts',(-1.32381550858266,1.,-1.600735118587));
#30412=CARTESIAN_POINT('Ctrl Pts',(-1.32224985747686,-1.,-1.59471591079408));
#30413=CARTESIAN_POINT('Ctrl Pts',(-1.32224985747686,1.,-1.59471591079408));
#30414=CARTESIAN_POINT('Ctrl Pts',(-1.32064537110891,-1.,-1.58872057258244));
#30415=CARTESIAN_POINT('Ctrl Pts',(-1.32064537110891,1.,-1.58872057258244));
#30416=CARTESIAN_POINT('Ctrl Pts',(-1.31900135021428,-1.,-1.58274907898829));
#30417=CARTESIAN_POINT('Ctrl Pts',(-1.31900135021428,1.,-1.58274907898829));
#30418=CARTESIAN_POINT('Ctrl Pts',(-1.31731642317183,-1.,-1.57680056505585));
#30419=CARTESIAN_POINT('Ctrl Pts',(-1.31731642317183,1.,-1.57680056505585));
#30420=CARTESIAN_POINT('Ctrl Pts',(-1.31558903860015,-1.,-1.57087397835721));
#30421=CARTESIAN_POINT('Ctrl Pts',(-1.31558903860015,1.,-1.57087397835721));
#30422=CARTESIAN_POINT('Ctrl Pts',(-1.31381795281002,-1.,-1.56496872402352));
#30423=CARTESIAN_POINT('Ctrl Pts',(-1.31381795281002,1.,-1.56496872402352));
#30424=CARTESIAN_POINT('Ctrl Pts',(-1.31200264341696,-1.,-1.55908521254822));
#30425=CARTESIAN_POINT('Ctrl Pts',(-1.31200264341696,1.,-1.55908521254822));
#30426=CARTESIAN_POINT('Ctrl Pts',(-1.31014393684221,-1.,-1.55322568759481));
#30427=CARTESIAN_POINT('Ctrl Pts',(-1.31014393684221,1.,-1.55322568759481));
#30428=CARTESIAN_POINT('Ctrl Pts',(-1.30824393907471,-1.,-1.54739413957183));
#30429=CARTESIAN_POINT('Ctrl Pts',(-1.30824393907471,1.,-1.54739413957183));
#30430=CARTESIAN_POINT('Ctrl Pts',(-1.30630475189553,-1.,-1.54159462645428));
#30431=CARTESIAN_POINT('Ctrl Pts',(-1.30630475189553,1.,-1.54159462645428));
#30432=CARTESIAN_POINT('Ctrl Pts',(-1.30432735639487,-1.,-1.53582981268976));
#30433=CARTESIAN_POINT('Ctrl Pts',(-1.30432735639487,1.,-1.53582981268976));
#30434=CARTESIAN_POINT('Ctrl Pts',(-1.3023106439557,-1.,-1.53009970283893));
#30435=CARTESIAN_POINT('Ctrl Pts',(-1.3023106439557,1.,-1.53009970283893));
#30436=CARTESIAN_POINT('Ctrl Pts',(-1.30024984366334,-1.,-1.5243995786107));
#30437=CARTESIAN_POINT('Ctrl Pts',(-1.30024984366334,1.,-1.5243995786107));
#30438=CARTESIAN_POINT('Ctrl Pts',(-1.29813791800757,-1.,-1.51872184912735));
#30439=CARTESIAN_POINT('Ctrl Pts',(-1.29813791800757,1.,-1.51872184912735));
#30440=CARTESIAN_POINT('Ctrl Pts',(-1.29596850710518,-1.,-1.51305994241412));
#30441=CARTESIAN_POINT('Ctrl Pts',(-1.29596850710518,1.,-1.51305994241412));
#30442=CARTESIAN_POINT('Ctrl Pts',(-1.29373841372843,-1.,-1.50741159078367));
#30443=CARTESIAN_POINT('Ctrl Pts',(-1.29373841372843,1.,-1.50741159078367));
#30444=CARTESIAN_POINT('Ctrl Pts',(-1.29145022885171,-1.,-1.50178230149764));
#30445=CARTESIAN_POINT('Ctrl Pts',(-1.29145022885171,1.,-1.50178230149764));
#30446=CARTESIAN_POINT('Ctrl Pts',(-1.28911506584232,-1.,-1.49618896881729));
#30447=CARTESIAN_POINT('Ctrl Pts',(-1.28911506584232,1.,-1.49618896881729));
#30448=CARTESIAN_POINT('Ctrl Pts',(-1.28674676116415,-1.,-1.4906522831275));
#30449=CARTESIAN_POINT('Ctrl Pts',(-1.28674676116415,1.,-1.4906522831275));
#30450=CARTESIAN_POINT('Ctrl Pts',(-1.28435533880184,-1.,-1.48518817118891));
#30451=CARTESIAN_POINT('Ctrl Pts',(-1.28435533880184,1.,-1.48518817118891));
#30452=CARTESIAN_POINT('Ctrl Pts',(-1.28194158939522,-1.,-1.47980070347102));
#30453=CARTESIAN_POINT('Ctrl Pts',(-1.28194158939522,1.,-1.47980070347102));
#30454=CARTESIAN_POINT('Ctrl Pts',(-1.27948918248524,-1.,-1.4744717526711));
#30455=CARTESIAN_POINT('Ctrl Pts',(-1.27948918248524,1.,-1.4744717526711));
#30456=CARTESIAN_POINT('Ctrl Pts',(-1.27696414831144,-1.,-1.46916035917197));
#30457=CARTESIAN_POINT('Ctrl Pts',(-1.27696414831144,1.,-1.46916035917197));
#30458=CARTESIAN_POINT('Ctrl Pts',(-1.27433119897877,-1.,-1.4638243133254));
#30459=CARTESIAN_POINT('Ctrl Pts',(-1.27433119897877,1.,-1.4638243133254));
#30460=CARTESIAN_POINT('Ctrl Pts',(-1.27156805265312,-1.,-1.45843906294725));
#30461=CARTESIAN_POINT('Ctrl Pts',(-1.27156805265312,1.,-1.45843906294725));
#30462=CARTESIAN_POINT('Ctrl Pts',(-1.26867786804854,-1.,-1.45301422764205));
#30463=CARTESIAN_POINT('Ctrl Pts',(-1.26867786804854,1.,-1.45301422764205));
#30464=CARTESIAN_POINT('Ctrl Pts',(-1.26570925118767,-1.,-1.44761985001544));
#30465=CARTESIAN_POINT('Ctrl Pts',(-1.26570925118767,1.,-1.44761985001544));
#30466=CARTESIAN_POINT('Ctrl Pts',(-1.26273903323723,-1.,-1.44236470511145));
#30467=CARTESIAN_POINT('Ctrl Pts',(-1.26273903323723,1.,-1.44236470511145));
#30468=CARTESIAN_POINT('Ctrl Pts',(-1.25983531011894,-1.,-1.43734919180719));
#30469=CARTESIAN_POINT('Ctrl Pts',(-1.25983531011894,1.,-1.43734919180719));
#30470=CARTESIAN_POINT('Ctrl Pts',(-1.25702687965744,-1.,-1.43262645609679));
#30471=CARTESIAN_POINT('Ctrl Pts',(-1.25702687965744,1.,-1.43262645609679));
#30472=CARTESIAN_POINT('Ctrl Pts',(-1.25426945222783,-1.,-1.42815938799555));
#30473=CARTESIAN_POINT('Ctrl Pts',(-1.25426945222783,1.,-1.42815938799555));
#30474=CARTESIAN_POINT('Ctrl Pts',(-1.25141455570299,-1.,-1.42378102115911));
#30475=CARTESIAN_POINT('Ctrl Pts',(-1.25141455570299,1.,-1.42378102115911));
#30476=CARTESIAN_POINT('Ctrl Pts',(-1.24824430986911,-1.,-1.41923722596421));
#30477=CARTESIAN_POINT('Ctrl Pts',(-1.24824430986911,1.,-1.41923722596421));
#30478=CARTESIAN_POINT('Ctrl Pts',(-1.24450600513278,-1.,-1.41422913175437));
#30479=CARTESIAN_POINT('Ctrl Pts',(-1.24450600513278,1.,-1.41422913175437));
#30480=CARTESIAN_POINT('Ctrl Pts',(-1.23994455029421,-1.,-1.40845295531151));
#30481=CARTESIAN_POINT('Ctrl Pts',(-1.23994455029421,1.,-1.40845295531151));
#30482=CARTESIAN_POINT('Ctrl Pts',(-1.23434087289768,-1.,-1.40164708205345));
#30483=CARTESIAN_POINT('Ctrl Pts',(-1.23434087289768,1.,-1.40164708205345));
#30484=CARTESIAN_POINT('Ctrl Pts',(-1.22752961898063,-1.,-1.39361389567257));
#30485=CARTESIAN_POINT('Ctrl Pts',(-1.22752961898063,1.,-1.39361389567257));
#30486=CARTESIAN_POINT('Ctrl Pts',(-1.21938737278853,-1.,-1.38420564525391));
#30487=CARTESIAN_POINT('Ctrl Pts',(-1.21938737278853,1.,-1.38420564525391));
#30488=CARTESIAN_POINT('Ctrl Pts',(-1.20982812923113,-1.,-1.37331915604962));
#30489=CARTESIAN_POINT('Ctrl Pts',(-1.20982812923113,1.,-1.37331915604962));
#30490=CARTESIAN_POINT('Ctrl Pts',(-1.1987959077656,-1.,-1.36088705040677));
#30491=CARTESIAN_POINT('Ctrl Pts',(-1.1987959077656,1.,-1.36088705040677));
#30492=CARTESIAN_POINT('Ctrl Pts',(-1.18625865664915,-1.,-1.34687053998157));
#30493=CARTESIAN_POINT('Ctrl Pts',(-1.18625865664915,1.,-1.34687053998157));
#30494=CARTESIAN_POINT('Ctrl Pts',(-1.17501305787994,-1.,-1.33437539344842));
#30495=CARTESIAN_POINT('Ctrl Pts',(-1.17501305787994,1.,-1.33437539344842));
#30496=CARTESIAN_POINT('Ctrl Pts',(-1.16589330092532,-1.,-1.32428080720544));
#30497=CARTESIAN_POINT('Ctrl Pts',(-1.16589330092532,1.,-1.32428080720544));
#30498=CARTESIAN_POINT('Ctrl Pts',(-1.15950888730433,-1.,-1.3172297721596));
#30499=CARTESIAN_POINT('Ctrl Pts',(-1.15950888730433,1.,-1.3172297721596));
#30500=CARTESIAN_POINT('Ctrl Pts',(-1.15624053661742,-1.,-1.31362392696033));
#30501=CARTESIAN_POINT('Ctrl Pts',(-1.15624053661742,1.,-1.31362392696033));
#30502=CARTESIAN_POINT('',(-1.34869019493419,1.,-1.73811241238545));
#30503=CARTESIAN_POINT('Ctrl Pts',(-1.34869019493419,1.,-1.73811241238545));
#30504=CARTESIAN_POINT('Ctrl Pts',(-1.34854391898145,1.,-1.73682580585819));
#30505=CARTESIAN_POINT('Ctrl Pts',(-1.34824783113158,1.,-1.73425417886255));
#30506=CARTESIAN_POINT('Ctrl Pts',(-1.3477930915247,1.,-1.73040149654497));
#30507=CARTESIAN_POINT('Ctrl Pts',(-1.34716554820013,1.,-1.72527410681298));
#30508=CARTESIAN_POINT('Ctrl Pts',(-1.34634568653586,1.,-1.7188807715095));
#30509=CARTESIAN_POINT('Ctrl Pts',(-1.34549029589563,1.,-1.71250340687011));
#30510=CARTESIAN_POINT('Ctrl Pts',(-1.34459924533783,1.,-1.70614212266676));
#30511=CARTESIAN_POINT('Ctrl Pts',(-1.34367237124322,1.,-1.69979707754221));
#30512=CARTESIAN_POINT('Ctrl Pts',(-1.34270948206139,1.,-1.6934684849664));
#30513=CARTESIAN_POINT('Ctrl Pts',(-1.34171037484673,1.,-1.68715660868602));
#30514=CARTESIAN_POINT('Ctrl Pts',(-1.3406748518516,1.,-1.68086176030308));
#30515=CARTESIAN_POINT('Ctrl Pts',(-1.33960273470372,1.,-1.67458429426126));
#30516=CARTESIAN_POINT('Ctrl Pts',(-1.33849388654458,1.,-1.66832460784078));
#30517=CARTESIAN_POINT('Ctrl Pts',(-1.33734820885331,1.,-1.66208312542073));
#30518=CARTESIAN_POINT('Ctrl Pts',(-1.33616559745217,1.,-1.65586025952651));
#30519=CARTESIAN_POINT('Ctrl Pts',(-1.33494590468003,1.,-1.64965637286843));
#30520=CARTESIAN_POINT('Ctrl Pts',(-1.33368890676554,1.,-1.64347174856007));
#30521=CARTESIAN_POINT('Ctrl Pts',(-1.33239425103694,1.,-1.6373065347505));
#30522=CARTESIAN_POINT('Ctrl Pts',(-1.33106149345618,1.,-1.63116079730887));
#30523=CARTESIAN_POINT('Ctrl Pts',(-1.32969019505665,1.,-1.62503464209777));
#30524=CARTESIAN_POINT('Ctrl Pts',(-1.32828000610448,1.,-1.61892832270723));
#30525=CARTESIAN_POINT('Ctrl Pts',(-1.32683074483365,1.,-1.61284234015762));
#30526=CARTESIAN_POINT('Ctrl Pts',(-1.32534250785794,1.,-1.6067775829097));
#30527=CARTESIAN_POINT('Ctrl Pts',(-1.32381550858266,1.,-1.600735118587));
#30528=CARTESIAN_POINT('Ctrl Pts',(-1.32224985747686,1.,-1.59471591079408));
#30529=CARTESIAN_POINT('Ctrl Pts',(-1.32064537110891,1.,-1.58872057258244));
#30530=CARTESIAN_POINT('Ctrl Pts',(-1.31900135021428,1.,-1.58274907898829));
#30531=CARTESIAN_POINT('Ctrl Pts',(-1.31731642317183,1.,-1.57680056505585));
#30532=CARTESIAN_POINT('Ctrl Pts',(-1.31558903860015,1.,-1.57087397835721));
#30533=CARTESIAN_POINT('Ctrl Pts',(-1.31381795281002,1.,-1.56496872402352));
#30534=CARTESIAN_POINT('Ctrl Pts',(-1.31200264341696,1.,-1.55908521254822));
#30535=CARTESIAN_POINT('Ctrl Pts',(-1.31014393684221,1.,-1.55322568759481));
#30536=CARTESIAN_POINT('Ctrl Pts',(-1.30824393907471,1.,-1.54739413957183));
#30537=CARTESIAN_POINT('Ctrl Pts',(-1.30630475189553,1.,-1.54159462645428));
#30538=CARTESIAN_POINT('Ctrl Pts',(-1.30432735639487,1.,-1.53582981268976));
#30539=CARTESIAN_POINT('Ctrl Pts',(-1.3023106439557,1.,-1.53009970283893));
#30540=CARTESIAN_POINT('Ctrl Pts',(-1.30024984366334,1.,-1.5243995786107));
#30541=CARTESIAN_POINT('Ctrl Pts',(-1.29813791800757,1.,-1.51872184912735));
#30542=CARTESIAN_POINT('Ctrl Pts',(-1.29596850710518,1.,-1.51305994241412));
#30543=CARTESIAN_POINT('Ctrl Pts',(-1.29373841372843,1.,-1.50741159078367));
#30544=CARTESIAN_POINT('Ctrl Pts',(-1.29145022885171,1.,-1.50178230149764));
#30545=CARTESIAN_POINT('Ctrl Pts',(-1.28911506584232,1.,-1.49618896881729));
#30546=CARTESIAN_POINT('Ctrl Pts',(-1.28674676116415,1.,-1.4906522831275));
#30547=CARTESIAN_POINT('Ctrl Pts',(-1.28435533880184,1.,-1.48518817118891));
#30548=CARTESIAN_POINT('Ctrl Pts',(-1.28194158939522,1.,-1.47980070347102));
#30549=CARTESIAN_POINT('Ctrl Pts',(-1.27948918248524,1.,-1.4744717526711));
#30550=CARTESIAN_POINT('Ctrl Pts',(-1.27696414831144,1.,-1.46916035917197));
#30551=CARTESIAN_POINT('Ctrl Pts',(-1.27433119897877,1.,-1.4638243133254));
#30552=CARTESIAN_POINT('Ctrl Pts',(-1.27156805265312,1.,-1.45843906294725));
#30553=CARTESIAN_POINT('Ctrl Pts',(-1.26867786804854,1.,-1.45301422764205));
#30554=CARTESIAN_POINT('Ctrl Pts',(-1.26570925118767,1.,-1.44761985001544));
#30555=CARTESIAN_POINT('Ctrl Pts',(-1.26273903323723,1.,-1.44236470511145));
#30556=CARTESIAN_POINT('Ctrl Pts',(-1.25983531011894,1.,-1.43734919180719));
#30557=CARTESIAN_POINT('Ctrl Pts',(-1.25702687965744,1.,-1.43262645609679));
#30558=CARTESIAN_POINT('Ctrl Pts',(-1.25426945222783,1.,-1.42815938799555));
#30559=CARTESIAN_POINT('Ctrl Pts',(-1.25141455570299,1.,-1.42378102115911));
#30560=CARTESIAN_POINT('Ctrl Pts',(-1.24824430986911,1.,-1.41923722596421));
#30561=CARTESIAN_POINT('Ctrl Pts',(-1.24450600513278,1.,-1.41422913175437));
#30562=CARTESIAN_POINT('Ctrl Pts',(-1.23994455029421,1.,-1.40845295531151));
#30563=CARTESIAN_POINT('Ctrl Pts',(-1.23434087289768,1.,-1.40164708205345));
#30564=CARTESIAN_POINT('Ctrl Pts',(-1.22752961898063,1.,-1.39361389567257));
#30565=CARTESIAN_POINT('Ctrl Pts',(-1.21938737278853,1.,-1.38420564525391));
#30566=CARTESIAN_POINT('Ctrl Pts',(-1.20982812923113,1.,-1.37331915604962));
#30567=CARTESIAN_POINT('Ctrl Pts',(-1.1987959077656,1.,-1.36088705040677));
#30568=CARTESIAN_POINT('Ctrl Pts',(-1.18625865664915,1.,-1.34687053998157));
#30569=CARTESIAN_POINT('Ctrl Pts',(-1.17501305787994,1.,-1.33437539344842));
#30570=CARTESIAN_POINT('Ctrl Pts',(-1.16589330092532,1.,-1.32428080720544));
#30571=CARTESIAN_POINT('Ctrl Pts',(-1.15950888730433,1.,-1.3172297721596));
#30572=CARTESIAN_POINT('Ctrl Pts',(-1.15624053661742,1.,-1.31362392696033));
#30573=CARTESIAN_POINT('',(-1.34869019493419,0.,-1.73811241238545));
#30574=CARTESIAN_POINT('Origin',(-1.23627494547115,0.,-1.81978687191668));
#30575=CARTESIAN_POINT('',(-1.23627494547115,1.,-1.81978687191668));
#30576=CARTESIAN_POINT('',(-1.34869019493419,1.,-1.73811241238545));
#30577=CARTESIAN_POINT('',(-1.23627494547115,0.,-1.81978687191668));
#30578=CARTESIAN_POINT('Ctrl Pts',(-0.892032620296855,-1.,-1.5055822144029));
#30579=CARTESIAN_POINT('Ctrl Pts',(-0.892032620296855,1.,-1.5055822144029));
#30580=CARTESIAN_POINT('Ctrl Pts',(-0.894452006967538,-1.,-1.50980486807181));
#30581=CARTESIAN_POINT('Ctrl Pts',(-0.894452006967538,1.,-1.50980486807181));
#30582=CARTESIAN_POINT('Ctrl Pts',(-0.89918504749193,-1.,-1.51805569591479));
#30583=CARTESIAN_POINT('Ctrl Pts',(-0.89918504749193,1.,-1.51805569591479));
#30584=CARTESIAN_POINT('Ctrl Pts',(-0.905967409640499,-1.,-1.52984849890434));
#30585=CARTESIAN_POINT('Ctrl Pts',(-0.905967409640499,1.,-1.52984849890434));
#30586=CARTESIAN_POINT('Ctrl Pts',(-0.91437591904658,-1.,-1.54440491152808));
#30587=CARTESIAN_POINT('Ctrl Pts',(-0.91437591904658,1.,-1.54440491152808));
#30588=CARTESIAN_POINT('Ctrl Pts',(-0.923832188966322,-1.,-1.56065988582509));
#30589=CARTESIAN_POINT('Ctrl Pts',(-0.923832188966322,1.,-1.56065988582509));
#30590=CARTESIAN_POINT('Ctrl Pts',(-0.932246680128849,-1.,-1.57499388385561));
#30591=CARTESIAN_POINT('Ctrl Pts',(-0.932246680128849,1.,-1.57499388385561));
#30592=CARTESIAN_POINT('Ctrl Pts',(-0.939646377909319,-1.,-1.58744937489796));
#30593=CARTESIAN_POINT('Ctrl Pts',(-0.939646377909319,1.,-1.58744937489796));
#30594=CARTESIAN_POINT('Ctrl Pts',(-0.946078063325796,-1.,-1.59810042045408));
#30595=CARTESIAN_POINT('Ctrl Pts',(-0.946078063325796,1.,-1.59810042045408));
#30596=CARTESIAN_POINT('Ctrl Pts',(-0.951613284361248,-1.,-1.60706069897794));
#30597=CARTESIAN_POINT('Ctrl Pts',(-0.951613284361248,1.,-1.60706069897794));
#30598=CARTESIAN_POINT('Ctrl Pts',(-0.956354422921573,-1.,-1.61449324337233));
#30599=CARTESIAN_POINT('Ctrl Pts',(-0.956354422921573,1.,-1.61449324337233));
#30600=CARTESIAN_POINT('Ctrl Pts',(-0.960438326099958,-1.,-1.62061638139929));
#30601=CARTESIAN_POINT('Ctrl Pts',(-0.960438326099958,1.,-1.62061638139929));
#30602=CARTESIAN_POINT('Ctrl Pts',(-0.964046107037821,-1.,-1.6257193066974));
#30603=CARTESIAN_POINT('Ctrl Pts',(-0.964046107037821,1.,-1.6257193066974));
#30604=CARTESIAN_POINT('Ctrl Pts',(-0.967387853228041,-1.,-1.63013849959083));
#30605=CARTESIAN_POINT('Ctrl Pts',(-0.967387853228041,1.,-1.63013849959083));
#30606=CARTESIAN_POINT('Ctrl Pts',(-0.970669715996356,-1.,-1.63420665729609));
#30607=CARTESIAN_POINT('Ctrl Pts',(-0.970669715996356,1.,-1.63420665729609));
#30608=CARTESIAN_POINT('Ctrl Pts',(-0.974066058287501,-1.,-1.63820952658157));
#30609=CARTESIAN_POINT('Ctrl Pts',(-0.974066058287501,1.,-1.63820952658157));
#30610=CARTESIAN_POINT('Ctrl Pts',(-0.977689794120297,-1.,-1.64233990826831));
#30611=CARTESIAN_POINT('Ctrl Pts',(-0.977689794120297,1.,-1.64233990826831));
#30612=CARTESIAN_POINT('Ctrl Pts',(-0.981562530940574,-1.,-1.64665139190834));
#30613=CARTESIAN_POINT('Ctrl Pts',(-0.981562530940574,1.,-1.64665139190834));
#30614=CARTESIAN_POINT('Ctrl Pts',(-0.985642622921626,-1.,-1.6511001661277));
#30615=CARTESIAN_POINT('Ctrl Pts',(-0.985642622921626,1.,-1.6511001661277));
#30616=CARTESIAN_POINT('Ctrl Pts',(-0.98985562785445,-1.,-1.65559044289746));
#30617=CARTESIAN_POINT('Ctrl Pts',(-0.98985562785445,1.,-1.65559044289746));
#30618=CARTESIAN_POINT('Ctrl Pts',(-0.994121836661116,-1.,-1.66001553809916));
#30619=CARTESIAN_POINT('Ctrl Pts',(-0.994121836661116,1.,-1.66001553809916));
#30620=CARTESIAN_POINT('Ctrl Pts',(-0.998389654952317,-1.,-1.66430758030304));
#30621=CARTESIAN_POINT('Ctrl Pts',(-0.998389654952317,1.,-1.66430758030304));
#30622=CARTESIAN_POINT('Ctrl Pts',(-1.00265091003682,-1.,-1.66846059277231));
#30623=CARTESIAN_POINT('Ctrl Pts',(-1.00265091003682,1.,-1.66846059277231));
#30624=CARTESIAN_POINT('Ctrl Pts',(-1.00692206696387,-1.,-1.67250335383248));
#30625=CARTESIAN_POINT('Ctrl Pts',(-1.00692206696387,1.,-1.67250335383248));
#30626=CARTESIAN_POINT('Ctrl Pts',(-1.01123236493507,-1.,-1.67648246776457));
#30627=CARTESIAN_POINT('Ctrl Pts',(-1.01123236493507,1.,-1.67648246776457));
#30628=CARTESIAN_POINT('Ctrl Pts',(-1.01561026162787,-1.,-1.6804428989482));
#30629=CARTESIAN_POINT('Ctrl Pts',(-1.01561026162787,1.,-1.6804428989482));
#30630=CARTESIAN_POINT('Ctrl Pts',(-1.02006795074222,-1.,-1.68440578021739));
#30631=CARTESIAN_POINT('Ctrl Pts',(-1.02006795074222,1.,-1.68440578021739));
#30632=CARTESIAN_POINT('Ctrl Pts',(-1.02460180535272,-1.,-1.68836910178475));
#30633=CARTESIAN_POINT('Ctrl Pts',(-1.02460180535272,1.,-1.68836910178475));
#30634=CARTESIAN_POINT('Ctrl Pts',(-1.02919977579155,-1.,-1.69231840863471));
#30635=CARTESIAN_POINT('Ctrl Pts',(-1.02919977579155,1.,-1.69231840863471));
#30636=CARTESIAN_POINT('Ctrl Pts',(-1.03384646003587,-1.,-1.69623414782769));
#30637=CARTESIAN_POINT('Ctrl Pts',(-1.03384646003587,1.,-1.69623414782769));
#30638=CARTESIAN_POINT('Ctrl Pts',(-1.03852922490782,-1.,-1.70010052930951));
#30639=CARTESIAN_POINT('Ctrl Pts',(-1.03852922490782,1.,-1.70010052930951));
#30640=CARTESIAN_POINT('Ctrl Pts',(-1.04324363334546,-1.,-1.70391338707969));
#30641=CARTESIAN_POINT('Ctrl Pts',(-1.04324363334546,1.,-1.70391338707969));
#30642=CARTESIAN_POINT('Ctrl Pts',(-1.0479908540499,-1.,-1.70767646263641));
#30643=CARTESIAN_POINT('Ctrl Pts',(-1.0479908540499,1.,-1.70767646263641));
#30644=CARTESIAN_POINT('Ctrl Pts',(-1.05277517202854,-1.,-1.71139783543986));
#30645=CARTESIAN_POINT('Ctrl Pts',(-1.05277517202854,1.,-1.71139783543986));
#30646=CARTESIAN_POINT('Ctrl Pts',(-1.05760163192481,-1.,-1.71508654427022));
#30647=CARTESIAN_POINT('Ctrl Pts',(-1.05760163192481,1.,-1.71508654427022));
#30648=CARTESIAN_POINT('Ctrl Pts',(-1.0624732468065,-1.,-1.71874858456908));
#30649=CARTESIAN_POINT('Ctrl Pts',(-1.0624732468065,1.,-1.71874858456908));
#30650=CARTESIAN_POINT('Ctrl Pts',(-1.06738966975463,-1.,-1.72238500928456));
#30651=CARTESIAN_POINT('Ctrl Pts',(-1.06738966975463,1.,-1.72238500928456));
#30652=CARTESIAN_POINT('Ctrl Pts',(-1.07234866990252,-1.,-1.72599406198489));
#30653=CARTESIAN_POINT('Ctrl Pts',(-1.07234866990252,1.,-1.72599406198489));
#30654=CARTESIAN_POINT('Ctrl Pts',(-1.0773470373727,-1.,-1.72957248977424));
#30655=CARTESIAN_POINT('Ctrl Pts',(-1.0773470373727,1.,-1.72957248977424));
#30656=CARTESIAN_POINT('Ctrl Pts',(-1.08238162784749,-1.,-1.73311705663407));
#30657=CARTESIAN_POINT('Ctrl Pts',(-1.08238162784749,1.,-1.73311705663407));
#30658=CARTESIAN_POINT('Ctrl Pts',(-1.08745056285429,-1.,-1.73662628326093));
#30659=CARTESIAN_POINT('Ctrl Pts',(-1.08745056285429,1.,-1.73662628326093));
#30660=CARTESIAN_POINT('Ctrl Pts',(-1.09255329056496,-1.,-1.74010053962252));
#30661=CARTESIAN_POINT('Ctrl Pts',(-1.09255329056496,1.,-1.74010053962252));
#30662=CARTESIAN_POINT('Ctrl Pts',(-1.09768999241229,-1.,-1.74354119236212));
#30663=CARTESIAN_POINT('Ctrl Pts',(-1.09768999241229,1.,-1.74354119236212));
#30664=CARTESIAN_POINT('Ctrl Pts',(-1.10286118991144,-1.,-1.74695004214924));
#30665=CARTESIAN_POINT('Ctrl Pts',(-1.10286118991144,1.,-1.74695004214924));
#30666=CARTESIAN_POINT('Ctrl Pts',(-1.10806728183003,-1.,-1.75032866075914));
#30667=CARTESIAN_POINT('Ctrl Pts',(-1.10806728183003,1.,-1.75032866075914));
#30668=CARTESIAN_POINT('Ctrl Pts',(-1.11330807582542,-1.,-1.75367772094617));
#30669=CARTESIAN_POINT('Ctrl Pts',(-1.11330807582542,1.,-1.75367772094617));
#30670=CARTESIAN_POINT('Ctrl Pts',(-1.11858293216752,-1.,-1.75699720772089));
#30671=CARTESIAN_POINT('Ctrl Pts',(-1.11858293216752,1.,-1.75699720772089));
#30672=CARTESIAN_POINT('Ctrl Pts',(-1.12389096855078,-1.,-1.76028671825084));
#30673=CARTESIAN_POINT('Ctrl Pts',(-1.12389096855078,1.,-1.76028671825084));
#30674=CARTESIAN_POINT('Ctrl Pts',(-1.12923123555076,-1.,-1.76354571966171));
#30675=CARTESIAN_POINT('Ctrl Pts',(-1.12923123555076,1.,-1.76354571966171));
#30676=CARTESIAN_POINT('Ctrl Pts',(-1.13460291804635,-1.,-1.76677384551883));
#30677=CARTESIAN_POINT('Ctrl Pts',(-1.13460291804635,1.,-1.76677384551883));
#30678=CARTESIAN_POINT('Ctrl Pts',(-1.14000548337,-1.,-1.76997111386806));
#30679=CARTESIAN_POINT('Ctrl Pts',(-1.14000548337,1.,-1.76997111386806));
#30680=CARTESIAN_POINT('Ctrl Pts',(-1.14543858226948,-1.,-1.77313777896234));
#30681=CARTESIAN_POINT('Ctrl Pts',(-1.14543858226948,1.,-1.77313777896234));
#30682=CARTESIAN_POINT('Ctrl Pts',(-1.15090197841531,-1.,-1.77627422557034));
#30683=CARTESIAN_POINT('Ctrl Pts',(-1.15090197841531,1.,-1.77627422557034));
#30684=CARTESIAN_POINT('Ctrl Pts',(-1.15639547194689,-1.,-1.77938085564261));
#30685=CARTESIAN_POINT('Ctrl Pts',(-1.15639547194689,1.,-1.77938085564261));
#30686=CARTESIAN_POINT('Ctrl Pts',(-1.16191881298458,-1.,-1.78245795880949));
#30687=CARTESIAN_POINT('Ctrl Pts',(-1.16191881298458,1.,-1.78245795880949));
#30688=CARTESIAN_POINT('Ctrl Pts',(-1.16747166312239,-1.,-1.78550566040349));
#30689=CARTESIAN_POINT('Ctrl Pts',(-1.16747166312239,1.,-1.78550566040349));
#30690=CARTESIAN_POINT('Ctrl Pts',(-1.17305363177265,-1.,-1.78852398877523));
#30691=CARTESIAN_POINT('Ctrl Pts',(-1.17305363177265,1.,-1.78852398877523));
#30692=CARTESIAN_POINT('Ctrl Pts',(-1.17866429440781,-1.,-1.79151291552646));
#30693=CARTESIAN_POINT('Ctrl Pts',(-1.17866429440781,1.,-1.79151291552646));
#30694=CARTESIAN_POINT('Ctrl Pts',(-1.18430321697471,-1.,-1.79447240321572));
#30695=CARTESIAN_POINT('Ctrl Pts',(-1.18430321697471,1.,-1.79447240321572));
#30696=CARTESIAN_POINT('Ctrl Pts',(-1.1899699793456,-1.,-1.79740245923649));
#30697=CARTESIAN_POINT('Ctrl Pts',(-1.1899699793456,1.,-1.79740245923649));
#30698=CARTESIAN_POINT('Ctrl Pts',(-1.19566418930405,-1.,-1.80030314370121));
#30699=CARTESIAN_POINT('Ctrl Pts',(-1.19566418930405,1.,-1.80030314370121));
#30700=CARTESIAN_POINT('Ctrl Pts',(-1.2013854893912,-1.,-1.8031745483882));
#30701=CARTESIAN_POINT('Ctrl Pts',(-1.2013854893912,1.,-1.8031745483882));
#30702=CARTESIAN_POINT('Ctrl Pts',(-1.20713356605519,-1.,-1.80601678480772));
#30703=CARTESIAN_POINT('Ctrl Pts',(-1.20713356605519,1.,-1.80601678480772));
#30704=CARTESIAN_POINT('Ctrl Pts',(-1.2129081570818,-1.,-1.80882996916931));
#30705=CARTESIAN_POINT('Ctrl Pts',(-1.2129081570818,1.,-1.80882996916931));
#30706=CARTESIAN_POINT('Ctrl Pts',(-1.2187090610323,-1.,-1.81161420806172));
#30707=CARTESIAN_POINT('Ctrl Pts',(-1.2187090610323,1.,-1.81161420806172));
#30708=CARTESIAN_POINT('Ctrl Pts',(-1.22453613304507,-1.,-1.81436959209778));
#30709=CARTESIAN_POINT('Ctrl Pts',(-1.22453613304507,1.,-1.81436959209778));
#30710=CARTESIAN_POINT('Ctrl Pts',(-1.22921864890975,-1.,-1.81655087183054));
#30711=CARTESIAN_POINT('Ctrl Pts',(-1.22921864890975,1.,-1.81655087183054));
#30712=CARTESIAN_POINT('Ctrl Pts',(-1.23274224526804,-1.,-1.81817389920914));
#30713=CARTESIAN_POINT('Ctrl Pts',(-1.23274224526804,1.,-1.81817389920914));
#30714=CARTESIAN_POINT('Ctrl Pts',(-1.23509651170384,-1.,-1.81925017193531));
#30715=CARTESIAN_POINT('Ctrl Pts',(-1.23509651170384,1.,-1.81925017193531));
#30716=CARTESIAN_POINT('Ctrl Pts',(-1.23627494547115,-1.,-1.81978687191668));
#30717=CARTESIAN_POINT('Ctrl Pts',(-1.23627494547115,1.,-1.81978687191668));
#30718=CARTESIAN_POINT('',(-0.892032620296855,1.,-1.5055822144029));
#30719=CARTESIAN_POINT('Ctrl Pts',(-0.892032620296855,1.,-1.5055822144029));
#30720=CARTESIAN_POINT('Ctrl Pts',(-0.894452006967538,1.,-1.50980486807181));
#30721=CARTESIAN_POINT('Ctrl Pts',(-0.89918504749193,1.,-1.51805569591479));
#30722=CARTESIAN_POINT('Ctrl Pts',(-0.905967409640499,1.,-1.52984849890434));
#30723=CARTESIAN_POINT('Ctrl Pts',(-0.91437591904658,1.,-1.54440491152808));
#30724=CARTESIAN_POINT('Ctrl Pts',(-0.923832188966322,1.,-1.56065988582509));
#30725=CARTESIAN_POINT('Ctrl Pts',(-0.932246680128849,1.,-1.57499388385561));
#30726=CARTESIAN_POINT('Ctrl Pts',(-0.939646377909319,1.,-1.58744937489796));
#30727=CARTESIAN_POINT('Ctrl Pts',(-0.946078063325796,1.,-1.59810042045408));
#30728=CARTESIAN_POINT('Ctrl Pts',(-0.951613284361248,1.,-1.60706069897794));
#30729=CARTESIAN_POINT('Ctrl Pts',(-0.956354422921573,1.,-1.61449324337233));
#30730=CARTESIAN_POINT('Ctrl Pts',(-0.960438326099958,1.,-1.62061638139929));
#30731=CARTESIAN_POINT('Ctrl Pts',(-0.964046107037821,1.,-1.6257193066974));
#30732=CARTESIAN_POINT('Ctrl Pts',(-0.967387853228041,1.,-1.63013849959083));
#30733=CARTESIAN_POINT('Ctrl Pts',(-0.970669715996356,1.,-1.63420665729609));
#30734=CARTESIAN_POINT('Ctrl Pts',(-0.974066058287501,1.,-1.63820952658157));
#30735=CARTESIAN_POINT('Ctrl Pts',(-0.977689794120297,1.,-1.64233990826831));
#30736=CARTESIAN_POINT('Ctrl Pts',(-0.981562530940574,1.,-1.64665139190834));
#30737=CARTESIAN_POINT('Ctrl Pts',(-0.985642622921626,1.,-1.6511001661277));
#30738=CARTESIAN_POINT('Ctrl Pts',(-0.98985562785445,1.,-1.65559044289746));
#30739=CARTESIAN_POINT('Ctrl Pts',(-0.994121836661116,1.,-1.66001553809916));
#30740=CARTESIAN_POINT('Ctrl Pts',(-0.998389654952317,1.,-1.66430758030304));
#30741=CARTESIAN_POINT('Ctrl Pts',(-1.00265091003682,1.,-1.66846059277231));
#30742=CARTESIAN_POINT('Ctrl Pts',(-1.00692206696387,1.,-1.67250335383248));
#30743=CARTESIAN_POINT('Ctrl Pts',(-1.01123236493507,1.,-1.67648246776457));
#30744=CARTESIAN_POINT('Ctrl Pts',(-1.01561026162787,1.,-1.6804428989482));
#30745=CARTESIAN_POINT('Ctrl Pts',(-1.02006795074222,1.,-1.68440578021739));
#30746=CARTESIAN_POINT('Ctrl Pts',(-1.02460180535272,1.,-1.68836910178475));
#30747=CARTESIAN_POINT('Ctrl Pts',(-1.02919977579155,1.,-1.69231840863471));
#30748=CARTESIAN_POINT('Ctrl Pts',(-1.03384646003587,1.,-1.69623414782769));
#30749=CARTESIAN_POINT('Ctrl Pts',(-1.03852922490782,1.,-1.70010052930951));
#30750=CARTESIAN_POINT('Ctrl Pts',(-1.04324363334546,1.,-1.70391338707969));
#30751=CARTESIAN_POINT('Ctrl Pts',(-1.0479908540499,1.,-1.70767646263641));
#30752=CARTESIAN_POINT('Ctrl Pts',(-1.05277517202854,1.,-1.71139783543986));
#30753=CARTESIAN_POINT('Ctrl Pts',(-1.05760163192481,1.,-1.71508654427022));
#30754=CARTESIAN_POINT('Ctrl Pts',(-1.0624732468065,1.,-1.71874858456908));
#30755=CARTESIAN_POINT('Ctrl Pts',(-1.06738966975463,1.,-1.72238500928456));
#30756=CARTESIAN_POINT('Ctrl Pts',(-1.07234866990252,1.,-1.72599406198489));
#30757=CARTESIAN_POINT('Ctrl Pts',(-1.0773470373727,1.,-1.72957248977424));
#30758=CARTESIAN_POINT('Ctrl Pts',(-1.08238162784749,1.,-1.73311705663407));
#30759=CARTESIAN_POINT('Ctrl Pts',(-1.08745056285429,1.,-1.73662628326093));
#30760=CARTESIAN_POINT('Ctrl Pts',(-1.09255329056496,1.,-1.74010053962252));
#30761=CARTESIAN_POINT('Ctrl Pts',(-1.09768999241229,1.,-1.74354119236212));
#30762=CARTESIAN_POINT('Ctrl Pts',(-1.10286118991144,1.,-1.74695004214924));
#30763=CARTESIAN_POINT('Ctrl Pts',(-1.10806728183003,1.,-1.75032866075914));
#30764=CARTESIAN_POINT('Ctrl Pts',(-1.11330807582542,1.,-1.75367772094617));
#30765=CARTESIAN_POINT('Ctrl Pts',(-1.11858293216752,1.,-1.75699720772089));
#30766=CARTESIAN_POINT('Ctrl Pts',(-1.12389096855078,1.,-1.76028671825084));
#30767=CARTESIAN_POINT('Ctrl Pts',(-1.12923123555076,1.,-1.76354571966171));
#30768=CARTESIAN_POINT('Ctrl Pts',(-1.13460291804635,1.,-1.76677384551883));
#30769=CARTESIAN_POINT('Ctrl Pts',(-1.14000548337,1.,-1.76997111386806));
#30770=CARTESIAN_POINT('Ctrl Pts',(-1.14543858226948,1.,-1.77313777896234));
#30771=CARTESIAN_POINT('Ctrl Pts',(-1.15090197841531,1.,-1.77627422557034));
#30772=CARTESIAN_POINT('Ctrl Pts',(-1.15639547194689,1.,-1.77938085564261));
#30773=CARTESIAN_POINT('Ctrl Pts',(-1.16191881298458,1.,-1.78245795880949));
#30774=CARTESIAN_POINT('Ctrl Pts',(-1.16747166312239,1.,-1.78550566040349));
#30775=CARTESIAN_POINT('Ctrl Pts',(-1.17305363177265,1.,-1.78852398877523));
#30776=CARTESIAN_POINT('Ctrl Pts',(-1.17866429440781,1.,-1.79151291552646));
#30777=CARTESIAN_POINT('Ctrl Pts',(-1.18430321697471,1.,-1.79447240321572));
#30778=CARTESIAN_POINT('Ctrl Pts',(-1.1899699793456,1.,-1.79740245923649));
#30779=CARTESIAN_POINT('Ctrl Pts',(-1.19566418930405,1.,-1.80030314370121));
#30780=CARTESIAN_POINT('Ctrl Pts',(-1.2013854893912,1.,-1.8031745483882));
#30781=CARTESIAN_POINT('Ctrl Pts',(-1.20713356605519,1.,-1.80601678480772));
#30782=CARTESIAN_POINT('Ctrl Pts',(-1.2129081570818,1.,-1.80882996916931));
#30783=CARTESIAN_POINT('Ctrl Pts',(-1.2187090610323,1.,-1.81161420806172));
#30784=CARTESIAN_POINT('Ctrl Pts',(-1.22453613304507,1.,-1.81436959209778));
#30785=CARTESIAN_POINT('Ctrl Pts',(-1.22921864890975,1.,-1.81655087183054));
#30786=CARTESIAN_POINT('Ctrl Pts',(-1.23274224526804,1.,-1.81817389920914));
#30787=CARTESIAN_POINT('Ctrl Pts',(-1.23509651170384,1.,-1.81925017193531));
#30788=CARTESIAN_POINT('Ctrl Pts',(-1.23627494547115,1.,-1.81978687191668));
#30789=CARTESIAN_POINT('',(-0.892032620296856,0.,-1.5055822144029));
#30790=CARTESIAN_POINT('Origin',(0.,0.,0.));
#30791=CARTESIAN_POINT('',(-0.693717979106305,1.,-1.60662857109684));
#30792=CARTESIAN_POINT('Origin',(0.,1.,0.));
#30793=CARTESIAN_POINT('',(-0.693717979106306,0.,-1.60662857109684));
#30794=CARTESIAN_POINT('Ctrl Pts',(-0.745574324794401,-1.,-2.0698113262342));
#30795=CARTESIAN_POINT('Ctrl Pts',(-0.745574324794401,1.,-2.0698113262342));
#30796=CARTESIAN_POINT('Ctrl Pts',(-0.745832791378367,-1.,-2.06854248895728));
#30797=CARTESIAN_POINT('Ctrl Pts',(-0.745832791378367,1.,-2.06854248895728));
#30798=CARTESIAN_POINT('Ctrl Pts',(-0.7463458715442,-1.,-2.06600523016815));
#30799=CARTESIAN_POINT('Ctrl Pts',(-0.7463458715442,1.,-2.06600523016815));
#30800=CARTESIAN_POINT('Ctrl Pts',(-0.747103932787919,-1.,-2.06220058927826));
#30801=CARTESIAN_POINT('Ctrl Pts',(-0.747103932787919,1.,-2.06220058927826));
#30802=CARTESIAN_POINT('Ctrl Pts',(-0.748091554183802,-1.,-2.05713023031006));
#30803=CARTESIAN_POINT('Ctrl Pts',(-0.748091554183802,1.,-2.05713023031006));
#30804=CARTESIAN_POINT('Ctrl Pts',(-0.749287468665046,-1.,-2.05079645592154));
#30805=CARTESIAN_POINT('Ctrl Pts',(-0.749287468665046,1.,-2.05079645592154));
#30806=CARTESIAN_POINT('Ctrl Pts',(-0.750444657875576,-1.,-2.04446689147979));
#30807=CARTESIAN_POINT('Ctrl Pts',(-0.750444657875576,1.,-2.04446689147979));
#30808=CARTESIAN_POINT('Ctrl Pts',(-0.751562963361115,-1.,-2.03814160092099));
#30809=CARTESIAN_POINT('Ctrl Pts',(-0.751562963361115,1.,-2.03814160092099));
#30810=CARTESIAN_POINT('Ctrl Pts',(-0.752642180487211,-1.,-2.03182068456221));
#30811=CARTESIAN_POINT('Ctrl Pts',(-0.752642180487211,1.,-2.03182068456221));
#30812=CARTESIAN_POINT('Ctrl Pts',(-0.753682061112768,-1.,-2.02550428623313));
#30813=CARTESIAN_POINT('Ctrl Pts',(-0.753682061112768,1.,-2.02550428623313));
#30814=CARTESIAN_POINT('Ctrl Pts',(-0.754682330722816,-1.,-2.01919259405809));
#30815=CARTESIAN_POINT('Ctrl Pts',(-0.754682330722816,1.,-2.01919259405809));
#30816=CARTESIAN_POINT('Ctrl Pts',(-0.755642704957865,-1.,-2.01288584328084));
#30817=CARTESIAN_POINT('Ctrl Pts',(-0.755642704957865,1.,-2.01288584328084));
#30818=CARTESIAN_POINT('Ctrl Pts',(-0.75656290464667,-1.,-2.0065843158773));
#30819=CARTESIAN_POINT('Ctrl Pts',(-0.75656290464667,1.,-2.0065843158773));
#30820=CARTESIAN_POINT('Ctrl Pts',(-0.757442676862724,-1.,-2.00028834739178));
#30821=CARTESIAN_POINT('Ctrl Pts',(-0.757442676862724,1.,-2.00028834739178));
#30822=CARTESIAN_POINT('Ctrl Pts',(-0.758281796766761,-1.,-1.99399831098817));
#30823=CARTESIAN_POINT('Ctrl Pts',(-0.758281796766761,1.,-1.99399831098817));
#30824=CARTESIAN_POINT('Ctrl Pts',(-0.759080037802488,-1.,-1.98771456680874));
#30825=CARTESIAN_POINT('Ctrl Pts',(-0.759080037802488,1.,-1.98771456680874));
#30826=CARTESIAN_POINT('Ctrl Pts',(-0.75983714745219,-1.,-1.98143741418172));
#30827=CARTESIAN_POINT('Ctrl Pts',(-0.75983714745219,1.,-1.98143741418172));
#30828=CARTESIAN_POINT('Ctrl Pts',(-0.760552825409757,-1.,-1.97516705321494));
#30829=CARTESIAN_POINT('Ctrl Pts',(-0.760552825409757,1.,-1.97516705321494));
#30830=CARTESIAN_POINT('Ctrl Pts',(-0.76122669048382,-1.,-1.96890351582499));
#30831=CARTESIAN_POINT('Ctrl Pts',(-0.76122669048382,1.,-1.96890351582499));
#30832=CARTESIAN_POINT('Ctrl Pts',(-0.761858300014423,-1.,-1.96264672744186));
#30833=CARTESIAN_POINT('Ctrl Pts',(-0.761858300014423,1.,-1.96264672744186));
#30834=CARTESIAN_POINT('Ctrl Pts',(-0.762447203806179,-1.,-1.95639665309869));
#30835=CARTESIAN_POINT('Ctrl Pts',(-0.762447203806179,1.,-1.95639665309869));
#30836=CARTESIAN_POINT('Ctrl Pts',(-0.762992990878769,-1.,-1.95015342590024));
#30837=CARTESIAN_POINT('Ctrl Pts',(-0.762992990878769,1.,-1.95015342590024));
#30838=CARTESIAN_POINT('Ctrl Pts',(-0.763495333538629,-1.,-1.9439174661764));
#30839=CARTESIAN_POINT('Ctrl Pts',(-0.763495333538629,1.,-1.9439174661764));
#30840=CARTESIAN_POINT('Ctrl Pts',(-0.763954049121458,-1.,-1.93768964875886));
#30841=CARTESIAN_POINT('Ctrl Pts',(-0.763954049121458,1.,-1.93768964875886));
#30842=CARTESIAN_POINT('Ctrl Pts',(-0.764369010673941,-1.,-1.93147105496382));
#30843=CARTESIAN_POINT('Ctrl Pts',(-0.764369010673941,1.,-1.93147105496382));
#30844=CARTESIAN_POINT('Ctrl Pts',(-0.764740025488211,-1.,-1.92526263537048));
#30845=CARTESIAN_POINT('Ctrl Pts',(-0.764740025488211,1.,-1.92526263537048));
#30846=CARTESIAN_POINT('Ctrl Pts',(-0.765066729667088,-1.,-1.91906491634196));
#30847=CARTESIAN_POINT('Ctrl Pts',(-0.765066729667088,1.,-1.91906491634196));
#30848=CARTESIAN_POINT('Ctrl Pts',(-0.765348465884722,-1.,-1.91287765805169));
#30849=CARTESIAN_POINT('Ctrl Pts',(-0.765348465884722,1.,-1.91287765805169));
#30850=CARTESIAN_POINT('Ctrl Pts',(-0.765584196937919,-1.,-1.90669961402356));
#30851=CARTESIAN_POINT('Ctrl Pts',(-0.765584196937919,1.,-1.90669961402356));
#30852=CARTESIAN_POINT('Ctrl Pts',(-0.765772772593386,-1.,-1.90052930393596));
#30853=CARTESIAN_POINT('Ctrl Pts',(-0.765772772593386,1.,-1.90052930393596));
#30854=CARTESIAN_POINT('Ctrl Pts',(-0.765913193856978,-1.,-1.89436577771388));
#30855=CARTESIAN_POINT('Ctrl Pts',(-0.765913193856978,1.,-1.89436577771388));
#30856=CARTESIAN_POINT('Ctrl Pts',(-0.766004837062091,-1.,-1.88820926433409));
#30857=CARTESIAN_POINT('Ctrl Pts',(-0.766004837062091,1.,-1.88820926433409));
#30858=CARTESIAN_POINT('Ctrl Pts',(-0.766047794851865,-1.,-1.88206215302561));
#30859=CARTESIAN_POINT('Ctrl Pts',(-0.766047794851865,1.,-1.88206215302561));
#30860=CARTESIAN_POINT('Ctrl Pts',(-0.766042837036744,-1.,-1.87592888967883));
#30861=CARTESIAN_POINT('Ctrl Pts',(-0.766042837036744,1.,-1.87592888967883));
#30862=CARTESIAN_POINT('Ctrl Pts',(-0.765990708546091,-1.,-1.86981398314341));
#30863=CARTESIAN_POINT('Ctrl Pts',(-0.765990708546091,1.,-1.86981398314341));
#30864=CARTESIAN_POINT('Ctrl Pts',(-0.765891519092547,-1.,-1.86372027063312));
#30865=CARTESIAN_POINT('Ctrl Pts',(-0.765891519092547,1.,-1.86372027063312));
#30866=CARTESIAN_POINT('Ctrl Pts',(-0.765744212909318,-1.,-1.85764741390394));
#30867=CARTESIAN_POINT('Ctrl Pts',(-0.765744212909318,1.,-1.85764741390394));
#30868=CARTESIAN_POINT('Ctrl Pts',(-0.765545710619062,-1.,-1.85158945130063));
#30869=CARTESIAN_POINT('Ctrl Pts',(-0.765545710619062,1.,-1.85158945130063));
#30870=CARTESIAN_POINT('Ctrl Pts',(-0.765291664862029,-1.,-1.84553698875924));
#30871=CARTESIAN_POINT('Ctrl Pts',(-0.765291664862029,1.,-1.84553698875924));
#30872=CARTESIAN_POINT('Ctrl Pts',(-0.764978057881737,-1.,-1.83948181064835));
#30873=CARTESIAN_POINT('Ctrl Pts',(-0.764978057881737,1.,-1.83948181064835));
#30874=CARTESIAN_POINT('Ctrl Pts',(-0.764602549687853,-1.,-1.83342077227142));
#30875=CARTESIAN_POINT('Ctrl Pts',(-0.764602549687853,1.,-1.83342077227142));
#30876=CARTESIAN_POINT('Ctrl Pts',(-0.764165902605995,-1.,-1.82735991200065));
#30877=CARTESIAN_POINT('Ctrl Pts',(-0.764165902605995,1.,-1.82735991200065));
#30878=CARTESIAN_POINT('Ctrl Pts',(-0.763673465462726,-1.,-1.82131873145266));
#30879=CARTESIAN_POINT('Ctrl Pts',(-0.763673465462726,1.,-1.82131873145266));
#30880=CARTESIAN_POINT('Ctrl Pts',(-0.763132003836634,-1.,-1.8153211840553));
#30881=CARTESIAN_POINT('Ctrl Pts',(-0.763132003836634,1.,-1.8153211840553));
#30882=CARTESIAN_POINT('Ctrl Pts',(-0.762546129463938,-1.,-1.80938551463965));
#30883=CARTESIAN_POINT('Ctrl Pts',(-0.762546129463938,1.,-1.80938551463965));
#30884=CARTESIAN_POINT('Ctrl Pts',(-0.761915336443547,-1.,-1.80351583877342));
#30885=CARTESIAN_POINT('Ctrl Pts',(-0.761915336443547,1.,-1.80351583877342));
#30886=CARTESIAN_POINT('Ctrl Pts',(-0.761229695230558,-1.,-1.79768986997783));
#30887=CARTESIAN_POINT('Ctrl Pts',(-0.761229695230558,1.,-1.79768986997783));
#30888=CARTESIAN_POINT('Ctrl Pts',(-0.760469555880749,-1.,-1.7918581561088));
#30889=CARTESIAN_POINT('Ctrl Pts',(-0.760469555880749,1.,-1.7918581561088));
#30890=CARTESIAN_POINT('Ctrl Pts',(-0.759614401110189,-1.,-1.78596964884604));
#30891=CARTESIAN_POINT('Ctrl Pts',(-0.759614401110189,1.,-1.78596964884604));
#30892=CARTESIAN_POINT('Ctrl Pts',(-0.758650626677518,-1.,-1.77999411220945));
#30893=CARTESIAN_POINT('Ctrl Pts',(-0.758650626677518,1.,-1.77999411220945));
#30894=CARTESIAN_POINT('Ctrl Pts',(-0.757578264077029,-1.,-1.77394167108292));
#30895=CARTESIAN_POINT('Ctrl Pts',(-0.757578264077029,1.,-1.77394167108292));
#30896=CARTESIAN_POINT('Ctrl Pts',(-0.75642189602781,-1.,-1.76789396002998));
#30897=CARTESIAN_POINT('Ctrl Pts',(-0.75642189602781,1.,-1.76789396002998));
#30898=CARTESIAN_POINT('Ctrl Pts',(-0.755220979974461,-1.,-1.76197817240128));
#30899=CARTESIAN_POINT('Ctrl Pts',(-0.755220979974461,1.,-1.76197817240128));
#30900=CARTESIAN_POINT('Ctrl Pts',(-0.754009254027829,-1.,-1.75631083600019));
#30901=CARTESIAN_POINT('Ctrl Pts',(-0.754009254027829,1.,-1.75631083600019));
#30902=CARTESIAN_POINT('Ctrl Pts',(-0.752797683531314,-1.,-1.75095139468794));
#30903=CARTESIAN_POINT('Ctrl Pts',(-0.752797683531314,1.,-1.75095139468794));
#30904=CARTESIAN_POINT('Ctrl Pts',(-0.751555614164482,-1.,-1.74585086852502));
#30905=CARTESIAN_POINT('Ctrl Pts',(-0.751555614164482,1.,-1.74585086852502));
#30906=CARTESIAN_POINT('Ctrl Pts',(-0.750193435981249,-1.,-1.74080458267114));
#30907=CARTESIAN_POINT('Ctrl Pts',(-0.750193435981249,1.,-1.74080458267114));
#30908=CARTESIAN_POINT('Ctrl Pts',(-0.74858246295687,-1.,-1.7355035168033));
#30909=CARTESIAN_POINT('Ctrl Pts',(-0.74858246295687,1.,-1.7355035168033));
#30910=CARTESIAN_POINT('Ctrl Pts',(-0.746574710097752,-1.,-1.72958533647714));
#30911=CARTESIAN_POINT('Ctrl Pts',(-0.746574710097752,1.,-1.72958533647714));
#30912=CARTESIAN_POINT('Ctrl Pts',(-0.744021445433093,-1.,-1.72268229916769));
#30913=CARTESIAN_POINT('Ctrl Pts',(-0.744021445433093,1.,-1.72268229916769));
#30914=CARTESIAN_POINT('Ctrl Pts',(-0.74079516202821,-1.,-1.71447789751001));
#30915=CARTESIAN_POINT('Ctrl Pts',(-0.74079516202821,1.,-1.71447789751001));
#30916=CARTESIAN_POINT('Ctrl Pts',(-0.736799665716932,-1.,-1.70473309004249));
#30917=CARTESIAN_POINT('Ctrl Pts',(-0.736799665716932,1.,-1.70473309004249));
#30918=CARTESIAN_POINT('Ctrl Pts',(-0.731963238685357,-1.,-1.69326921972915));
#30919=CARTESIAN_POINT('Ctrl Pts',(-0.731963238685357,1.,-1.69326921972915));
#30920=CARTESIAN_POINT('Ctrl Pts',(-0.726235967982445,-1.,-1.67996158451922));
#30921=CARTESIAN_POINT('Ctrl Pts',(-0.726235967982445,1.,-1.67996158451922));
#30922=CARTESIAN_POINT('Ctrl Pts',(-0.71958543378795,-1.,-1.66472880551777));
#30923=CARTESIAN_POINT('Ctrl Pts',(-0.71958543378795,1.,-1.66472880551777));
#30924=CARTESIAN_POINT('Ctrl Pts',(-0.711993139340447,-1.,-1.64752408828442));
#30925=CARTESIAN_POINT('Ctrl Pts',(-0.711993139340447,1.,-1.64752408828442));
#30926=CARTESIAN_POINT('Ctrl Pts',(-0.705159151977294,-1.,-1.6321654166204));
#30927=CARTESIAN_POINT('Ctrl Pts',(-0.705159151977294,1.,-1.6321654166204));
#30928=CARTESIAN_POINT('Ctrl Pts',(-0.699605146398837,-1.,-1.61974673471117));
#30929=CARTESIAN_POINT('Ctrl Pts',(-0.699605146398837,1.,-1.61974673471117));
#30930=CARTESIAN_POINT('Ctrl Pts',(-0.69571209787897,-1.,-1.61106790957619));
#30931=CARTESIAN_POINT('Ctrl Pts',(-0.69571209787897,1.,-1.61106790957619));
#30932=CARTESIAN_POINT('Ctrl Pts',(-0.693717979106305,-1.,-1.60662857109684));
#30933=CARTESIAN_POINT('Ctrl Pts',(-0.693717979106305,1.,-1.60662857109684));
#30934=CARTESIAN_POINT('',(-0.745574324794401,1.,-2.0698113262342));
#30935=CARTESIAN_POINT('Ctrl Pts',(-0.745574324794401,1.,-2.0698113262342));
#30936=CARTESIAN_POINT('Ctrl Pts',(-0.745832791378367,1.,-2.06854248895728));
#30937=CARTESIAN_POINT('Ctrl Pts',(-0.7463458715442,1.,-2.06600523016815));
#30938=CARTESIAN_POINT('Ctrl Pts',(-0.747103932787919,1.,-2.06220058927826));
#30939=CARTESIAN_POINT('Ctrl Pts',(-0.748091554183802,1.,-2.05713023031006));
#30940=CARTESIAN_POINT('Ctrl Pts',(-0.749287468665046,1.,-2.05079645592154));
#30941=CARTESIAN_POINT('Ctrl Pts',(-0.750444657875576,1.,-2.04446689147979));
#30942=CARTESIAN_POINT('Ctrl Pts',(-0.751562963361115,1.,-2.03814160092099));
#30943=CARTESIAN_POINT('Ctrl Pts',(-0.752642180487211,1.,-2.03182068456221));
#30944=CARTESIAN_POINT('Ctrl Pts',(-0.753682061112768,1.,-2.02550428623313));
#30945=CARTESIAN_POINT('Ctrl Pts',(-0.754682330722816,1.,-2.01919259405809));
#30946=CARTESIAN_POINT('Ctrl Pts',(-0.755642704957865,1.,-2.01288584328084));
#30947=CARTESIAN_POINT('Ctrl Pts',(-0.75656290464667,1.,-2.0065843158773));
#30948=CARTESIAN_POINT('Ctrl Pts',(-0.757442676862724,1.,-2.00028834739178));
#30949=CARTESIAN_POINT('Ctrl Pts',(-0.758281796766761,1.,-1.99399831098817));
#30950=CARTESIAN_POINT('Ctrl Pts',(-0.759080037802488,1.,-1.98771456680874));
#30951=CARTESIAN_POINT('Ctrl Pts',(-0.75983714745219,1.,-1.98143741418172));
#30952=CARTESIAN_POINT('Ctrl Pts',(-0.760552825409757,1.,-1.97516705321494));
#30953=CARTESIAN_POINT('Ctrl Pts',(-0.76122669048382,1.,-1.96890351582499));
#30954=CARTESIAN_POINT('Ctrl Pts',(-0.761858300014423,1.,-1.96264672744186));
#30955=CARTESIAN_POINT('Ctrl Pts',(-0.762447203806179,1.,-1.95639665309869));
#30956=CARTESIAN_POINT('Ctrl Pts',(-0.762992990878769,1.,-1.95015342590024));
#30957=CARTESIAN_POINT('Ctrl Pts',(-0.763495333538629,1.,-1.9439174661764));
#30958=CARTESIAN_POINT('Ctrl Pts',(-0.763954049121458,1.,-1.93768964875886));
#30959=CARTESIAN_POINT('Ctrl Pts',(-0.764369010673941,1.,-1.93147105496382));
#30960=CARTESIAN_POINT('Ctrl Pts',(-0.764740025488211,1.,-1.92526263537048));
#30961=CARTESIAN_POINT('Ctrl Pts',(-0.765066729667088,1.,-1.91906491634196));
#30962=CARTESIAN_POINT('Ctrl Pts',(-0.765348465884722,1.,-1.91287765805169));
#30963=CARTESIAN_POINT('Ctrl Pts',(-0.765584196937919,1.,-1.90669961402356));
#30964=CARTESIAN_POINT('Ctrl Pts',(-0.765772772593386,1.,-1.90052930393596));
#30965=CARTESIAN_POINT('Ctrl Pts',(-0.765913193856978,1.,-1.89436577771388));
#30966=CARTESIAN_POINT('Ctrl Pts',(-0.766004837062091,1.,-1.88820926433409));
#30967=CARTESIAN_POINT('Ctrl Pts',(-0.766047794851865,1.,-1.88206215302561));
#30968=CARTESIAN_POINT('Ctrl Pts',(-0.766042837036744,1.,-1.87592888967883));
#30969=CARTESIAN_POINT('Ctrl Pts',(-0.765990708546091,1.,-1.86981398314341));
#30970=CARTESIAN_POINT('Ctrl Pts',(-0.765891519092547,1.,-1.86372027063312));
#30971=CARTESIAN_POINT('Ctrl Pts',(-0.765744212909318,1.,-1.85764741390394));
#30972=CARTESIAN_POINT('Ctrl Pts',(-0.765545710619062,1.,-1.85158945130063));
#30973=CARTESIAN_POINT('Ctrl Pts',(-0.765291664862029,1.,-1.84553698875924));
#30974=CARTESIAN_POINT('Ctrl Pts',(-0.764978057881737,1.,-1.83948181064835));
#30975=CARTESIAN_POINT('Ctrl Pts',(-0.764602549687853,1.,-1.83342077227142));
#30976=CARTESIAN_POINT('Ctrl Pts',(-0.764165902605995,1.,-1.82735991200065));
#30977=CARTESIAN_POINT('Ctrl Pts',(-0.763673465462726,1.,-1.82131873145266));
#30978=CARTESIAN_POINT('Ctrl Pts',(-0.763132003836634,1.,-1.8153211840553));
#30979=CARTESIAN_POINT('Ctrl Pts',(-0.762546129463938,1.,-1.80938551463965));
#30980=CARTESIAN_POINT('Ctrl Pts',(-0.761915336443547,1.,-1.80351583877342));
#30981=CARTESIAN_POINT('Ctrl Pts',(-0.761229695230558,1.,-1.79768986997783));
#30982=CARTESIAN_POINT('Ctrl Pts',(-0.760469555880749,1.,-1.7918581561088));
#30983=CARTESIAN_POINT('Ctrl Pts',(-0.759614401110189,1.,-1.78596964884604));
#30984=CARTESIAN_POINT('Ctrl Pts',(-0.758650626677518,1.,-1.77999411220945));
#30985=CARTESIAN_POINT('Ctrl Pts',(-0.757578264077029,1.,-1.77394167108292));
#30986=CARTESIAN_POINT('Ctrl Pts',(-0.75642189602781,1.,-1.76789396002998));
#30987=CARTESIAN_POINT('Ctrl Pts',(-0.755220979974461,1.,-1.76197817240128));
#30988=CARTESIAN_POINT('Ctrl Pts',(-0.754009254027829,1.,-1.75631083600019));
#30989=CARTESIAN_POINT('Ctrl Pts',(-0.752797683531314,1.,-1.75095139468794));
#30990=CARTESIAN_POINT('Ctrl Pts',(-0.751555614164482,1.,-1.74585086852502));
#30991=CARTESIAN_POINT('Ctrl Pts',(-0.750193435981249,1.,-1.74080458267114));
#30992=CARTESIAN_POINT('Ctrl Pts',(-0.74858246295687,1.,-1.7355035168033));
#30993=CARTESIAN_POINT('Ctrl Pts',(-0.746574710097752,1.,-1.72958533647714));
#30994=CARTESIAN_POINT('Ctrl Pts',(-0.744021445433093,1.,-1.72268229916769));
#30995=CARTESIAN_POINT('Ctrl Pts',(-0.74079516202821,1.,-1.71447789751001));
#30996=CARTESIAN_POINT('Ctrl Pts',(-0.736799665716932,1.,-1.70473309004249));
#30997=CARTESIAN_POINT('Ctrl Pts',(-0.731963238685357,1.,-1.69326921972915));
#30998=CARTESIAN_POINT('Ctrl Pts',(-0.726235967982445,1.,-1.67996158451922));
#30999=CARTESIAN_POINT('Ctrl Pts',(-0.71958543378795,1.,-1.66472880551777));
#31000=CARTESIAN_POINT('Ctrl Pts',(-0.711993139340447,1.,-1.64752408828442));
#31001=CARTESIAN_POINT('Ctrl Pts',(-0.705159151977294,1.,-1.6321654166204));
#31002=CARTESIAN_POINT('Ctrl Pts',(-0.699605146398837,1.,-1.61974673471117));
#31003=CARTESIAN_POINT('Ctrl Pts',(-0.69571209787897,1.,-1.61106790957619));
#31004=CARTESIAN_POINT('Ctrl Pts',(-0.693717979106305,1.,-1.60662857109684));
#31005=CARTESIAN_POINT('',(-0.745574324794401,0.,-2.0698113262342));
#31006=CARTESIAN_POINT('Origin',(-0.61342227326009,0.,-2.11275013067528));
#31007=CARTESIAN_POINT('',(-0.61342227326009,1.,-2.11275013067528));
#31008=CARTESIAN_POINT('',(-0.745574324794401,1.,-2.0698113262342));
#31009=CARTESIAN_POINT('',(-0.61342227326009,0.,-2.11275013067528));
#31010=CARTESIAN_POINT('Ctrl Pts',(-0.383122945602004,-1.,-1.7075470150345));
#31011=CARTESIAN_POINT('Ctrl Pts',(-0.383122945602004,1.,-1.7075470150345));
#31012=CARTESIAN_POINT('Ctrl Pts',(-0.384119047315542,-1.,-1.71231062891958));
#31013=CARTESIAN_POINT('Ctrl Pts',(-0.384119047315542,1.,-1.71231062891958));
#31014=CARTESIAN_POINT('Ctrl Pts',(-0.38607079032701,-1.,-1.72162022246158));
#31015=CARTESIAN_POINT('Ctrl Pts',(-0.38607079032701,1.,-1.72162022246158));
#31016=CARTESIAN_POINT('Ctrl Pts',(-0.388877023509191,-1.,-1.7349317097561));
#31017=CARTESIAN_POINT('Ctrl Pts',(-0.388877023509191,1.,-1.7349317097561));
#31018=CARTESIAN_POINT('Ctrl Pts',(-0.392375812294307,-1.,-1.75137405313962));
#31019=CARTESIAN_POINT('Ctrl Pts',(-0.392375812294307,1.,-1.75137405313962));
#31020=CARTESIAN_POINT('Ctrl Pts',(-0.39634619612042,-1.,-1.7697556004756));
#31021=CARTESIAN_POINT('Ctrl Pts',(-0.39634619612042,1.,-1.7697556004756));
#31022=CARTESIAN_POINT('Ctrl Pts',(-0.39991940378308,-1.,-1.78598826347533));
#31023=CARTESIAN_POINT('Ctrl Pts',(-0.39991940378308,1.,-1.78598826347533));
#31024=CARTESIAN_POINT('Ctrl Pts',(-0.403107976170441,-1.,-1.80012077176221));
#31025=CARTESIAN_POINT('Ctrl Pts',(-0.403107976170441,1.,-1.80012077176221));
#31026=CARTESIAN_POINT('Ctrl Pts',(-0.405933518411838,-1.,-1.81223801813988));
#31027=CARTESIAN_POINT('Ctrl Pts',(-0.405933518411838,1.,-1.81223801813988));
#31028=CARTESIAN_POINT('Ctrl Pts',(-0.408428948108533,-1.,-1.8224702267854));
#31029=CARTESIAN_POINT('Ctrl Pts',(-0.408428948108533,1.,-1.8224702267854));
#31030=CARTESIAN_POINT('Ctrl Pts',(-0.410641256301675,-1.,-1.83100408895216));
#31031=CARTESIAN_POINT('Ctrl Pts',(-0.410641256301675,1.,-1.83100408895216));
#31032=CARTESIAN_POINT('Ctrl Pts',(-0.412633125322162,-1.,-1.83808953475839));
#31033=CARTESIAN_POINT('Ctrl Pts',(-0.412633125322162,1.,-1.83808953475839));
#31034=CARTESIAN_POINT('Ctrl Pts',(-0.41448743825434,-1.,-1.8440575707371));
#31035=CARTESIAN_POINT('Ctrl Pts',(-0.41448743825434,1.,-1.8440575707371));
#31036=CARTESIAN_POINT('Ctrl Pts',(-0.416300022038864,-1.,-1.84929312929882));
#31037=CARTESIAN_POINT('Ctrl Pts',(-0.416300022038864,1.,-1.84929312929882));
#31038=CARTESIAN_POINT('Ctrl Pts',(-0.418164129143534,-1.,-1.85417632856234));
#31039=CARTESIAN_POINT('Ctrl Pts',(-0.418164129143534,1.,-1.85417632856234));
#31040=CARTESIAN_POINT('Ctrl Pts',(-0.420157287975619,-1.,-1.85903281096686));
#31041=CARTESIAN_POINT('Ctrl Pts',(-0.420157287975619,1.,-1.85903281096686));
#31042=CARTESIAN_POINT('Ctrl Pts',(-0.422327307418275,-1.,-1.86408083334028));
#31043=CARTESIAN_POINT('Ctrl Pts',(-0.422327307418275,1.,-1.86408083334028));
#31044=CARTESIAN_POINT('Ctrl Pts',(-0.424678177291359,-1.,-1.86937803944323));
#31045=CARTESIAN_POINT('Ctrl Pts',(-0.424678177291359,1.,-1.86937803944323));
#31046=CARTESIAN_POINT('Ctrl Pts',(-0.427183828519102,-1.,-1.87486989291484));
#31047=CARTESIAN_POINT('Ctrl Pts',(-0.427183828519102,1.,-1.87486989291484));
#31048=CARTESIAN_POINT('Ctrl Pts',(-0.429803062482344,-1.,-1.88044229001832));
#31049=CARTESIAN_POINT('Ctrl Pts',(-0.429803062482344,1.,-1.88044229001832));
#31050=CARTESIAN_POINT('Ctrl Pts',(-0.432493038548748,-1.,-1.88596913666793));
#31051=CARTESIAN_POINT('Ctrl Pts',(-0.432493038548748,1.,-1.88596913666793));
#31052=CARTESIAN_POINT('Ctrl Pts',(-0.435225660963383,-1.,-1.89136993975504));
#31053=CARTESIAN_POINT('Ctrl Pts',(-0.435225660963383,1.,-1.89136993975504));
#31054=CARTESIAN_POINT('Ctrl Pts',(-0.437995003948244,-1.,-1.89663648956466));
#31055=CARTESIAN_POINT('Ctrl Pts',(-0.437995003948244,1.,-1.89663648956466));
#31056=CARTESIAN_POINT('Ctrl Pts',(-0.440807833704038,-1.,-1.90180124389086));
#31057=CARTESIAN_POINT('Ctrl Pts',(-0.440807833704038,1.,-1.90180124389086));
#31058=CARTESIAN_POINT('Ctrl Pts',(-0.443677556849151,-1.,-1.90691756144898));
#31059=CARTESIAN_POINT('Ctrl Pts',(-0.443677556849151,1.,-1.90691756144898));
#31060=CARTESIAN_POINT('Ctrl Pts',(-0.446617343485711,-1.,-1.9120369998112));
#31061=CARTESIAN_POINT('Ctrl Pts',(-0.446617343485711,1.,-1.9120369998112));
#31062=CARTESIAN_POINT('Ctrl Pts',(-0.449632260106662,-1.,-1.91718342555755));
#31063=CARTESIAN_POINT('Ctrl Pts',(-0.449632260106662,1.,-1.91718342555755));
#31064=CARTESIAN_POINT('Ctrl Pts',(-0.452719478359432,-1.,-1.92235380648502));
#31065=CARTESIAN_POINT('Ctrl Pts',(-0.452719478359432,1.,-1.92235380648502));
#31066=CARTESIAN_POINT('Ctrl Pts',(-0.455872005174371,-1.,-1.92753067150476));
#31067=CARTESIAN_POINT('Ctrl Pts',(-0.455872005174371,1.,-1.92753067150476));
#31068=CARTESIAN_POINT('Ctrl Pts',(-0.459081234547926,-1.,-1.93269066517934));
#31069=CARTESIAN_POINT('Ctrl Pts',(-0.459081234547926,1.,-1.93269066517934));
#31070=CARTESIAN_POINT('Ctrl Pts',(-0.462340031009056,-1.,-1.93781486640821));
#31071=CARTESIAN_POINT('Ctrl Pts',(-0.462340031009056,1.,-1.93781486640821));
#31072=CARTESIAN_POINT('Ctrl Pts',(-0.46564546202603,-1.,-1.9428979419619));
#31073=CARTESIAN_POINT('Ctrl Pts',(-0.46564546202603,1.,-1.9428979419619));
#31074=CARTESIAN_POINT('Ctrl Pts',(-0.468997482913135,-1.,-1.94794381136514));
#31075=CARTESIAN_POINT('Ctrl Pts',(-0.468997482913135,1.,-1.94794381136514));
#31076=CARTESIAN_POINT('Ctrl Pts',(-0.472397672264072,-1.,-1.95296148278133));
#31077=CARTESIAN_POINT('Ctrl Pts',(-0.472397672264072,1.,-1.95296148278133));
#31078=CARTESIAN_POINT('Ctrl Pts',(-0.475848034683176,-1.,-1.95796111148177));
#31079=CARTESIAN_POINT('Ctrl Pts',(-0.475848034683176,1.,-1.95796111148177));
#31080=CARTESIAN_POINT('Ctrl Pts',(-0.479349583074855,-1.,-1.96294933055943));
#31081=CARTESIAN_POINT('Ctrl Pts',(-0.479349583074855,1.,-1.96294933055943));
#31082=CARTESIAN_POINT('Ctrl Pts',(-0.482901662120691,-1.,-1.96792703422362));
#31083=CARTESIAN_POINT('Ctrl Pts',(-0.482901662120691,1.,-1.96792703422362));
#31084=CARTESIAN_POINT('Ctrl Pts',(-0.486502692907659,-1.,-1.97289186263272));
#31085=CARTESIAN_POINT('Ctrl Pts',(-0.486502692907659,1.,-1.97289186263272));
#31086=CARTESIAN_POINT('Ctrl Pts',(-0.490150627860952,-1.,-1.97783973019229));
#31087=CARTESIAN_POINT('Ctrl Pts',(-0.490150627860952,1.,-1.97783973019229));
#31088=CARTESIAN_POINT('Ctrl Pts',(-0.493843476541495,-1.,-1.98276658761821));
#31089=CARTESIAN_POINT('Ctrl Pts',(-0.493843476541495,1.,-1.98276658761821));
#31090=CARTESIAN_POINT('Ctrl Pts',(-0.497579909545574,-1.,-1.98767044752932));
#31091=CARTESIAN_POINT('Ctrl Pts',(-0.497579909545574,1.,-1.98767044752932));
#31092=CARTESIAN_POINT('Ctrl Pts',(-0.501359287727146,-1.,-1.99255149126155));
#31093=CARTESIAN_POINT('Ctrl Pts',(-0.501359287727146,1.,-1.99255149126155));
#31094=CARTESIAN_POINT('Ctrl Pts',(-0.505181361323026,-1.,-1.99741107463572));
#31095=CARTESIAN_POINT('Ctrl Pts',(-0.505181361323026,1.,-1.99741107463572));
#31096=CARTESIAN_POINT('Ctrl Pts',(-0.509046069886157,-1.,-2.00225107134734));
#31097=CARTESIAN_POINT('Ctrl Pts',(-0.509046069886157,1.,-2.00225107134734));
#31098=CARTESIAN_POINT('Ctrl Pts',(-0.512953306961792,-1.,-2.00707309946949));
#31099=CARTESIAN_POINT('Ctrl Pts',(-0.512953306961792,1.,-2.00707309946949));
#31100=CARTESIAN_POINT('Ctrl Pts',(-0.516902681728687,-1.,-2.01187773939242));
#31101=CARTESIAN_POINT('Ctrl Pts',(-0.516902681728687,1.,-2.01187773939242));
#31102=CARTESIAN_POINT('Ctrl Pts',(-0.52089359039937,-1.,-2.01666477917286));
#31103=CARTESIAN_POINT('Ctrl Pts',(-0.52089359039937,1.,-2.01666477917286));
#31104=CARTESIAN_POINT('Ctrl Pts',(-0.524925318333476,-1.,-2.02143356304698));
#31105=CARTESIAN_POINT('Ctrl Pts',(-0.524925318333476,1.,-2.02143356304698));
#31106=CARTESIAN_POINT('Ctrl Pts',(-0.528997127241914,-1.,-2.0261832908329));
#31107=CARTESIAN_POINT('Ctrl Pts',(-0.528997127241914,1.,-2.0261832908329));
#31108=CARTESIAN_POINT('Ctrl Pts',(-0.533108355132977,-1.,-2.03091336214426));
#31109=CARTESIAN_POINT('Ctrl Pts',(-0.533108355132977,1.,-2.03091336214426));
#31110=CARTESIAN_POINT('Ctrl Pts',(-0.537258489833262,-1.,-2.03562362954037));
#31111=CARTESIAN_POINT('Ctrl Pts',(-0.537258489833262,1.,-2.03562362954037));
#31112=CARTESIAN_POINT('Ctrl Pts',(-0.541447120615659,-1.,-2.04031422690527));
#31113=CARTESIAN_POINT('Ctrl Pts',(-0.541447120615659,1.,-2.04031422690527));
#31114=CARTESIAN_POINT('Ctrl Pts',(-0.54567390381743,-1.,-2.04498544714588));
#31115=CARTESIAN_POINT('Ctrl Pts',(-0.54567390381743,1.,-2.04498544714588));
#31116=CARTESIAN_POINT('Ctrl Pts',(-0.549938525150295,-1.,-2.04963761077958));
#31117=CARTESIAN_POINT('Ctrl Pts',(-0.549938525150295,1.,-2.04963761077958));
#31118=CARTESIAN_POINT('Ctrl Pts',(-0.554240657463906,-1.,-2.05427091604413));
#31119=CARTESIAN_POINT('Ctrl Pts',(-0.554240657463906,1.,-2.05427091604413));
#31120=CARTESIAN_POINT('Ctrl Pts',(-0.558579940185151,-1.,-2.05888537756462));
#31121=CARTESIAN_POINT('Ctrl Pts',(-0.558579940185151,1.,-2.05888537756462));
#31122=CARTESIAN_POINT('Ctrl Pts',(-0.562955993082261,-1.,-2.06348090160589));
#31123=CARTESIAN_POINT('Ctrl Pts',(-0.562955993082261,1.,-2.06348090160589));
#31124=CARTESIAN_POINT('Ctrl Pts',(-0.567368421181087,-1.,-2.06805732997334));
#31125=CARTESIAN_POINT('Ctrl Pts',(-0.567368421181087,1.,-2.06805732997334));
#31126=CARTESIAN_POINT('Ctrl Pts',(-0.571816823242603,-1.,-2.07261449292824));
#31127=CARTESIAN_POINT('Ctrl Pts',(-0.571816823242603,1.,-2.07261449292824));
#31128=CARTESIAN_POINT('Ctrl Pts',(-0.576300797416844,-1.,-2.07715226767559));
#31129=CARTESIAN_POINT('Ctrl Pts',(-0.576300797416844,1.,-2.07715226767559));
#31130=CARTESIAN_POINT('Ctrl Pts',(-0.580819952108063,-1.,-2.08167059018418));
#31131=CARTESIAN_POINT('Ctrl Pts',(-0.580819952108063,1.,-2.08167059018418));
#31132=CARTESIAN_POINT('Ctrl Pts',(-0.585373918991617,-1.,-2.08616943727951));
#31133=CARTESIAN_POINT('Ctrl Pts',(-0.585373918991617,1.,-2.08616943727951));
#31134=CARTESIAN_POINT('Ctrl Pts',(-0.589962365403406,-1.,-2.09064881812129));
#31135=CARTESIAN_POINT('Ctrl Pts',(-0.589962365403406,1.,-2.09064881812129));
#31136=CARTESIAN_POINT('Ctrl Pts',(-0.594585006052162,-1.,-2.0951087622027));
#31137=CARTESIAN_POINT('Ctrl Pts',(-0.594585006052162,1.,-2.0951087622027));
#31138=CARTESIAN_POINT('Ctrl Pts',(-0.599241616420533,-1.,-2.0995493086477));
#31139=CARTESIAN_POINT('Ctrl Pts',(-0.599241616420533,1.,-2.0995493086477));
#31140=CARTESIAN_POINT('Ctrl Pts',(-0.60393203073603,-1.,-2.10397049886949));
#31141=CARTESIAN_POINT('Ctrl Pts',(-0.60393203073603,1.,-2.10397049886949));
#31142=CARTESIAN_POINT('Ctrl Pts',(-0.607711315454876,-1.,-2.1074919961518));
#31143=CARTESIAN_POINT('Ctrl Pts',(-0.607711315454876,1.,-2.1074919961518));
#31144=CARTESIAN_POINT('Ctrl Pts',(-0.610560911689899,-1.,-2.11012443807238));
#31145=CARTESIAN_POINT('Ctrl Pts',(-0.610560911689899,1.,-2.11012443807238));
#31146=CARTESIAN_POINT('Ctrl Pts',(-0.6124673655618,-1.,-2.11187554259986));
#31147=CARTESIAN_POINT('Ctrl Pts',(-0.6124673655618,1.,-2.11187554259986));
#31148=CARTESIAN_POINT('Ctrl Pts',(-0.61342227326009,-1.,-2.11275013067528));
#31149=CARTESIAN_POINT('Ctrl Pts',(-0.61342227326009,1.,-2.11275013067528));
#31150=CARTESIAN_POINT('',(-0.383122945602004,1.,-1.7075470150345));
#31151=CARTESIAN_POINT('Ctrl Pts',(-0.383122945602004,1.,-1.7075470150345));
#31152=CARTESIAN_POINT('Ctrl Pts',(-0.384119047315542,1.,-1.71231062891958));
#31153=CARTESIAN_POINT('Ctrl Pts',(-0.38607079032701,1.,-1.72162022246158));
#31154=CARTESIAN_POINT('Ctrl Pts',(-0.388877023509191,1.,-1.7349317097561));
#31155=CARTESIAN_POINT('Ctrl Pts',(-0.392375812294307,1.,-1.75137405313962));
#31156=CARTESIAN_POINT('Ctrl Pts',(-0.39634619612042,1.,-1.7697556004756));
#31157=CARTESIAN_POINT('Ctrl Pts',(-0.39991940378308,1.,-1.78598826347533));
#31158=CARTESIAN_POINT('Ctrl Pts',(-0.403107976170441,1.,-1.80012077176221));
#31159=CARTESIAN_POINT('Ctrl Pts',(-0.405933518411838,1.,-1.81223801813988));
#31160=CARTESIAN_POINT('Ctrl Pts',(-0.408428948108533,1.,-1.8224702267854));
#31161=CARTESIAN_POINT('Ctrl Pts',(-0.410641256301675,1.,-1.83100408895216));
#31162=CARTESIAN_POINT('Ctrl Pts',(-0.412633125322162,1.,-1.83808953475839));
#31163=CARTESIAN_POINT('Ctrl Pts',(-0.41448743825434,1.,-1.8440575707371));
#31164=CARTESIAN_POINT('Ctrl Pts',(-0.416300022038864,1.,-1.84929312929882));
#31165=CARTESIAN_POINT('Ctrl Pts',(-0.418164129143534,1.,-1.85417632856234));
#31166=CARTESIAN_POINT('Ctrl Pts',(-0.420157287975619,1.,-1.85903281096686));
#31167=CARTESIAN_POINT('Ctrl Pts',(-0.422327307418275,1.,-1.86408083334028));
#31168=CARTESIAN_POINT('Ctrl Pts',(-0.424678177291359,1.,-1.86937803944323));
#31169=CARTESIAN_POINT('Ctrl Pts',(-0.427183828519102,1.,-1.87486989291484));
#31170=CARTESIAN_POINT('Ctrl Pts',(-0.429803062482344,1.,-1.88044229001832));
#31171=CARTESIAN_POINT('Ctrl Pts',(-0.432493038548748,1.,-1.88596913666793));
#31172=CARTESIAN_POINT('Ctrl Pts',(-0.435225660963383,1.,-1.89136993975504));
#31173=CARTESIAN_POINT('Ctrl Pts',(-0.437995003948244,1.,-1.89663648956466));
#31174=CARTESIAN_POINT('Ctrl Pts',(-0.440807833704038,1.,-1.90180124389086));
#31175=CARTESIAN_POINT('Ctrl Pts',(-0.443677556849151,1.,-1.90691756144898));
#31176=CARTESIAN_POINT('Ctrl Pts',(-0.446617343485711,1.,-1.9120369998112));
#31177=CARTESIAN_POINT('Ctrl Pts',(-0.449632260106662,1.,-1.91718342555755));
#31178=CARTESIAN_POINT('Ctrl Pts',(-0.452719478359432,1.,-1.92235380648502));
#31179=CARTESIAN_POINT('Ctrl Pts',(-0.455872005174371,1.,-1.92753067150476));
#31180=CARTESIAN_POINT('Ctrl Pts',(-0.459081234547926,1.,-1.93269066517934));
#31181=CARTESIAN_POINT('Ctrl Pts',(-0.462340031009056,1.,-1.93781486640821));
#31182=CARTESIAN_POINT('Ctrl Pts',(-0.46564546202603,1.,-1.9428979419619));
#31183=CARTESIAN_POINT('Ctrl Pts',(-0.468997482913135,1.,-1.94794381136514));
#31184=CARTESIAN_POINT('Ctrl Pts',(-0.472397672264072,1.,-1.95296148278133));
#31185=CARTESIAN_POINT('Ctrl Pts',(-0.475848034683176,1.,-1.95796111148177));
#31186=CARTESIAN_POINT('Ctrl Pts',(-0.479349583074855,1.,-1.96294933055943));
#31187=CARTESIAN_POINT('Ctrl Pts',(-0.482901662120691,1.,-1.96792703422362));
#31188=CARTESIAN_POINT('Ctrl Pts',(-0.486502692907659,1.,-1.97289186263272));
#31189=CARTESIAN_POINT('Ctrl Pts',(-0.490150627860952,1.,-1.97783973019229));
#31190=CARTESIAN_POINT('Ctrl Pts',(-0.493843476541495,1.,-1.98276658761821));
#31191=CARTESIAN_POINT('Ctrl Pts',(-0.497579909545574,1.,-1.98767044752932));
#31192=CARTESIAN_POINT('Ctrl Pts',(-0.501359287727146,1.,-1.99255149126155));
#31193=CARTESIAN_POINT('Ctrl Pts',(-0.505181361323026,1.,-1.99741107463572));
#31194=CARTESIAN_POINT('Ctrl Pts',(-0.509046069886157,1.,-2.00225107134734));
#31195=CARTESIAN_POINT('Ctrl Pts',(-0.512953306961792,1.,-2.00707309946949));
#31196=CARTESIAN_POINT('Ctrl Pts',(-0.516902681728687,1.,-2.01187773939242));
#31197=CARTESIAN_POINT('Ctrl Pts',(-0.52089359039937,1.,-2.01666477917286));
#31198=CARTESIAN_POINT('Ctrl Pts',(-0.524925318333476,1.,-2.02143356304698));
#31199=CARTESIAN_POINT('Ctrl Pts',(-0.528997127241914,1.,-2.0261832908329));
#31200=CARTESIAN_POINT('Ctrl Pts',(-0.533108355132977,1.,-2.03091336214426));
#31201=CARTESIAN_POINT('Ctrl Pts',(-0.537258489833262,1.,-2.03562362954037));
#31202=CARTESIAN_POINT('Ctrl Pts',(-0.541447120615659,1.,-2.04031422690527));
#31203=CARTESIAN_POINT('Ctrl Pts',(-0.54567390381743,1.,-2.04498544714588));
#31204=CARTESIAN_POINT('Ctrl Pts',(-0.549938525150295,1.,-2.04963761077958));
#31205=CARTESIAN_POINT('Ctrl Pts',(-0.554240657463906,1.,-2.05427091604413));
#31206=CARTESIAN_POINT('Ctrl Pts',(-0.558579940185151,1.,-2.05888537756462));
#31207=CARTESIAN_POINT('Ctrl Pts',(-0.562955993082261,1.,-2.06348090160589));
#31208=CARTESIAN_POINT('Ctrl Pts',(-0.567368421181087,1.,-2.06805732997334));
#31209=CARTESIAN_POINT('Ctrl Pts',(-0.571816823242603,1.,-2.07261449292824));
#31210=CARTESIAN_POINT('Ctrl Pts',(-0.576300797416844,1.,-2.07715226767559));
#31211=CARTESIAN_POINT('Ctrl Pts',(-0.580819952108063,1.,-2.08167059018418));
#31212=CARTESIAN_POINT('Ctrl Pts',(-0.585373918991617,1.,-2.08616943727951));
#31213=CARTESIAN_POINT('Ctrl Pts',(-0.589962365403406,1.,-2.09064881812129));
#31214=CARTESIAN_POINT('Ctrl Pts',(-0.594585006052162,1.,-2.0951087622027));
#31215=CARTESIAN_POINT('Ctrl Pts',(-0.599241616420533,1.,-2.0995493086477));
#31216=CARTESIAN_POINT('Ctrl Pts',(-0.60393203073603,1.,-2.10397049886949));
#31217=CARTESIAN_POINT('Ctrl Pts',(-0.607711315454876,1.,-2.1074919961518));
#31218=CARTESIAN_POINT('Ctrl Pts',(-0.610560911689899,1.,-2.11012443807238));
#31219=CARTESIAN_POINT('Ctrl Pts',(-0.6124673655618,1.,-2.11187554259986));
#31220=CARTESIAN_POINT('Ctrl Pts',(-0.61342227326009,1.,-2.11275013067528));
#31221=CARTESIAN_POINT('',(-0.383122945602003,0.,-1.7075470150345));
#31222=CARTESIAN_POINT('Origin',(0.,0.,0.));
#31223=CARTESIAN_POINT('',(-0.163289472382896,1.,-1.74236521665491));
#31224=CARTESIAN_POINT('Origin',(0.,1.,0.));
#31225=CARTESIAN_POINT('',(-0.163289472382896,0.,-1.74236521665491));
#31226=CARTESIAN_POINT('Ctrl Pts',(-0.0694764450219581,-1.,-2.19890268624765));
#31227=CARTESIAN_POINT('Ctrl Pts',(-0.0694764450219581,1.,-2.19890268624765));
#31228=CARTESIAN_POINT('Ctrl Pts',(-0.070114353632549,-1.,-2.19777582085423));
#31229=CARTESIAN_POINT('Ctrl Pts',(-0.070114353632549,1.,-2.19777582085423));
#31230=CARTESIAN_POINT('Ctrl Pts',(-0.0713863779526154,-1.,-2.19552129484002));
#31231=CARTESIAN_POINT('Ctrl Pts',(-0.0713863779526154,1.,-2.19552129484002));
#31232=CARTESIAN_POINT('Ctrl Pts',(-0.0732830357306725,-1.,-2.19213712013662));
#31233=CARTESIAN_POINT('Ctrl Pts',(-0.0732830357306725,1.,-2.19213712013662));
#31234=CARTESIAN_POINT('Ctrl Pts',(-0.0757891465836148,-1.,-2.1876201139953));
#31235=CARTESIAN_POINT('Ctrl Pts',(-0.0757891465836148,1.,-2.1876201139953));
#31236=CARTESIAN_POINT('Ctrl Pts',(-0.0788837727685243,-1.,-2.18196589448887));
#31237=CARTESIAN_POINT('Ctrl Pts',(-0.0788837727685243,1.,-2.18196589448887));
#31238=CARTESIAN_POINT('Ctrl Pts',(-0.0819402680872765,-1.,-2.176303712113));
#31239=CARTESIAN_POINT('Ctrl Pts',(-0.0819402680872765,1.,-2.176303712113));
#31240=CARTESIAN_POINT('Ctrl Pts',(-0.0849584620835372,-1.,-2.17063357870952));
#31241=CARTESIAN_POINT('Ctrl Pts',(-0.0849584620835372,1.,-2.17063357870952));
#31242=CARTESIAN_POINT('Ctrl Pts',(-0.0879381291386923,-1.,-2.16495552645014));
#31243=CARTESIAN_POINT('Ctrl Pts',(-0.0879381291386923,1.,-2.16495552645014));
#31244=CARTESIAN_POINT('Ctrl Pts',(-0.0908789888107265,-1.,-2.15926961544516));
#31245=CARTESIAN_POINT('Ctrl Pts',(-0.0908789888107265,1.,-2.15926961544516));
#31246=CARTESIAN_POINT('Ctrl Pts',(-0.0937807218867643,-1.,-2.1535759397817));
#31247=CARTESIAN_POINT('Ctrl Pts',(-0.0937807218867643,1.,-2.1535759397817));
#31248=CARTESIAN_POINT('Ctrl Pts',(-0.0966429852305459,-1.,-2.14787463531795));
#31249=CARTESIAN_POINT('Ctrl Pts',(-0.0966429852305459,1.,-2.14787463531795));
#31250=CARTESIAN_POINT('Ctrl Pts',(-0.0994654261990915,-1.,-2.14216588396025));
#31251=CARTESIAN_POINT('Ctrl Pts',(-0.0994654261990915,1.,-2.14216588396025));
#31252=CARTESIAN_POINT('Ctrl Pts',(-0.1022477005561,-1.,-2.13644992667165));
#31253=CARTESIAN_POINT('Ctrl Pts',(-0.1022477005561,1.,-2.13644992667165));
#31254=CARTESIAN_POINT('Ctrl Pts',(-0.104989479152739,-1.,-2.13072704887293));
#31255=CARTESIAN_POINT('Ctrl Pts',(-0.104989479152739,1.,-2.13072704887293));
#31256=CARTESIAN_POINT('Ctrl Pts',(-0.10769043523109,-1.,-2.12499752307));
#31257=CARTESIAN_POINT('Ctrl Pts',(-0.10769043523109,1.,-2.12499752307));
#31258=CARTESIAN_POINT('Ctrl Pts',(-0.110350236135025,-1.,-2.11926155590865));
#31259=CARTESIAN_POINT('Ctrl Pts',(-0.110350236135025,1.,-2.11926155590865));
#31260=CARTESIAN_POINT('Ctrl Pts',(-0.112968534419737,-1.,-2.11351924490306));
#31261=CARTESIAN_POINT('Ctrl Pts',(-0.112968534419737,1.,-2.11351924490306));
#31262=CARTESIAN_POINT('Ctrl Pts',(-0.115544957687926,-1.,-2.10777050261309));
#31263=CARTESIAN_POINT('Ctrl Pts',(-0.115544957687926,1.,-2.10777050261309));
#31264=CARTESIAN_POINT('Ctrl Pts',(-0.118079107988355,-1.,-2.102015121329));
#31265=CARTESIAN_POINT('Ctrl Pts',(-0.118079107988355,1.,-2.102015121329));
#31266=CARTESIAN_POINT('Ctrl Pts',(-0.120570567965122,-1.,-2.0962529286773));
#31267=CARTESIAN_POINT('Ctrl Pts',(-0.120570567965122,1.,-2.0962529286773));
#31268=CARTESIAN_POINT('Ctrl Pts',(-0.123018905621083,-1.,-2.09048392424825));
#31269=CARTESIAN_POINT('Ctrl Pts',(-0.123018905621083,1.,-2.09048392424825));
#31270=CARTESIAN_POINT('Ctrl Pts',(-0.125423679412061,-1.,-2.08470840653643));
#31271=CARTESIAN_POINT('Ctrl Pts',(-0.125423679412061,1.,-2.08470840653643));
#31272=CARTESIAN_POINT('Ctrl Pts',(-0.12778444527612,-1.,-2.07892715110987));
#31273=CARTESIAN_POINT('Ctrl Pts',(-0.12778444527612,1.,-2.07892715110987));
#31274=CARTESIAN_POINT('Ctrl Pts',(-0.130100748328403,-1.,-2.07314114713063));
#31275=CARTESIAN_POINT('Ctrl Pts',(-0.130100748328403,1.,-2.07314114713063));
#31276=CARTESIAN_POINT('Ctrl Pts',(-0.13237211154771,-1.,-2.06735123910326));
#31277=CARTESIAN_POINT('Ctrl Pts',(-0.13237211154771,1.,-2.06735123910326));
#31278=CARTESIAN_POINT('Ctrl Pts',(-0.134598026192106,-1.,-2.06155781517842));
#31279=CARTESIAN_POINT('Ctrl Pts',(-0.134598026192106,1.,-2.06155781517842));
#31280=CARTESIAN_POINT('Ctrl Pts',(-0.136777941218044,-1.,-2.05576044414264));
#31281=CARTESIAN_POINT('Ctrl Pts',(-0.136777941218044,1.,-2.05576044414264));
#31282=CARTESIAN_POINT('Ctrl Pts',(-0.138911255368966,-1.,-2.04995762001328));
#31283=CARTESIAN_POINT('Ctrl Pts',(-0.138911255368966,1.,-2.04995762001328));
#31284=CARTESIAN_POINT('Ctrl Pts',(-0.140997332152546,-1.,-2.04414757947916));
#31285=CARTESIAN_POINT('Ctrl Pts',(-0.140997332152546,1.,-2.04414757947916));
#31286=CARTESIAN_POINT('Ctrl Pts',(-0.143035515058209,-1.,-2.03832911025912));
#31287=CARTESIAN_POINT('Ctrl Pts',(-0.143035515058209,1.,-2.03832911025912));
#31288=CARTESIAN_POINT('Ctrl Pts',(-0.145025140186057,-1.,-2.03250223739942));
#31289=CARTESIAN_POINT('Ctrl Pts',(-0.145025140186057,1.,-2.03250223739942));
#31290=CARTESIAN_POINT('Ctrl Pts',(-0.146965557332583,-1.,-2.02666926182017));
#31291=CARTESIAN_POINT('Ctrl Pts',(-0.146965557332583,1.,-2.02666926182017));
#31292=CARTESIAN_POINT('Ctrl Pts',(-0.148856124775337,-1.,-2.02083464969894));
#31293=CARTESIAN_POINT('Ctrl Pts',(-0.148856124775337,1.,-2.02083464969894));
#31294=CARTESIAN_POINT('Ctrl Pts',(-0.150696157673078,-1.,-2.01500291940238));
#31295=CARTESIAN_POINT('Ctrl Pts',(-0.150696157673078,1.,-2.01500291940238));
#31296=CARTESIAN_POINT('Ctrl Pts',(-0.15248488362145,-1.,-2.00917680318424));
#31297=CARTESIAN_POINT('Ctrl Pts',(-0.15248488362145,1.,-2.00917680318424));
#31298=CARTESIAN_POINT('Ctrl Pts',(-0.154221403049722,-1.,-2.00335565310543));
#31299=CARTESIAN_POINT('Ctrl Pts',(-0.154221403049722,1.,-2.00335565310543));
#31300=CARTESIAN_POINT('Ctrl Pts',(-0.155904629548783,-1.,-1.99753284771497));
#31301=CARTESIAN_POINT('Ctrl Pts',(-0.155904629548783,1.,-1.99753284771497));
#31302=CARTESIAN_POINT('Ctrl Pts',(-0.157533331459227,-1.,-1.99169810931908));
#31303=CARTESIAN_POINT('Ctrl Pts',(-0.157533331459227,1.,-1.99169810931908));
#31304=CARTESIAN_POINT('Ctrl Pts',(-0.159106226437299,-1.,-1.98584238283292));
#31305=CARTESIAN_POINT('Ctrl Pts',(-0.159106226437299,1.,-1.98584238283292));
#31306=CARTESIAN_POINT('Ctrl Pts',(-0.160622060784611,-1.,-1.97996195437559));
#31307=CARTESIAN_POINT('Ctrl Pts',(-0.160622060784611,1.,-1.97996195437559));
#31308=CARTESIAN_POINT('Ctrl Pts',(-0.162079693556289,-1.,-1.97406280235188));
#31309=CARTESIAN_POINT('Ctrl Pts',(-0.162079693556289,1.,-1.97406280235188));
#31310=CARTESIAN_POINT('Ctrl Pts',(-0.163478185457734,-1.,-1.96816512677967));
#31311=CARTESIAN_POINT('Ctrl Pts',(-0.163478185457734,1.,-1.96816512677967));
#31312=CARTESIAN_POINT('Ctrl Pts',(-0.164816568920269,-1.,-1.96229379940136));
#31313=CARTESIAN_POINT('Ctrl Pts',(-0.164816568920269,1.,-1.96229379940136));
#31314=CARTESIAN_POINT('Ctrl Pts',(-0.166093592002812,-1.,-1.9564675971873));
#31315=CARTESIAN_POINT('Ctrl Pts',(-0.166093592002812,1.,-1.9564675971873));
#31316=CARTESIAN_POINT('Ctrl Pts',(-0.167307501784475,-1.,-1.95069027794294));
#31317=CARTESIAN_POINT('Ctrl Pts',(-0.167307501784475,1.,-1.95069027794294));
#31318=CARTESIAN_POINT('Ctrl Pts',(-0.168455741607556,-1.,-1.94493757756931));
#31319=CARTESIAN_POINT('Ctrl Pts',(-0.168455741607556,1.,-1.94493757756931));
#31320=CARTESIAN_POINT('Ctrl Pts',(-0.169534904817491,-1.,-1.93915639211581));
#31321=CARTESIAN_POINT('Ctrl Pts',(-0.169534904817491,1.,-1.93915639211581));
#31322=CARTESIAN_POINT('Ctrl Pts',(-0.170541253116202,-1.,-1.93329183155539));
#31323=CARTESIAN_POINT('Ctrl Pts',(-0.170541253116202,1.,-1.93329183155539));
#31324=CARTESIAN_POINT('Ctrl Pts',(-0.171471191532988,-1.,-1.92731093582036));
#31325=CARTESIAN_POINT('Ctrl Pts',(-0.171471191532988,1.,-1.92731093582036));
#31326=CARTESIAN_POINT('Ctrl Pts',(-0.172321621259514,-1.,-1.9212233439798));
#31327=CARTESIAN_POINT('Ctrl Pts',(-0.172321621259514,1.,-1.9212233439798));
#31328=CARTESIAN_POINT('Ctrl Pts',(-0.173090695383496,-1.,-1.91511429159527));
#31329=CARTESIAN_POINT('Ctrl Pts',(-0.173090695383496,1.,-1.91511429159527));
#31330=CARTESIAN_POINT('Ctrl Pts',(-0.173776635257817,-1.,-1.90911693975267));
#31331=CARTESIAN_POINT('Ctrl Pts',(-0.173776635257817,1.,-1.90911693975267));
#31332=CARTESIAN_POINT('Ctrl Pts',(-0.174375518661085,-1.,-1.90335253862834));
#31333=CARTESIAN_POINT('Ctrl Pts',(-0.174375518661085,1.,-1.90335253862834));
#31334=CARTESIAN_POINT('Ctrl Pts',(-0.174879405091263,-1.,-1.89788101117132));
#31335=CARTESIAN_POINT('Ctrl Pts',(-0.174879405091263,1.,-1.89788101117132));
#31336=CARTESIAN_POINT('Ctrl Pts',(-0.175274276190844,-1.,-1.892646301985));
#31337=CARTESIAN_POINT('Ctrl Pts',(-0.175274276190844,1.,-1.892646301985));
#31338=CARTESIAN_POINT('Ctrl Pts',(-0.175538155840648,-1.,-1.88742606273259));
#31339=CARTESIAN_POINT('Ctrl Pts',(-0.175538155840648,1.,-1.88742606273259));
#31340=CARTESIAN_POINT('Ctrl Pts',(-0.175644148889699,-1.,-1.88188663145367));
#31341=CARTESIAN_POINT('Ctrl Pts',(-0.175644148889699,1.,-1.88188663145367));
#31342=CARTESIAN_POINT('Ctrl Pts',(-0.175563480746485,-1.,-1.87563767773588));
#31343=CARTESIAN_POINT('Ctrl Pts',(-0.175563480746485,1.,-1.87563767773588));
#31344=CARTESIAN_POINT('Ctrl Pts',(-0.175268337590758,-1.,-1.86828349694799));
#31345=CARTESIAN_POINT('Ctrl Pts',(-0.175268337590758,1.,-1.86828349694799));
#31346=CARTESIAN_POINT('Ctrl Pts',(-0.17473525927603,-1.,-1.85948367088837));
#31347=CARTESIAN_POINT('Ctrl Pts',(-0.17473525927603,1.,-1.85948367088837));
#31348=CARTESIAN_POINT('Ctrl Pts',(-0.173946627587731,-1.,-1.8489811319852));
#31349=CARTESIAN_POINT('Ctrl Pts',(-0.173946627587731,1.,-1.8489811319852));
#31350=CARTESIAN_POINT('Ctrl Pts',(-0.1728894428919,-1.,-1.83658380527692));
#31351=CARTESIAN_POINT('Ctrl Pts',(-0.1728894428919,1.,-1.83658380527692));
#31352=CARTESIAN_POINT('Ctrl Pts',(-0.171554770204119,-1.,-1.82215766811545));
#31353=CARTESIAN_POINT('Ctrl Pts',(-0.171554770204119,1.,-1.82215766811545));
#31354=CARTESIAN_POINT('Ctrl Pts',(-0.169936923904608,-1.,-1.80561530629706));
#31355=CARTESIAN_POINT('Ctrl Pts',(-0.169936923904608,1.,-1.80561530629706));
#31356=CARTESIAN_POINT('Ctrl Pts',(-0.168032772805197,-1.,-1.7869064998507));
#31357=CARTESIAN_POINT('Ctrl Pts',(-0.168032772805197,1.,-1.7869064998507));
#31358=CARTESIAN_POINT('Ctrl Pts',(-0.1662793551464,-1.,-1.77018771684844));
#31359=CARTESIAN_POINT('Ctrl Pts',(-0.1662793551464,1.,-1.77018771684844));
#31360=CARTESIAN_POINT('Ctrl Pts',(-0.164834765707158,-1.,-1.75666056638427));
#31361=CARTESIAN_POINT('Ctrl Pts',(-0.164834765707158,1.,-1.75666056638427));
#31362=CARTESIAN_POINT('Ctrl Pts',(-0.163814161002002,-1.,-1.7472034950333));
#31363=CARTESIAN_POINT('Ctrl Pts',(-0.163814161002002,1.,-1.7472034950333));
#31364=CARTESIAN_POINT('Ctrl Pts',(-0.163289472382896,-1.,-1.74236521665491));
#31365=CARTESIAN_POINT('Ctrl Pts',(-0.163289472382896,1.,-1.74236521665491));
#31366=CARTESIAN_POINT('',(-0.0694764450219581,1.,-2.19890268624765));
#31367=CARTESIAN_POINT('Ctrl Pts',(-0.0694764450219581,1.,-2.19890268624765));
#31368=CARTESIAN_POINT('Ctrl Pts',(-0.070114353632549,1.,-2.19777582085423));
#31369=CARTESIAN_POINT('Ctrl Pts',(-0.0713863779526154,1.,-2.19552129484002));
#31370=CARTESIAN_POINT('Ctrl Pts',(-0.0732830357306725,1.,-2.19213712013662));
#31371=CARTESIAN_POINT('Ctrl Pts',(-0.0757891465836148,1.,-2.1876201139953));
#31372=CARTESIAN_POINT('Ctrl Pts',(-0.0788837727685243,1.,-2.18196589448887));
#31373=CARTESIAN_POINT('Ctrl Pts',(-0.0819402680872765,1.,-2.176303712113));
#31374=CARTESIAN_POINT('Ctrl Pts',(-0.0849584620835372,1.,-2.17063357870952));
#31375=CARTESIAN_POINT('Ctrl Pts',(-0.0879381291386923,1.,-2.16495552645014));
#31376=CARTESIAN_POINT('Ctrl Pts',(-0.0908789888107265,1.,-2.15926961544516));
#31377=CARTESIAN_POINT('Ctrl Pts',(-0.0937807218867643,1.,-2.1535759397817));
#31378=CARTESIAN_POINT('Ctrl Pts',(-0.0966429852305459,1.,-2.14787463531795));
#31379=CARTESIAN_POINT('Ctrl Pts',(-0.0994654261990915,1.,-2.14216588396025));
#31380=CARTESIAN_POINT('Ctrl Pts',(-0.1022477005561,1.,-2.13644992667165));
#31381=CARTESIAN_POINT('Ctrl Pts',(-0.104989479152739,1.,-2.13072704887293));
#31382=CARTESIAN_POINT('Ctrl Pts',(-0.10769043523109,1.,-2.12499752307));
#31383=CARTESIAN_POINT('Ctrl Pts',(-0.110350236135025,1.,-2.11926155590865));
#31384=CARTESIAN_POINT('Ctrl Pts',(-0.112968534419737,1.,-2.11351924490306));
#31385=CARTESIAN_POINT('Ctrl Pts',(-0.115544957687926,1.,-2.10777050261309));
#31386=CARTESIAN_POINT('Ctrl Pts',(-0.118079107988355,1.,-2.102015121329));
#31387=CARTESIAN_POINT('Ctrl Pts',(-0.120570567965122,1.,-2.0962529286773));
#31388=CARTESIAN_POINT('Ctrl Pts',(-0.123018905621083,1.,-2.09048392424825));
#31389=CARTESIAN_POINT('Ctrl Pts',(-0.125423679412061,1.,-2.08470840653643));
#31390=CARTESIAN_POINT('Ctrl Pts',(-0.12778444527612,1.,-2.07892715110987));
#31391=CARTESIAN_POINT('Ctrl Pts',(-0.130100748328403,1.,-2.07314114713063));
#31392=CARTESIAN_POINT('Ctrl Pts',(-0.13237211154771,1.,-2.06735123910326));
#31393=CARTESIAN_POINT('Ctrl Pts',(-0.134598026192106,1.,-2.06155781517842));
#31394=CARTESIAN_POINT('Ctrl Pts',(-0.136777941218044,1.,-2.05576044414264));
#31395=CARTESIAN_POINT('Ctrl Pts',(-0.138911255368966,1.,-2.04995762001328));
#31396=CARTESIAN_POINT('Ctrl Pts',(-0.140997332152546,1.,-2.04414757947916));
#31397=CARTESIAN_POINT('Ctrl Pts',(-0.143035515058209,1.,-2.03832911025912));
#31398=CARTESIAN_POINT('Ctrl Pts',(-0.145025140186057,1.,-2.03250223739942));
#31399=CARTESIAN_POINT('Ctrl Pts',(-0.146965557332583,1.,-2.02666926182017));
#31400=CARTESIAN_POINT('Ctrl Pts',(-0.148856124775337,1.,-2.02083464969894));
#31401=CARTESIAN_POINT('Ctrl Pts',(-0.150696157673078,1.,-2.01500291940238));
#31402=CARTESIAN_POINT('Ctrl Pts',(-0.15248488362145,1.,-2.00917680318424));
#31403=CARTESIAN_POINT('Ctrl Pts',(-0.154221403049722,1.,-2.00335565310543));
#31404=CARTESIAN_POINT('Ctrl Pts',(-0.155904629548783,1.,-1.99753284771497));
#31405=CARTESIAN_POINT('Ctrl Pts',(-0.157533331459227,1.,-1.99169810931908));
#31406=CARTESIAN_POINT('Ctrl Pts',(-0.159106226437299,1.,-1.98584238283292));
#31407=CARTESIAN_POINT('Ctrl Pts',(-0.160622060784611,1.,-1.97996195437559));
#31408=CARTESIAN_POINT('Ctrl Pts',(-0.162079693556289,1.,-1.97406280235188));
#31409=CARTESIAN_POINT('Ctrl Pts',(-0.163478185457734,1.,-1.96816512677967));
#31410=CARTESIAN_POINT('Ctrl Pts',(-0.164816568920269,1.,-1.96229379940136));
#31411=CARTESIAN_POINT('Ctrl Pts',(-0.166093592002812,1.,-1.9564675971873));
#31412=CARTESIAN_POINT('Ctrl Pts',(-0.167307501784475,1.,-1.95069027794294));
#31413=CARTESIAN_POINT('Ctrl Pts',(-0.168455741607556,1.,-1.94493757756931));
#31414=CARTESIAN_POINT('Ctrl Pts',(-0.169534904817491,1.,-1.93915639211581));
#31415=CARTESIAN_POINT('Ctrl Pts',(-0.170541253116202,1.,-1.93329183155539));
#31416=CARTESIAN_POINT('Ctrl Pts',(-0.171471191532988,1.,-1.92731093582036));
#31417=CARTESIAN_POINT('Ctrl Pts',(-0.172321621259514,1.,-1.9212233439798));
#31418=CARTESIAN_POINT('Ctrl Pts',(-0.173090695383496,1.,-1.91511429159527));
#31419=CARTESIAN_POINT('Ctrl Pts',(-0.173776635257817,1.,-1.90911693975267));
#31420=CARTESIAN_POINT('Ctrl Pts',(-0.174375518661085,1.,-1.90335253862834));
#31421=CARTESIAN_POINT('Ctrl Pts',(-0.174879405091263,1.,-1.89788101117132));
#31422=CARTESIAN_POINT('Ctrl Pts',(-0.175274276190844,1.,-1.892646301985));
#31423=CARTESIAN_POINT('Ctrl Pts',(-0.175538155840648,1.,-1.88742606273259));
#31424=CARTESIAN_POINT('Ctrl Pts',(-0.175644148889699,1.,-1.88188663145367));
#31425=CARTESIAN_POINT('Ctrl Pts',(-0.175563480746485,1.,-1.87563767773588));
#31426=CARTESIAN_POINT('Ctrl Pts',(-0.175268337590758,1.,-1.86828349694799));
#31427=CARTESIAN_POINT('Ctrl Pts',(-0.17473525927603,1.,-1.85948367088837));
#31428=CARTESIAN_POINT('Ctrl Pts',(-0.173946627587731,1.,-1.8489811319852));
#31429=CARTESIAN_POINT('Ctrl Pts',(-0.1728894428919,1.,-1.83658380527692));
#31430=CARTESIAN_POINT('Ctrl Pts',(-0.171554770204119,1.,-1.82215766811545));
#31431=CARTESIAN_POINT('Ctrl Pts',(-0.169936923904608,1.,-1.80561530629706));
#31432=CARTESIAN_POINT('Ctrl Pts',(-0.168032772805197,1.,-1.7869064998507));
#31433=CARTESIAN_POINT('Ctrl Pts',(-0.1662793551464,1.,-1.77018771684844));
#31434=CARTESIAN_POINT('Ctrl Pts',(-0.164834765707158,1.,-1.75666056638427));
#31435=CARTESIAN_POINT('Ctrl Pts',(-0.163814161002002,1.,-1.7472034950333));
#31436=CARTESIAN_POINT('Ctrl Pts',(-0.163289472382896,1.,-1.74236521665491));
#31437=CARTESIAN_POINT('',(-0.0694764450219581,0.,-2.19890268624765));
#31438=CARTESIAN_POINT('Origin',(0.0694764450219584,0.,-2.19890268624765));
#31439=CARTESIAN_POINT('',(0.0694764450219584,1.,-2.19890268624765));
#31440=CARTESIAN_POINT('',(-0.0694764450219581,1.,-2.19890268624765));
#31441=CARTESIAN_POINT('',(0.0694764450219584,0.,-2.19890268624765));
#31442=CARTESIAN_POINT('Ctrl Pts',(0.163289472382896,-1.,-1.74236521665491));
#31443=CARTESIAN_POINT('Ctrl Pts',(0.163289472382896,1.,-1.74236521665491));
#31444=CARTESIAN_POINT('Ctrl Pts',(0.163814161002474,-1.,-1.74720349503904));
#31445=CARTESIAN_POINT('Ctrl Pts',(0.163814161002474,1.,-1.74720349503904));
#31446=CARTESIAN_POINT('Ctrl Pts',(0.164834765708484,-1.,-1.75666056640041));
#31447=CARTESIAN_POINT('Ctrl Pts',(0.164834765708484,1.,-1.75666056640041));
#31448=CARTESIAN_POINT('Ctrl Pts',(0.166279355148738,-1.,-1.77018771687692));
#31449=CARTESIAN_POINT('Ctrl Pts',(0.166279355148738,1.,-1.77018771687692));
#31450=CARTESIAN_POINT('Ctrl Pts',(0.16803277280837,-1.,-1.78690649988931));
#31451=CARTESIAN_POINT('Ctrl Pts',(0.16803277280837,1.,-1.78690649988931));
#31452=CARTESIAN_POINT('Ctrl Pts',(0.169936923908078,-1.,-1.80561530633924));
#31453=CARTESIAN_POINT('Ctrl Pts',(0.169936923908078,1.,-1.80561530633924));
#31454=CARTESIAN_POINT('Ctrl Pts',(0.171554770207306,-1.,-1.82215766815414));
#31455=CARTESIAN_POINT('Ctrl Pts',(0.171554770207306,1.,-1.82215766815414));
#31456=CARTESIAN_POINT('Ctrl Pts',(0.17288944289442,-1.,-1.83658380530747));
#31457=CARTESIAN_POINT('Ctrl Pts',(0.17288944289442,1.,-1.83658380530747));
#31458=CARTESIAN_POINT('Ctrl Pts',(0.173946627589401,-1.,-1.84898113200543));
#31459=CARTESIAN_POINT('Ctrl Pts',(0.173946627589401,1.,-1.84898113200543));
#31460=CARTESIAN_POINT('Ctrl Pts',(0.174735259276856,-1.,-1.85948367089838));
#31461=CARTESIAN_POINT('Ctrl Pts',(0.174735259276856,1.,-1.85948367089838));
#31462=CARTESIAN_POINT('Ctrl Pts',(0.175268337590901,-1.,-1.86828349694972));
#31463=CARTESIAN_POINT('Ctrl Pts',(0.175268337590901,1.,-1.86828349694972));
#31464=CARTESIAN_POINT('Ctrl Pts',(0.175563480746205,-1.,-1.87563767773249));
#31465=CARTESIAN_POINT('Ctrl Pts',(0.175563480746205,1.,-1.87563767773249));
#31466=CARTESIAN_POINT('Ctrl Pts',(0.175644148889271,-1.,-1.88188663144846));
#31467=CARTESIAN_POINT('Ctrl Pts',(0.175644148889271,1.,-1.88188663144846));
#31468=CARTESIAN_POINT('Ctrl Pts',(0.175538155840286,-1.,-1.88742606272818));
#31469=CARTESIAN_POINT('Ctrl Pts',(0.175538155840286,1.,-1.88742606272818));
#31470=CARTESIAN_POINT('Ctrl Pts',(0.175274276190664,-1.,-1.89264630198279));
#31471=CARTESIAN_POINT('Ctrl Pts',(0.175274276190664,1.,-1.89264630198279));
#31472=CARTESIAN_POINT('Ctrl Pts',(0.174879405091277,-1.,-1.89788101117148));
#31473=CARTESIAN_POINT('Ctrl Pts',(0.174879405091277,1.,-1.89788101117148));
#31474=CARTESIAN_POINT('Ctrl Pts',(0.174375518661222,-1.,-1.90335253863003));
#31475=CARTESIAN_POINT('Ctrl Pts',(0.174375518661222,1.,-1.90335253863003));
#31476=CARTESIAN_POINT('Ctrl Pts',(0.173776635257984,-1.,-1.90911693975475));
#31477=CARTESIAN_POINT('Ctrl Pts',(0.173776635257984,1.,-1.90911693975475));
#31478=CARTESIAN_POINT('Ctrl Pts',(0.173090695383619,-1.,-1.91511429159681));
#31479=CARTESIAN_POINT('Ctrl Pts',(0.173090695383619,1.,-1.91511429159681));
#31480=CARTESIAN_POINT('Ctrl Pts',(0.172321621259557,-1.,-1.92122334398034));
#31481=CARTESIAN_POINT('Ctrl Pts',(0.172321621259557,1.,-1.92122334398034));
#31482=CARTESIAN_POINT('Ctrl Pts',(0.17147119153296,-1.,-1.92731093582));
#31483=CARTESIAN_POINT('Ctrl Pts',(0.17147119153296,1.,-1.92731093582));
#31484=CARTESIAN_POINT('Ctrl Pts',(0.170541253116136,-1.,-1.93329183155455));
#31485=CARTESIAN_POINT('Ctrl Pts',(0.170541253116136,1.,-1.93329183155455));
#31486=CARTESIAN_POINT('Ctrl Pts',(0.169534904817425,-1.,-1.93915639211497));
#31487=CARTESIAN_POINT('Ctrl Pts',(0.169534904817425,1.,-1.93915639211497));
#31488=CARTESIAN_POINT('Ctrl Pts',(0.168455741607516,-1.,-1.94493757756879));
#31489=CARTESIAN_POINT('Ctrl Pts',(0.168455741607516,1.,-1.94493757756879));
#31490=CARTESIAN_POINT('Ctrl Pts',(0.167307501784469,-1.,-1.95069027794286));
#31491=CARTESIAN_POINT('Ctrl Pts',(0.167307501784469,1.,-1.95069027794286));
#31492=CARTESIAN_POINT('Ctrl Pts',(0.166093592002833,-1.,-1.95646759718755));
#31493=CARTESIAN_POINT('Ctrl Pts',(0.166093592002833,1.,-1.95646759718755));
#31494=CARTESIAN_POINT('Ctrl Pts',(0.1648165689203,-1.,-1.96229379940174));
#31495=CARTESIAN_POINT('Ctrl Pts',(0.1648165689203,1.,-1.96229379940174));
#31496=CARTESIAN_POINT('Ctrl Pts',(0.16347818545776,-1.,-1.96816512678));
#31497=CARTESIAN_POINT('Ctrl Pts',(0.16347818545776,1.,-1.96816512678));
#31498=CARTESIAN_POINT('Ctrl Pts',(0.162079693556302,-1.,-1.97406280235204));
#31499=CARTESIAN_POINT('Ctrl Pts',(0.162079693556302,1.,-1.97406280235204));
#31500=CARTESIAN_POINT('Ctrl Pts',(0.16062206078461,-1.,-1.97996195437557));
#31501=CARTESIAN_POINT('Ctrl Pts',(0.16062206078461,1.,-1.97996195437557));
#31502=CARTESIAN_POINT('Ctrl Pts',(0.159106226437288,-1.,-1.98584238283279));
#31503=CARTESIAN_POINT('Ctrl Pts',(0.159106226437288,1.,-1.98584238283279));
#31504=CARTESIAN_POINT('Ctrl Pts',(0.157533331459215,-1.,-1.99169810931893));
#31505=CARTESIAN_POINT('Ctrl Pts',(0.157533331459215,1.,-1.99169810931893));
#31506=CARTESIAN_POINT('Ctrl Pts',(0.155904629548774,-1.,-1.99753284771487));
#31507=CARTESIAN_POINT('Ctrl Pts',(0.155904629548774,1.,-1.99753284771487));
#31508=CARTESIAN_POINT('Ctrl Pts',(0.154221403049719,-1.,-2.00335565310539));
#31509=CARTESIAN_POINT('Ctrl Pts',(0.154221403049719,1.,-2.00335565310539));
#31510=CARTESIAN_POINT('Ctrl Pts',(0.152484883621452,-1.,-2.00917680318426));
#31511=CARTESIAN_POINT('Ctrl Pts',(0.152484883621452,1.,-2.00917680318426));
#31512=CARTESIAN_POINT('Ctrl Pts',(0.150696157673084,-1.,-2.01500291940243));
#31513=CARTESIAN_POINT('Ctrl Pts',(0.150696157673084,1.,-2.01500291940243));
#31514=CARTESIAN_POINT('Ctrl Pts',(0.148856124775343,-1.,-2.02083464969897));
#31515=CARTESIAN_POINT('Ctrl Pts',(0.148856124775343,1.,-2.02083464969897));
#31516=CARTESIAN_POINT('Ctrl Pts',(0.146965557332586,-1.,-2.02666926182017));
#31517=CARTESIAN_POINT('Ctrl Pts',(0.146965557332586,1.,-2.02666926182017));
#31518=CARTESIAN_POINT('Ctrl Pts',(0.145025140186058,-1.,-2.03250223739941));
#31519=CARTESIAN_POINT('Ctrl Pts',(0.145025140186058,1.,-2.03250223739941));
#31520=CARTESIAN_POINT('Ctrl Pts',(0.143035515058208,-1.,-2.03832911025913));
#31521=CARTESIAN_POINT('Ctrl Pts',(0.143035515058208,1.,-2.03832911025913));
#31522=CARTESIAN_POINT('Ctrl Pts',(0.140997332152545,-1.,-2.04414757947919));
#31523=CARTESIAN_POINT('Ctrl Pts',(0.140997332152545,1.,-2.04414757947919));
#31524=CARTESIAN_POINT('Ctrl Pts',(0.138911255368966,-1.,-2.04995762001333));
#31525=CARTESIAN_POINT('Ctrl Pts',(0.138911255368966,1.,-2.04995762001333));
#31526=CARTESIAN_POINT('Ctrl Pts',(0.136777941218044,-1.,-2.0557604441427));
#31527=CARTESIAN_POINT('Ctrl Pts',(0.136777941218044,1.,-2.0557604441427));
#31528=CARTESIAN_POINT('Ctrl Pts',(0.134598026192107,-1.,-2.06155781517844));
#31529=CARTESIAN_POINT('Ctrl Pts',(0.134598026192107,1.,-2.06155781517844));
#31530=CARTESIAN_POINT('Ctrl Pts',(0.13237211154771,-1.,-2.06735123910319));
#31531=CARTESIAN_POINT('Ctrl Pts',(0.13237211154771,1.,-2.06735123910319));
#31532=CARTESIAN_POINT('Ctrl Pts',(0.1301007483284,-1.,-2.07314114713047));
#31533=CARTESIAN_POINT('Ctrl Pts',(0.1301007483284,1.,-2.07314114713047));
#31534=CARTESIAN_POINT('Ctrl Pts',(0.127784445276116,-1.,-2.07892715110967));
#31535=CARTESIAN_POINT('Ctrl Pts',(0.127784445276116,1.,-2.07892715110967));
#31536=CARTESIAN_POINT('Ctrl Pts',(0.125423679412058,-1.,-2.08470840653628));
#31537=CARTESIAN_POINT('Ctrl Pts',(0.125423679412058,1.,-2.08470840653628));
#31538=CARTESIAN_POINT('Ctrl Pts',(0.123018905621083,-1.,-2.09048392424826));
#31539=CARTESIAN_POINT('Ctrl Pts',(0.123018905621083,1.,-2.09048392424826));
#31540=CARTESIAN_POINT('Ctrl Pts',(0.120570567965129,-1.,-2.09625292867756));
#31541=CARTESIAN_POINT('Ctrl Pts',(0.120570567965129,1.,-2.09625292867756));
#31542=CARTESIAN_POINT('Ctrl Pts',(0.118079107988368,-1.,-2.10201512132945));
#31543=CARTESIAN_POINT('Ctrl Pts',(0.118079107988368,1.,-2.10201512132945));
#31544=CARTESIAN_POINT('Ctrl Pts',(0.11554495768794,-1.,-2.10777050261359));
#31545=CARTESIAN_POINT('Ctrl Pts',(0.11554495768794,1.,-2.10777050261359));
#31546=CARTESIAN_POINT('Ctrl Pts',(0.112968534419746,-1.,-2.11351924490335));
#31547=CARTESIAN_POINT('Ctrl Pts',(0.112968534419746,1.,-2.11351924490335));
#31548=CARTESIAN_POINT('Ctrl Pts',(0.11035023613502,-1.,-2.11926155590849));
#31549=CARTESIAN_POINT('Ctrl Pts',(0.11035023613502,1.,-2.11926155590849));
#31550=CARTESIAN_POINT('Ctrl Pts',(0.107690435231068,-1.,-2.12499752306927));
#31551=CARTESIAN_POINT('Ctrl Pts',(0.107690435231068,1.,-2.12499752306927));
#31552=CARTESIAN_POINT('Ctrl Pts',(0.104989479152703,-1.,-2.1307270488718));
#31553=CARTESIAN_POINT('Ctrl Pts',(0.104989479152703,1.,-2.1307270488718));
#31554=CARTESIAN_POINT('Ctrl Pts',(0.102247700556064,-1.,-2.13644992667052));
#31555=CARTESIAN_POINT('Ctrl Pts',(0.102247700556064,1.,-2.13644992667052));
#31556=CARTESIAN_POINT('Ctrl Pts',(0.0994654261990743,-1.,-2.14216588395974));
#31557=CARTESIAN_POINT('Ctrl Pts',(0.0994654261990743,1.,-2.14216588395974));
#31558=CARTESIAN_POINT('Ctrl Pts',(0.0966429852305689,-1.,-2.14787463531864));
#31559=CARTESIAN_POINT('Ctrl Pts',(0.0966429852305689,1.,-2.14787463531864));
#31560=CARTESIAN_POINT('Ctrl Pts',(0.0937807218868345,-1.,-2.15357593978377));
#31561=CARTESIAN_POINT('Ctrl Pts',(0.0937807218868345,1.,-2.15357593978377));
#31562=CARTESIAN_POINT('Ctrl Pts',(0.0908789888108266,-1.,-2.15926961544808));
#31563=CARTESIAN_POINT('Ctrl Pts',(0.0908789888108266,1.,-2.15926961544808));
#31564=CARTESIAN_POINT('Ctrl Pts',(0.0879381291387823,-1.,-2.16495552645275));
#31565=CARTESIAN_POINT('Ctrl Pts',(0.0879381291387823,1.,-2.16495552645275));
#31566=CARTESIAN_POINT('Ctrl Pts',(0.0849584620835643,-1.,-2.17063357871031));
#31567=CARTESIAN_POINT('Ctrl Pts',(0.0849584620835643,1.,-2.17063357871031));
#31568=CARTESIAN_POINT('Ctrl Pts',(0.0819402680871939,-1.,-2.1763037121106));
#31569=CARTESIAN_POINT('Ctrl Pts',(0.0819402680871939,1.,-2.1763037121106));
#31570=CARTESIAN_POINT('Ctrl Pts',(0.0788837727683228,-1.,-2.18196589448304));
#31571=CARTESIAN_POINT('Ctrl Pts',(0.0788837727683228,1.,-2.18196589448304));
#31572=CARTESIAN_POINT('Ctrl Pts',(0.0757891465833411,-1.,-2.1876201139874));
#31573=CARTESIAN_POINT('Ctrl Pts',(0.0757891465833411,1.,-2.1876201139874));
#31574=CARTESIAN_POINT('Ctrl Pts',(0.0732830357304276,-1.,-2.19213712012956));
#31575=CARTESIAN_POINT('Ctrl Pts',(0.0732830357304276,1.,-2.19213712012956));
#31576=CARTESIAN_POINT('Ctrl Pts',(0.0713863779524627,-1.,-2.19552129483562));
#31577=CARTESIAN_POINT('Ctrl Pts',(0.0713863779524627,1.,-2.19552129483562));
#31578=CARTESIAN_POINT('Ctrl Pts',(0.0701143536324926,-1.,-2.19777582085261));
#31579=CARTESIAN_POINT('Ctrl Pts',(0.0701143536324926,1.,-2.19777582085261));
#31580=CARTESIAN_POINT('Ctrl Pts',(0.0694764450219584,-1.,-2.19890268624765));
#31581=CARTESIAN_POINT('Ctrl Pts',(0.0694764450219584,1.,-2.19890268624765));
#31582=CARTESIAN_POINT('',(0.163289472382896,1.,-1.74236521665491));
#31583=CARTESIAN_POINT('Ctrl Pts',(0.163289472382896,1.,-1.74236521665491));
#31584=CARTESIAN_POINT('Ctrl Pts',(0.163814161002474,1.,-1.74720349503904));
#31585=CARTESIAN_POINT('Ctrl Pts',(0.164834765708484,1.,-1.75666056640041));
#31586=CARTESIAN_POINT('Ctrl Pts',(0.166279355148738,1.,-1.77018771687692));
#31587=CARTESIAN_POINT('Ctrl Pts',(0.16803277280837,1.,-1.78690649988931));
#31588=CARTESIAN_POINT('Ctrl Pts',(0.169936923908078,1.,-1.80561530633924));
#31589=CARTESIAN_POINT('Ctrl Pts',(0.171554770207306,1.,-1.82215766815414));
#31590=CARTESIAN_POINT('Ctrl Pts',(0.17288944289442,1.,-1.83658380530747));
#31591=CARTESIAN_POINT('Ctrl Pts',(0.173946627589401,1.,-1.84898113200543));
#31592=CARTESIAN_POINT('Ctrl Pts',(0.174735259276856,1.,-1.85948367089838));
#31593=CARTESIAN_POINT('Ctrl Pts',(0.175268337590901,1.,-1.86828349694972));
#31594=CARTESIAN_POINT('Ctrl Pts',(0.175563480746205,1.,-1.87563767773249));
#31595=CARTESIAN_POINT('Ctrl Pts',(0.175644148889271,1.,-1.88188663144846));
#31596=CARTESIAN_POINT('Ctrl Pts',(0.175538155840286,1.,-1.88742606272818));
#31597=CARTESIAN_POINT('Ctrl Pts',(0.175274276190664,1.,-1.89264630198279));
#31598=CARTESIAN_POINT('Ctrl Pts',(0.174879405091277,1.,-1.89788101117148));
#31599=CARTESIAN_POINT('Ctrl Pts',(0.174375518661222,1.,-1.90335253863003));
#31600=CARTESIAN_POINT('Ctrl Pts',(0.173776635257984,1.,-1.90911693975475));
#31601=CARTESIAN_POINT('Ctrl Pts',(0.173090695383619,1.,-1.91511429159681));
#31602=CARTESIAN_POINT('Ctrl Pts',(0.172321621259557,1.,-1.92122334398034));
#31603=CARTESIAN_POINT('Ctrl Pts',(0.17147119153296,1.,-1.92731093582));
#31604=CARTESIAN_POINT('Ctrl Pts',(0.170541253116136,1.,-1.93329183155455));
#31605=CARTESIAN_POINT('Ctrl Pts',(0.169534904817425,1.,-1.93915639211497));
#31606=CARTESIAN_POINT('Ctrl Pts',(0.168455741607516,1.,-1.94493757756879));
#31607=CARTESIAN_POINT('Ctrl Pts',(0.167307501784469,1.,-1.95069027794286));
#31608=CARTESIAN_POINT('Ctrl Pts',(0.166093592002833,1.,-1.95646759718755));
#31609=CARTESIAN_POINT('Ctrl Pts',(0.1648165689203,1.,-1.96229379940174));
#31610=CARTESIAN_POINT('Ctrl Pts',(0.16347818545776,1.,-1.96816512678));
#31611=CARTESIAN_POINT('Ctrl Pts',(0.162079693556302,1.,-1.97406280235204));
#31612=CARTESIAN_POINT('Ctrl Pts',(0.16062206078461,1.,-1.97996195437557));
#31613=CARTESIAN_POINT('Ctrl Pts',(0.159106226437288,1.,-1.98584238283279));
#31614=CARTESIAN_POINT('Ctrl Pts',(0.157533331459215,1.,-1.99169810931893));
#31615=CARTESIAN_POINT('Ctrl Pts',(0.155904629548774,1.,-1.99753284771487));
#31616=CARTESIAN_POINT('Ctrl Pts',(0.154221403049719,1.,-2.00335565310539));
#31617=CARTESIAN_POINT('Ctrl Pts',(0.152484883621452,1.,-2.00917680318426));
#31618=CARTESIAN_POINT('Ctrl Pts',(0.150696157673084,1.,-2.01500291940243));
#31619=CARTESIAN_POINT('Ctrl Pts',(0.148856124775343,1.,-2.02083464969897));
#31620=CARTESIAN_POINT('Ctrl Pts',(0.146965557332586,1.,-2.02666926182017));
#31621=CARTESIAN_POINT('Ctrl Pts',(0.145025140186058,1.,-2.03250223739941));
#31622=CARTESIAN_POINT('Ctrl Pts',(0.143035515058208,1.,-2.03832911025913));
#31623=CARTESIAN_POINT('Ctrl Pts',(0.140997332152545,1.,-2.04414757947919));
#31624=CARTESIAN_POINT('Ctrl Pts',(0.138911255368966,1.,-2.04995762001333));
#31625=CARTESIAN_POINT('Ctrl Pts',(0.136777941218044,1.,-2.0557604441427));
#31626=CARTESIAN_POINT('Ctrl Pts',(0.134598026192107,1.,-2.06155781517844));
#31627=CARTESIAN_POINT('Ctrl Pts',(0.13237211154771,1.,-2.06735123910319));
#31628=CARTESIAN_POINT('Ctrl Pts',(0.1301007483284,1.,-2.07314114713047));
#31629=CARTESIAN_POINT('Ctrl Pts',(0.127784445276116,1.,-2.07892715110967));
#31630=CARTESIAN_POINT('Ctrl Pts',(0.125423679412058,1.,-2.08470840653628));
#31631=CARTESIAN_POINT('Ctrl Pts',(0.123018905621083,1.,-2.09048392424826));
#31632=CARTESIAN_POINT('Ctrl Pts',(0.120570567965129,1.,-2.09625292867756));
#31633=CARTESIAN_POINT('Ctrl Pts',(0.118079107988368,1.,-2.10201512132945));
#31634=CARTESIAN_POINT('Ctrl Pts',(0.11554495768794,1.,-2.10777050261359));
#31635=CARTESIAN_POINT('Ctrl Pts',(0.112968534419746,1.,-2.11351924490335));
#31636=CARTESIAN_POINT('Ctrl Pts',(0.11035023613502,1.,-2.11926155590849));
#31637=CARTESIAN_POINT('Ctrl Pts',(0.107690435231068,1.,-2.12499752306927));
#31638=CARTESIAN_POINT('Ctrl Pts',(0.104989479152703,1.,-2.1307270488718));
#31639=CARTESIAN_POINT('Ctrl Pts',(0.102247700556064,1.,-2.13644992667052));
#31640=CARTESIAN_POINT('Ctrl Pts',(0.0994654261990743,1.,-2.14216588395974));
#31641=CARTESIAN_POINT('Ctrl Pts',(0.0966429852305689,1.,-2.14787463531864));
#31642=CARTESIAN_POINT('Ctrl Pts',(0.0937807218868345,1.,-2.15357593978377));
#31643=CARTESIAN_POINT('Ctrl Pts',(0.0908789888108266,1.,-2.15926961544808));
#31644=CARTESIAN_POINT('Ctrl Pts',(0.0879381291387823,1.,-2.16495552645275));
#31645=CARTESIAN_POINT('Ctrl Pts',(0.0849584620835643,1.,-2.17063357871031));
#31646=CARTESIAN_POINT('Ctrl Pts',(0.0819402680871939,1.,-2.1763037121106));
#31647=CARTESIAN_POINT('Ctrl Pts',(0.0788837727683228,1.,-2.18196589448304));
#31648=CARTESIAN_POINT('Ctrl Pts',(0.0757891465833411,1.,-2.1876201139874));
#31649=CARTESIAN_POINT('Ctrl Pts',(0.0732830357304276,1.,-2.19213712012956));
#31650=CARTESIAN_POINT('Ctrl Pts',(0.0713863779524627,1.,-2.19552129483562));
#31651=CARTESIAN_POINT('Ctrl Pts',(0.0701143536324926,1.,-2.19777582085261));
#31652=CARTESIAN_POINT('Ctrl Pts',(0.0694764450219584,1.,-2.19890268624765));
#31653=CARTESIAN_POINT('',(0.163289472382896,0.,-1.74236521665491));
#31654=CARTESIAN_POINT('Origin',(0.,0.,0.));
#31655=CARTESIAN_POINT('',(0.383122945602004,1.,-1.7075470150345));
#31656=CARTESIAN_POINT('Origin',(0.,1.,0.));
#31657=CARTESIAN_POINT('',(0.383122945602004,0.,-1.7075470150345));
#31658=CARTESIAN_POINT('Ctrl Pts',(0.61342227326009,-1.,-2.11275013067528));
#31659=CARTESIAN_POINT('Ctrl Pts',(0.61342227326009,1.,-2.11275013067528));
#31660=CARTESIAN_POINT('Ctrl Pts',(0.61246736556225,-1.,-2.11187554260142));
#31661=CARTESIAN_POINT('Ctrl Pts',(0.61246736556225,1.,-2.11187554260142));
#31662=CARTESIAN_POINT('Ctrl Pts',(0.610560911691113,-1.,-2.11012443807661));
#31663=CARTESIAN_POINT('Ctrl Pts',(0.610560911691113,1.,-2.11012443807661));
#31664=CARTESIAN_POINT('Ctrl Pts',(0.607711315456826,-1.,-2.10749199615859));
#31665=CARTESIAN_POINT('Ctrl Pts',(0.607711315456826,1.,-2.10749199615859));
#31666=CARTESIAN_POINT('Ctrl Pts',(0.603932030738212,-1.,-2.10397049887709));
#31667=CARTESIAN_POINT('Ctrl Pts',(0.603932030738212,1.,-2.10397049887709));
#31668=CARTESIAN_POINT('Ctrl Pts',(0.599241616422144,-1.,-2.09954930865331));
#31669=CARTESIAN_POINT('Ctrl Pts',(0.599241616422144,1.,-2.09954930865331));
#31670=CARTESIAN_POINT('Ctrl Pts',(0.594585006052823,-1.,-2.09510876220501));
#31671=CARTESIAN_POINT('Ctrl Pts',(0.594585006052823,1.,-2.09510876220501));
#31672=CARTESIAN_POINT('Ctrl Pts',(0.589962365403189,-1.,-2.09064881812053));
#31673=CARTESIAN_POINT('Ctrl Pts',(0.589962365403189,1.,-2.09064881812053));
#31674=CARTESIAN_POINT('Ctrl Pts',(0.585373918990895,-1.,-2.086169437277));
#31675=CARTESIAN_POINT('Ctrl Pts',(0.585373918990895,1.,-2.086169437277));
#31676=CARTESIAN_POINT('Ctrl Pts',(0.580819952107256,-1.,-2.08167059018138));
#31677=CARTESIAN_POINT('Ctrl Pts',(0.580819952107256,1.,-2.08167059018138));
#31678=CARTESIAN_POINT('Ctrl Pts',(0.576300797416274,-1.,-2.07715226767361));
#31679=CARTESIAN_POINT('Ctrl Pts',(0.576300797416274,1.,-2.07715226767361));
#31680=CARTESIAN_POINT('Ctrl Pts',(0.571816823242411,-1.,-2.07261449292758));
#31681=CARTESIAN_POINT('Ctrl Pts',(0.571816823242411,1.,-2.07261449292758));
#31682=CARTESIAN_POINT('Ctrl Pts',(0.567368421181229,-1.,-2.06805732997383));
#31683=CARTESIAN_POINT('Ctrl Pts',(0.567368421181229,1.,-2.06805732997383));
#31684=CARTESIAN_POINT('Ctrl Pts',(0.562955993082574,-1.,-2.06348090160697));
#31685=CARTESIAN_POINT('Ctrl Pts',(0.562955993082574,1.,-2.06348090160697));
#31686=CARTESIAN_POINT('Ctrl Pts',(0.558579940185467,-1.,-2.05888537756571));
#31687=CARTESIAN_POINT('Ctrl Pts',(0.558579940185467,1.,-2.05888537756571));
#31688=CARTESIAN_POINT('Ctrl Pts',(0.554240657464109,-1.,-2.05427091604482));
#31689=CARTESIAN_POINT('Ctrl Pts',(0.554240657464109,1.,-2.05427091604482));
#31690=CARTESIAN_POINT('Ctrl Pts',(0.549938525150342,-1.,-2.04963761077974));
#31691=CARTESIAN_POINT('Ctrl Pts',(0.549938525150342,1.,-2.04963761077974));
#31692=CARTESIAN_POINT('Ctrl Pts',(0.545673903817348,-1.,-2.0449854471456));
#31693=CARTESIAN_POINT('Ctrl Pts',(0.545673903817348,1.,-2.0449854471456));
#31694=CARTESIAN_POINT('Ctrl Pts',(0.54144712061552,-1.,-2.0403142269048));
#31695=CARTESIAN_POINT('Ctrl Pts',(0.54144712061552,1.,-2.0403142269048));
#31696=CARTESIAN_POINT('Ctrl Pts',(0.537258489833134,-1.,-2.03562362953993));
#31697=CARTESIAN_POINT('Ctrl Pts',(0.537258489833134,1.,-2.03562362953993));
#31698=CARTESIAN_POINT('Ctrl Pts',(0.533108355132905,-1.,-2.03091336214401));
#31699=CARTESIAN_POINT('Ctrl Pts',(0.533108355132905,1.,-2.03091336214401));
#31700=CARTESIAN_POINT('Ctrl Pts',(0.52899712724191,-1.,-2.02618329083289));
#31701=CARTESIAN_POINT('Ctrl Pts',(0.52899712724191,1.,-2.02618329083289));
#31702=CARTESIAN_POINT('Ctrl Pts',(0.524925318333518,-1.,-2.02143356304712));
#31703=CARTESIAN_POINT('Ctrl Pts',(0.524925318333518,1.,-2.02143356304712));
#31704=CARTESIAN_POINT('Ctrl Pts',(0.520893590399428,-1.,-2.01666477917306));
#31705=CARTESIAN_POINT('Ctrl Pts',(0.520893590399428,1.,-2.01666477917306));
#31706=CARTESIAN_POINT('Ctrl Pts',(0.516902681728733,-1.,-2.01187773939257));
#31707=CARTESIAN_POINT('Ctrl Pts',(0.516902681728733,1.,-2.01187773939257));
#31708=CARTESIAN_POINT('Ctrl Pts',(0.512953306961813,-1.,-2.00707309946955));
#31709=CARTESIAN_POINT('Ctrl Pts',(0.512953306961813,1.,-2.00707309946955));
#31710=CARTESIAN_POINT('Ctrl Pts',(0.509046069886152,-1.,-2.00225107134733));
#31711=CARTESIAN_POINT('Ctrl Pts',(0.509046069886152,1.,-2.00225107134733));
#31712=CARTESIAN_POINT('Ctrl Pts',(0.505181361323011,-1.,-1.99741107463567));
#31713=CARTESIAN_POINT('Ctrl Pts',(0.505181361323011,1.,-1.99741107463567));
#31714=CARTESIAN_POINT('Ctrl Pts',(0.501359287727129,-1.,-1.9925514912615));
#31715=CARTESIAN_POINT('Ctrl Pts',(0.501359287727129,1.,-1.9925514912615));
#31716=CARTESIAN_POINT('Ctrl Pts',(0.497579909545564,-1.,-1.98767044752929));
#31717=CARTESIAN_POINT('Ctrl Pts',(0.497579909545564,1.,-1.98767044752929));
#31718=CARTESIAN_POINT('Ctrl Pts',(0.493843476541492,-1.,-1.9827665876182));
#31719=CARTESIAN_POINT('Ctrl Pts',(0.493843476541492,1.,-1.9827665876182));
#31720=CARTESIAN_POINT('Ctrl Pts',(0.490150627860955,-1.,-1.97783973019229));
#31721=CARTESIAN_POINT('Ctrl Pts',(0.490150627860955,1.,-1.97783973019229));
#31722=CARTESIAN_POINT('Ctrl Pts',(0.486502692907661,-1.,-1.97289186263272));
#31723=CARTESIAN_POINT('Ctrl Pts',(0.486502692907661,1.,-1.97289186263272));
#31724=CARTESIAN_POINT('Ctrl Pts',(0.482901662120686,-1.,-1.96792703422358));
#31725=CARTESIAN_POINT('Ctrl Pts',(0.482901662120686,1.,-1.96792703422358));
#31726=CARTESIAN_POINT('Ctrl Pts',(0.479349583074846,-1.,-1.96294933055938));
#31727=CARTESIAN_POINT('Ctrl Pts',(0.479349583074846,1.,-1.96294933055938));
#31728=CARTESIAN_POINT('Ctrl Pts',(0.475848034683171,-1.,-1.95796111148175));
#31729=CARTESIAN_POINT('Ctrl Pts',(0.475848034683171,1.,-1.95796111148175));
#31730=CARTESIAN_POINT('Ctrl Pts',(0.472397672264079,-1.,-1.95296148278136));
#31731=CARTESIAN_POINT('Ctrl Pts',(0.472397672264079,1.,-1.95296148278136));
#31732=CARTESIAN_POINT('Ctrl Pts',(0.468997482913158,-1.,-1.94794381136524));
#31733=CARTESIAN_POINT('Ctrl Pts',(0.468997482913158,1.,-1.94794381136524));
#31734=CARTESIAN_POINT('Ctrl Pts',(0.465645462026064,-1.,-1.94289794196205));
#31735=CARTESIAN_POINT('Ctrl Pts',(0.465645462026064,1.,-1.94289794196205));
#31736=CARTESIAN_POINT('Ctrl Pts',(0.462340031009087,-1.,-1.93781486640834));
#31737=CARTESIAN_POINT('Ctrl Pts',(0.462340031009087,1.,-1.93781486640834));
#31738=CARTESIAN_POINT('Ctrl Pts',(0.459081234547931,-1.,-1.93269066517936));
#31739=CARTESIAN_POINT('Ctrl Pts',(0.459081234547931,1.,-1.93269066517936));
#31740=CARTESIAN_POINT('Ctrl Pts',(0.455872005174335,-1.,-1.92753067150461));
#31741=CARTESIAN_POINT('Ctrl Pts',(0.455872005174335,1.,-1.92753067150461));
#31742=CARTESIAN_POINT('Ctrl Pts',(0.452719478359356,-1.,-1.9223538064847));
#31743=CARTESIAN_POINT('Ctrl Pts',(0.452719478359356,1.,-1.9223538064847));
#31744=CARTESIAN_POINT('Ctrl Pts',(0.449632260106572,-1.,-1.91718342555717));
#31745=CARTESIAN_POINT('Ctrl Pts',(0.449632260106572,1.,-1.91718342555717));
#31746=CARTESIAN_POINT('Ctrl Pts',(0.446617343485651,-1.,-1.91203699981095));
#31747=CARTESIAN_POINT('Ctrl Pts',(0.446617343485651,1.,-1.91203699981095));
#31748=CARTESIAN_POINT('Ctrl Pts',(0.44367755684917,-1.,-1.90691756144906));
#31749=CARTESIAN_POINT('Ctrl Pts',(0.44367755684917,1.,-1.90691756144906));
#31750=CARTESIAN_POINT('Ctrl Pts',(0.44080783370416,-1.,-1.90180124389137));
#31751=CARTESIAN_POINT('Ctrl Pts',(0.44080783370416,1.,-1.90180124389137));
#31752=CARTESIAN_POINT('Ctrl Pts',(0.437995003948443,-1.,-1.89663648956549));
#31753=CARTESIAN_POINT('Ctrl Pts',(0.437995003948443,1.,-1.89663648956549));
#31754=CARTESIAN_POINT('Ctrl Pts',(0.43522566096358,-1.,-1.89136993975585));
#31755=CARTESIAN_POINT('Ctrl Pts',(0.43522566096358,1.,-1.89136993975585));
#31756=CARTESIAN_POINT('Ctrl Pts',(0.432493038548833,-1.,-1.88596913666828));
#31757=CARTESIAN_POINT('Ctrl Pts',(0.432493038548833,1.,-1.88596913666828));
#31758=CARTESIAN_POINT('Ctrl Pts',(0.429803062482217,-1.,-1.88044229001779));
#31759=CARTESIAN_POINT('Ctrl Pts',(0.429803062482217,1.,-1.88044229001779));
#31760=CARTESIAN_POINT('Ctrl Pts',(0.427183828518743,-1.,-1.87486989291334));
#31761=CARTESIAN_POINT('Ctrl Pts',(0.427183828518743,1.,-1.87486989291334));
#31762=CARTESIAN_POINT('Ctrl Pts',(0.424678177290876,-1.,-1.8693780394412));
#31763=CARTESIAN_POINT('Ctrl Pts',(0.424678177290876,1.,-1.8693780394412));
#31764=CARTESIAN_POINT('Ctrl Pts',(0.422327307417884,-1.,-1.86408083333863));
#31765=CARTESIAN_POINT('Ctrl Pts',(0.422327307417884,1.,-1.86408083333863));
#31766=CARTESIAN_POINT('Ctrl Pts',(0.420157287975583,-1.,-1.8590328109667));
#31767=CARTESIAN_POINT('Ctrl Pts',(0.420157287975583,1.,-1.8590328109667));
#31768=CARTESIAN_POINT('Ctrl Pts',(0.418164129144045,-1.,-1.8541763285645));
#31769=CARTESIAN_POINT('Ctrl Pts',(0.418164129144045,1.,-1.8541763285645));
#31770=CARTESIAN_POINT('Ctrl Pts',(0.416300022039885,-1.,-1.84929312930314));
#31771=CARTESIAN_POINT('Ctrl Pts',(0.416300022039885,1.,-1.84929312930314));
#31772=CARTESIAN_POINT('Ctrl Pts',(0.414487438255542,-1.,-1.84405757074218));
#31773=CARTESIAN_POINT('Ctrl Pts',(0.414487438255542,1.,-1.84405757074218));
#31774=CARTESIAN_POINT('Ctrl Pts',(0.412633125322945,-1.,-1.8380895347617));
#31775=CARTESIAN_POINT('Ctrl Pts',(0.412633125322945,1.,-1.8380895347617));
#31776=CARTESIAN_POINT('Ctrl Pts',(0.410641256301276,-1.,-1.83100408895047));
#31777=CARTESIAN_POINT('Ctrl Pts',(0.410641256301276,1.,-1.83100408895047));
#31778=CARTESIAN_POINT('Ctrl Pts',(0.408428948106227,-1.,-1.82247022677562));
#31779=CARTESIAN_POINT('Ctrl Pts',(0.408428948106227,1.,-1.82247022677562));
#31780=CARTESIAN_POINT('Ctrl Pts',(0.405933518407175,-1.,-1.81223801812013));
#31781=CARTESIAN_POINT('Ctrl Pts',(0.405933518407175,1.,-1.81223801812013));
#31782=CARTESIAN_POINT('Ctrl Pts',(0.403107976163396,-1.,-1.80012077173238));
#31783=CARTESIAN_POINT('Ctrl Pts',(0.403107976163396,1.,-1.80012077173238));
#31784=CARTESIAN_POINT('Ctrl Pts',(0.399919403774155,-1.,-1.78598826343754));
#31785=CARTESIAN_POINT('Ctrl Pts',(0.399919403774155,1.,-1.78598826343754));
#31786=CARTESIAN_POINT('Ctrl Pts',(0.396346196110688,-1.,-1.76975560043442));
#31787=CARTESIAN_POINT('Ctrl Pts',(0.396346196110688,1.,-1.76975560043442));
#31788=CARTESIAN_POINT('Ctrl Pts',(0.392375812285395,-1.,-1.75137405310193));
#31789=CARTESIAN_POINT('Ctrl Pts',(0.392375812285395,1.,-1.75137405310193));
#31790=CARTESIAN_POINT('Ctrl Pts',(0.388877023502615,-1.,-1.73493170972829));
#31791=CARTESIAN_POINT('Ctrl Pts',(0.388877023502615,1.,-1.73493170972829));
#31792=CARTESIAN_POINT('Ctrl Pts',(0.386070790323281,-1.,-1.72162022244582));
#31793=CARTESIAN_POINT('Ctrl Pts',(0.386070790323281,1.,-1.72162022244582));
#31794=CARTESIAN_POINT('Ctrl Pts',(0.384119047314215,-1.,-1.71231062891398));
#31795=CARTESIAN_POINT('Ctrl Pts',(0.384119047314215,1.,-1.71231062891398));
#31796=CARTESIAN_POINT('Ctrl Pts',(0.383122945602004,-1.,-1.7075470150345));
#31797=CARTESIAN_POINT('Ctrl Pts',(0.383122945602004,1.,-1.7075470150345));
#31798=CARTESIAN_POINT('',(0.61342227326009,1.,-2.11275013067528));
#31799=CARTESIAN_POINT('Ctrl Pts',(0.61342227326009,1.,-2.11275013067528));
#31800=CARTESIAN_POINT('Ctrl Pts',(0.61246736556225,1.,-2.11187554260142));
#31801=CARTESIAN_POINT('Ctrl Pts',(0.610560911691113,1.,-2.11012443807661));
#31802=CARTESIAN_POINT('Ctrl Pts',(0.607711315456826,1.,-2.10749199615859));
#31803=CARTESIAN_POINT('Ctrl Pts',(0.603932030738212,1.,-2.10397049887709));
#31804=CARTESIAN_POINT('Ctrl Pts',(0.599241616422144,1.,-2.09954930865331));
#31805=CARTESIAN_POINT('Ctrl Pts',(0.594585006052823,1.,-2.09510876220501));
#31806=CARTESIAN_POINT('Ctrl Pts',(0.589962365403189,1.,-2.09064881812053));
#31807=CARTESIAN_POINT('Ctrl Pts',(0.585373918990895,1.,-2.086169437277));
#31808=CARTESIAN_POINT('Ctrl Pts',(0.580819952107256,1.,-2.08167059018138));
#31809=CARTESIAN_POINT('Ctrl Pts',(0.576300797416274,1.,-2.07715226767361));
#31810=CARTESIAN_POINT('Ctrl Pts',(0.571816823242411,1.,-2.07261449292758));
#31811=CARTESIAN_POINT('Ctrl Pts',(0.567368421181229,1.,-2.06805732997383));
#31812=CARTESIAN_POINT('Ctrl Pts',(0.562955993082574,1.,-2.06348090160697));
#31813=CARTESIAN_POINT('Ctrl Pts',(0.558579940185467,1.,-2.05888537756571));
#31814=CARTESIAN_POINT('Ctrl Pts',(0.554240657464109,1.,-2.05427091604482));
#31815=CARTESIAN_POINT('Ctrl Pts',(0.549938525150342,1.,-2.04963761077974));
#31816=CARTESIAN_POINT('Ctrl Pts',(0.545673903817348,1.,-2.0449854471456));
#31817=CARTESIAN_POINT('Ctrl Pts',(0.54144712061552,1.,-2.0403142269048));
#31818=CARTESIAN_POINT('Ctrl Pts',(0.537258489833134,1.,-2.03562362953993));
#31819=CARTESIAN_POINT('Ctrl Pts',(0.533108355132905,1.,-2.03091336214401));
#31820=CARTESIAN_POINT('Ctrl Pts',(0.52899712724191,1.,-2.02618329083289));
#31821=CARTESIAN_POINT('Ctrl Pts',(0.524925318333518,1.,-2.02143356304712));
#31822=CARTESIAN_POINT('Ctrl Pts',(0.520893590399428,1.,-2.01666477917306));
#31823=CARTESIAN_POINT('Ctrl Pts',(0.516902681728733,1.,-2.01187773939257));
#31824=CARTESIAN_POINT('Ctrl Pts',(0.512953306961813,1.,-2.00707309946955));
#31825=CARTESIAN_POINT('Ctrl Pts',(0.509046069886152,1.,-2.00225107134733));
#31826=CARTESIAN_POINT('Ctrl Pts',(0.505181361323011,1.,-1.99741107463567));
#31827=CARTESIAN_POINT('Ctrl Pts',(0.501359287727129,1.,-1.9925514912615));
#31828=CARTESIAN_POINT('Ctrl Pts',(0.497579909545564,1.,-1.98767044752929));
#31829=CARTESIAN_POINT('Ctrl Pts',(0.493843476541492,1.,-1.9827665876182));
#31830=CARTESIAN_POINT('Ctrl Pts',(0.490150627860955,1.,-1.97783973019229));
#31831=CARTESIAN_POINT('Ctrl Pts',(0.486502692907661,1.,-1.97289186263272));
#31832=CARTESIAN_POINT('Ctrl Pts',(0.482901662120686,1.,-1.96792703422358));
#31833=CARTESIAN_POINT('Ctrl Pts',(0.479349583074846,1.,-1.96294933055938));
#31834=CARTESIAN_POINT('Ctrl Pts',(0.475848034683171,1.,-1.95796111148175));
#31835=CARTESIAN_POINT('Ctrl Pts',(0.472397672264079,1.,-1.95296148278136));
#31836=CARTESIAN_POINT('Ctrl Pts',(0.468997482913158,1.,-1.94794381136524));
#31837=CARTESIAN_POINT('Ctrl Pts',(0.465645462026064,1.,-1.94289794196205));
#31838=CARTESIAN_POINT('Ctrl Pts',(0.462340031009087,1.,-1.93781486640834));
#31839=CARTESIAN_POINT('Ctrl Pts',(0.459081234547931,1.,-1.93269066517936));
#31840=CARTESIAN_POINT('Ctrl Pts',(0.455872005174335,1.,-1.92753067150461));
#31841=CARTESIAN_POINT('Ctrl Pts',(0.452719478359356,1.,-1.9223538064847));
#31842=CARTESIAN_POINT('Ctrl Pts',(0.449632260106572,1.,-1.91718342555717));
#31843=CARTESIAN_POINT('Ctrl Pts',(0.446617343485651,1.,-1.91203699981095));
#31844=CARTESIAN_POINT('Ctrl Pts',(0.44367755684917,1.,-1.90691756144906));
#31845=CARTESIAN_POINT('Ctrl Pts',(0.44080783370416,1.,-1.90180124389137));
#31846=CARTESIAN_POINT('Ctrl Pts',(0.437995003948443,1.,-1.89663648956549));
#31847=CARTESIAN_POINT('Ctrl Pts',(0.43522566096358,1.,-1.89136993975585));
#31848=CARTESIAN_POINT('Ctrl Pts',(0.432493038548833,1.,-1.88596913666828));
#31849=CARTESIAN_POINT('Ctrl Pts',(0.429803062482217,1.,-1.88044229001779));
#31850=CARTESIAN_POINT('Ctrl Pts',(0.427183828518743,1.,-1.87486989291334));
#31851=CARTESIAN_POINT('Ctrl Pts',(0.424678177290876,1.,-1.8693780394412));
#31852=CARTESIAN_POINT('Ctrl Pts',(0.422327307417884,1.,-1.86408083333863));
#31853=CARTESIAN_POINT('Ctrl Pts',(0.420157287975583,1.,-1.8590328109667));
#31854=CARTESIAN_POINT('Ctrl Pts',(0.418164129144045,1.,-1.8541763285645));
#31855=CARTESIAN_POINT('Ctrl Pts',(0.416300022039885,1.,-1.84929312930314));
#31856=CARTESIAN_POINT('Ctrl Pts',(0.414487438255542,1.,-1.84405757074218));
#31857=CARTESIAN_POINT('Ctrl Pts',(0.412633125322945,1.,-1.8380895347617));
#31858=CARTESIAN_POINT('Ctrl Pts',(0.410641256301276,1.,-1.83100408895047));
#31859=CARTESIAN_POINT('Ctrl Pts',(0.408428948106227,1.,-1.82247022677562));
#31860=CARTESIAN_POINT('Ctrl Pts',(0.405933518407175,1.,-1.81223801812013));
#31861=CARTESIAN_POINT('Ctrl Pts',(0.403107976163396,1.,-1.80012077173238));
#31862=CARTESIAN_POINT('Ctrl Pts',(0.399919403774155,1.,-1.78598826343754));
#31863=CARTESIAN_POINT('Ctrl Pts',(0.396346196110688,1.,-1.76975560043442));
#31864=CARTESIAN_POINT('Ctrl Pts',(0.392375812285395,1.,-1.75137405310193));
#31865=CARTESIAN_POINT('Ctrl Pts',(0.388877023502615,1.,-1.73493170972829));
#31866=CARTESIAN_POINT('Ctrl Pts',(0.386070790323281,1.,-1.72162022244582));
#31867=CARTESIAN_POINT('Ctrl Pts',(0.384119047314215,1.,-1.71231062891398));
#31868=CARTESIAN_POINT('Ctrl Pts',(0.383122945602004,1.,-1.7075470150345));
#31869=CARTESIAN_POINT('',(0.61342227326009,0.,-2.11275013067528));
#31870=CARTESIAN_POINT('Origin',(0.745574324794401,0.,-2.0698113262342));
#31871=CARTESIAN_POINT('',(0.745574324794401,1.,-2.0698113262342));
#31872=CARTESIAN_POINT('',(0.61342227326009,1.,-2.11275013067528));
#31873=CARTESIAN_POINT('',(0.745574324794401,0.,-2.0698113262342));
#31874=CARTESIAN_POINT('Ctrl Pts',(0.693717979106306,-1.,-1.60662857109684));
#31875=CARTESIAN_POINT('Ctrl Pts',(0.693717979106306,1.,-1.60662857109684));
#31876=CARTESIAN_POINT('Ctrl Pts',(0.695712097881194,-1.,-1.61106790958151));
#31877=CARTESIAN_POINT('Ctrl Pts',(0.695712097881194,1.,-1.61106790958151));
#31878=CARTESIAN_POINT('Ctrl Pts',(0.699605146405088,-1.,-1.61974673472612));
#31879=CARTESIAN_POINT('Ctrl Pts',(0.699605146405088,1.,-1.61974673472612));
#31880=CARTESIAN_POINT('Ctrl Pts',(0.705159151988319,-1.,-1.63216541664676));
#31881=CARTESIAN_POINT('Ctrl Pts',(0.705159151988319,1.,-1.63216541664676));
#31882=CARTESIAN_POINT('Ctrl Pts',(0.711993139355394,-1.,-1.64752408832016));
#31883=CARTESIAN_POINT('Ctrl Pts',(0.711993139355394,1.,-1.64752408832016));
#31884=CARTESIAN_POINT('Ctrl Pts',(0.719585433804282,-1.,-1.6647288055568));
#31885=CARTESIAN_POINT('Ctrl Pts',(0.719585433804282,1.,-1.6647288055568));
#31886=CARTESIAN_POINT('Ctrl Pts',(0.726235967997433,-1.,-1.67996158455503));
#31887=CARTESIAN_POINT('Ctrl Pts',(0.726235967997433,1.,-1.67996158455503));
#31888=CARTESIAN_POINT('Ctrl Pts',(0.731963238697195,-1.,-1.69326921975743));
#31889=CARTESIAN_POINT('Ctrl Pts',(0.731963238697195,1.,-1.69326921975743));
#31890=CARTESIAN_POINT('Ctrl Pts',(0.736799665724771,-1.,-1.70473309006121));
#31891=CARTESIAN_POINT('Ctrl Pts',(0.736799665724771,1.,-1.70473309006121));
#31892=CARTESIAN_POINT('Ctrl Pts',(0.740795162032087,-1.,-1.71447789751927));
#31893=CARTESIAN_POINT('Ctrl Pts',(0.740795162032087,1.,-1.71447789751927));
#31894=CARTESIAN_POINT('Ctrl Pts',(0.744021445433764,-1.,-1.7226822991693));
#31895=CARTESIAN_POINT('Ctrl Pts',(0.744021445433764,1.,-1.7226822991693));
#31896=CARTESIAN_POINT('Ctrl Pts',(0.746574710096436,-1.,-1.72958533647399));
#31897=CARTESIAN_POINT('Ctrl Pts',(0.746574710096436,1.,-1.72958533647399));
#31898=CARTESIAN_POINT('Ctrl Pts',(0.748582462954854,-1.,-1.73550351679848));
#31899=CARTESIAN_POINT('Ctrl Pts',(0.748582462954854,1.,-1.73550351679848));
#31900=CARTESIAN_POINT('Ctrl Pts',(0.75019343597954,-1.,-1.74080458266705));
#31901=CARTESIAN_POINT('Ctrl Pts',(0.75019343597954,1.,-1.74080458266705));
#31902=CARTESIAN_POINT('Ctrl Pts',(0.751555614163629,-1.,-1.74585086852298));
#31903=CARTESIAN_POINT('Ctrl Pts',(0.751555614163629,1.,-1.74585086852298));
#31904=CARTESIAN_POINT('Ctrl Pts',(0.752797683531377,-1.,-1.75095139468809));
#31905=CARTESIAN_POINT('Ctrl Pts',(0.752797683531377,1.,-1.75095139468809));
#31906=CARTESIAN_POINT('Ctrl Pts',(0.75400925402848,-1.,-1.75631083600175));
#31907=CARTESIAN_POINT('Ctrl Pts',(0.75400925402848,1.,-1.75631083600175));
#31908=CARTESIAN_POINT('Ctrl Pts',(0.755220979975262,-1.,-1.7619781724032));
#31909=CARTESIAN_POINT('Ctrl Pts',(0.755220979975262,1.,-1.7619781724032));
#31910=CARTESIAN_POINT('Ctrl Pts',(0.756421896028403,-1.,-1.76789396003141));
#31911=CARTESIAN_POINT('Ctrl Pts',(0.756421896028403,1.,-1.76789396003141));
#31912=CARTESIAN_POINT('Ctrl Pts',(0.757578264077238,-1.,-1.77394167108342));
#31913=CARTESIAN_POINT('Ctrl Pts',(0.757578264077238,1.,-1.77394167108342));
#31914=CARTESIAN_POINT('Ctrl Pts',(0.75865062667738,-1.,-1.77999411220912));
#31915=CARTESIAN_POINT('Ctrl Pts',(0.75865062667738,1.,-1.77999411220912));
#31916=CARTESIAN_POINT('Ctrl Pts',(0.759614401109868,-1.,-1.78596964884527));
#31917=CARTESIAN_POINT('Ctrl Pts',(0.759614401109868,1.,-1.78596964884527));
#31918=CARTESIAN_POINT('Ctrl Pts',(0.760469555880425,-1.,-1.79185815610802));
#31919=CARTESIAN_POINT('Ctrl Pts',(0.760469555880425,1.,-1.79185815610802));
#31920=CARTESIAN_POINT('Ctrl Pts',(0.761229695230359,-1.,-1.79768986997735));
#31921=CARTESIAN_POINT('Ctrl Pts',(0.761229695230359,1.,-1.79768986997735));
#31922=CARTESIAN_POINT('Ctrl Pts',(0.761915336443515,-1.,-1.80351583877334));
#31923=CARTESIAN_POINT('Ctrl Pts',(0.761915336443515,1.,-1.80351583877334));
#31924=CARTESIAN_POINT('Ctrl Pts',(0.762546129464036,-1.,-1.80938551463989));
#31925=CARTESIAN_POINT('Ctrl Pts',(0.762546129464036,1.,-1.80938551463989));
#31926=CARTESIAN_POINT('Ctrl Pts',(0.763132003836783,-1.,-1.81532118405566));
#31927=CARTESIAN_POINT('Ctrl Pts',(0.763132003836783,1.,-1.81532118405566));
#31928=CARTESIAN_POINT('Ctrl Pts',(0.763673465462854,-1.,-1.82131873145297));
#31929=CARTESIAN_POINT('Ctrl Pts',(0.763673465462854,1.,-1.82131873145297));
#31930=CARTESIAN_POINT('Ctrl Pts',(0.764165902606055,-1.,-1.8273599120008));
#31931=CARTESIAN_POINT('Ctrl Pts',(0.764165902606055,1.,-1.8273599120008));
#31932=CARTESIAN_POINT('Ctrl Pts',(0.764602549687845,-1.,-1.8334207722714));
#31933=CARTESIAN_POINT('Ctrl Pts',(0.764602549687845,1.,-1.8334207722714));
#31934=CARTESIAN_POINT('Ctrl Pts',(0.764978057881687,-1.,-1.83948181064823));
#31935=CARTESIAN_POINT('Ctrl Pts',(0.764978057881687,1.,-1.83948181064823));
#31936=CARTESIAN_POINT('Ctrl Pts',(0.765291664861971,-1.,-1.84553698875911));
#31937=CARTESIAN_POINT('Ctrl Pts',(0.765291664861971,1.,-1.84553698875911));
#31938=CARTESIAN_POINT('Ctrl Pts',(0.765545710619023,-1.,-1.85158945130054));
#31939=CARTESIAN_POINT('Ctrl Pts',(0.765545710619023,1.,-1.85158945130054));
#31940=CARTESIAN_POINT('Ctrl Pts',(0.765744212909305,-1.,-1.85764741390391));
#31941=CARTESIAN_POINT('Ctrl Pts',(0.765744212909305,1.,-1.85764741390391));
#31942=CARTESIAN_POINT('Ctrl Pts',(0.765891519092557,-1.,-1.86372027063315));
#31943=CARTESIAN_POINT('Ctrl Pts',(0.765891519092557,1.,-1.86372027063315));
#31944=CARTESIAN_POINT('Ctrl Pts',(0.765990708546111,-1.,-1.86981398314345));
#31945=CARTESIAN_POINT('Ctrl Pts',(0.765990708546111,1.,-1.86981398314345));
#31946=CARTESIAN_POINT('Ctrl Pts',(0.766042837036759,-1.,-1.87592888967886));
#31947=CARTESIAN_POINT('Ctrl Pts',(0.766042837036759,1.,-1.87592888967886));
#31948=CARTESIAN_POINT('Ctrl Pts',(0.766047794851868,-1.,-1.88206215302561));
#31949=CARTESIAN_POINT('Ctrl Pts',(0.766047794851868,1.,-1.88206215302561));
#31950=CARTESIAN_POINT('Ctrl Pts',(0.76600483706209,-1.,-1.88820926433409));
#31951=CARTESIAN_POINT('Ctrl Pts',(0.76600483706209,1.,-1.88820926433409));
#31952=CARTESIAN_POINT('Ctrl Pts',(0.765913193856979,-1.,-1.89436577771389));
#31953=CARTESIAN_POINT('Ctrl Pts',(0.765913193856979,1.,-1.89436577771389));
#31954=CARTESIAN_POINT('Ctrl Pts',(0.765772772593395,-1.,-1.90052930393599));
#31955=CARTESIAN_POINT('Ctrl Pts',(0.765772772593395,1.,-1.90052930393599));
#31956=CARTESIAN_POINT('Ctrl Pts',(0.765584196937936,-1.,-1.90669961402362));
#31957=CARTESIAN_POINT('Ctrl Pts',(0.765584196937936,1.,-1.90669961402362));
#31958=CARTESIAN_POINT('Ctrl Pts',(0.765348465884739,-1.,-1.91287765805174));
#31959=CARTESIAN_POINT('Ctrl Pts',(0.765348465884739,1.,-1.91287765805174));
#31960=CARTESIAN_POINT('Ctrl Pts',(0.765066729667095,-1.,-1.91906491634197));
#31961=CARTESIAN_POINT('Ctrl Pts',(0.765066729667095,1.,-1.91906491634197));
#31962=CARTESIAN_POINT('Ctrl Pts',(0.764740025488189,-1.,-1.92526263537041));
#31963=CARTESIAN_POINT('Ctrl Pts',(0.764740025488189,1.,-1.92526263537041));
#31964=CARTESIAN_POINT('Ctrl Pts',(0.764369010673889,-1.,-1.93147105496367));
#31965=CARTESIAN_POINT('Ctrl Pts',(0.764369010673889,1.,-1.93147105496367));
#31966=CARTESIAN_POINT('Ctrl Pts',(0.763954049121393,-1.,-1.93768964875867));
#31967=CARTESIAN_POINT('Ctrl Pts',(0.763954049121393,1.,-1.93768964875867));
#31968=CARTESIAN_POINT('Ctrl Pts',(0.76349533353858,-1.,-1.94391746617626));
#31969=CARTESIAN_POINT('Ctrl Pts',(0.76349533353858,1.,-1.94391746617626));
#31970=CARTESIAN_POINT('Ctrl Pts',(0.762992990878774,-1.,-1.95015342590025));
#31971=CARTESIAN_POINT('Ctrl Pts',(0.762992990878774,1.,-1.95015342590025));
#31972=CARTESIAN_POINT('Ctrl Pts',(0.762447203806263,-1.,-1.95639665309893));
#31973=CARTESIAN_POINT('Ctrl Pts',(0.762447203806263,1.,-1.95639665309893));
#31974=CARTESIAN_POINT('Ctrl Pts',(0.761858300014575,-1.,-1.96264672744229));
#31975=CARTESIAN_POINT('Ctrl Pts',(0.761858300014575,1.,-1.96264672744229));
#31976=CARTESIAN_POINT('Ctrl Pts',(0.761226690483986,-1.,-1.96890351582545));
#31977=CARTESIAN_POINT('Ctrl Pts',(0.761226690483986,1.,-1.96890351582545));
#31978=CARTESIAN_POINT('Ctrl Pts',(0.760552825409855,-1.,-1.97516705321521));
#31979=CARTESIAN_POINT('Ctrl Pts',(0.760552825409855,1.,-1.97516705321521));
#31980=CARTESIAN_POINT('Ctrl Pts',(0.759837147452135,-1.,-1.98143741418156));
#31981=CARTESIAN_POINT('Ctrl Pts',(0.759837147452135,1.,-1.98143741418156));
#31982=CARTESIAN_POINT('Ctrl Pts',(0.759080037802242,-1.,-1.98771456680806));
#31983=CARTESIAN_POINT('Ctrl Pts',(0.759080037802242,1.,-1.98771456680806));
#31984=CARTESIAN_POINT('Ctrl Pts',(0.758281796766377,-1.,-1.9939983109871));
#31985=CARTESIAN_POINT('Ctrl Pts',(0.758281796766377,1.,-1.9939983109871));
#31986=CARTESIAN_POINT('Ctrl Pts',(0.757442676862341,-1.,-2.00028834739072));
#31987=CARTESIAN_POINT('Ctrl Pts',(0.757442676862341,1.,-2.00028834739072));
#31988=CARTESIAN_POINT('Ctrl Pts',(0.756562904646496,-1.,-2.00658431587682));
#31989=CARTESIAN_POINT('Ctrl Pts',(0.756562904646496,1.,-2.00658431587682));
#31990=CARTESIAN_POINT('Ctrl Pts',(0.7556427049581,-1.,-2.01288584328149));
#31991=CARTESIAN_POINT('Ctrl Pts',(0.7556427049581,1.,-2.01288584328149));
#31992=CARTESIAN_POINT('Ctrl Pts',(0.75468233072352,-1.,-2.01919259406003));
#31993=CARTESIAN_POINT('Ctrl Pts',(0.75468233072352,1.,-2.01919259406003));
#31994=CARTESIAN_POINT('Ctrl Pts',(0.753682061113765,-1.,-2.02550428623587));
#31995=CARTESIAN_POINT('Ctrl Pts',(0.753682061113765,1.,-2.02550428623587));
#31996=CARTESIAN_POINT('Ctrl Pts',(0.752642180488104,-1.,-2.03182068456467));
#31997=CARTESIAN_POINT('Ctrl Pts',(0.752642180488104,1.,-2.03182068456467));
#31998=CARTESIAN_POINT('Ctrl Pts',(0.751562963361383,-1.,-2.03814160092173));
#31999=CARTESIAN_POINT('Ctrl Pts',(0.751562963361383,1.,-2.03814160092173));
#32000=CARTESIAN_POINT('Ctrl Pts',(0.750444657874758,-1.,-2.04446689147754));
#32001=CARTESIAN_POINT('Ctrl Pts',(0.750444657874758,1.,-2.04446689147754));
#32002=CARTESIAN_POINT('Ctrl Pts',(0.749287468663053,-1.,-2.05079645591606));
#32003=CARTESIAN_POINT('Ctrl Pts',(0.749287468663053,1.,-2.05079645591606));
#32004=CARTESIAN_POINT('Ctrl Pts',(0.748091554181101,-1.,-2.05713023030263));
#32005=CARTESIAN_POINT('Ctrl Pts',(0.748091554181101,1.,-2.05713023030263));
#32006=CARTESIAN_POINT('Ctrl Pts',(0.747103932785504,-1.,-2.06220058927162));
#32007=CARTESIAN_POINT('Ctrl Pts',(0.747103932785504,1.,-2.06220058927162));
#32008=CARTESIAN_POINT('Ctrl Pts',(0.746345871542695,-1.,-2.06600523016401));
#32009=CARTESIAN_POINT('Ctrl Pts',(0.746345871542695,1.,-2.06600523016401));
#32010=CARTESIAN_POINT('Ctrl Pts',(0.74583279137781,-1.,-2.06854248895575));
#32011=CARTESIAN_POINT('Ctrl Pts',(0.74583279137781,1.,-2.06854248895575));
#32012=CARTESIAN_POINT('Ctrl Pts',(0.745574324794401,-1.,-2.0698113262342));
#32013=CARTESIAN_POINT('Ctrl Pts',(0.745574324794401,1.,-2.0698113262342));
#32014=CARTESIAN_POINT('',(0.693717979106306,1.,-1.60662857109684));
#32015=CARTESIAN_POINT('Ctrl Pts',(0.693717979106306,1.,-1.60662857109684));
#32016=CARTESIAN_POINT('Ctrl Pts',(0.695712097881194,1.,-1.61106790958151));
#32017=CARTESIAN_POINT('Ctrl Pts',(0.699605146405088,1.,-1.61974673472612));
#32018=CARTESIAN_POINT('Ctrl Pts',(0.705159151988319,1.,-1.63216541664676));
#32019=CARTESIAN_POINT('Ctrl Pts',(0.711993139355394,1.,-1.64752408832016));
#32020=CARTESIAN_POINT('Ctrl Pts',(0.719585433804282,1.,-1.6647288055568));
#32021=CARTESIAN_POINT('Ctrl Pts',(0.726235967997433,1.,-1.67996158455503));
#32022=CARTESIAN_POINT('Ctrl Pts',(0.731963238697195,1.,-1.69326921975743));
#32023=CARTESIAN_POINT('Ctrl Pts',(0.736799665724771,1.,-1.70473309006121));
#32024=CARTESIAN_POINT('Ctrl Pts',(0.740795162032087,1.,-1.71447789751927));
#32025=CARTESIAN_POINT('Ctrl Pts',(0.744021445433764,1.,-1.7226822991693));
#32026=CARTESIAN_POINT('Ctrl Pts',(0.746574710096436,1.,-1.72958533647399));
#32027=CARTESIAN_POINT('Ctrl Pts',(0.748582462954854,1.,-1.73550351679848));
#32028=CARTESIAN_POINT('Ctrl Pts',(0.75019343597954,1.,-1.74080458266705));
#32029=CARTESIAN_POINT('Ctrl Pts',(0.751555614163629,1.,-1.74585086852298));
#32030=CARTESIAN_POINT('Ctrl Pts',(0.752797683531377,1.,-1.75095139468809));
#32031=CARTESIAN_POINT('Ctrl Pts',(0.75400925402848,1.,-1.75631083600175));
#32032=CARTESIAN_POINT('Ctrl Pts',(0.755220979975262,1.,-1.7619781724032));
#32033=CARTESIAN_POINT('Ctrl Pts',(0.756421896028403,1.,-1.76789396003141));
#32034=CARTESIAN_POINT('Ctrl Pts',(0.757578264077238,1.,-1.77394167108342));
#32035=CARTESIAN_POINT('Ctrl Pts',(0.75865062667738,1.,-1.77999411220912));
#32036=CARTESIAN_POINT('Ctrl Pts',(0.759614401109868,1.,-1.78596964884527));
#32037=CARTESIAN_POINT('Ctrl Pts',(0.760469555880425,1.,-1.79185815610802));
#32038=CARTESIAN_POINT('Ctrl Pts',(0.761229695230359,1.,-1.79768986997735));
#32039=CARTESIAN_POINT('Ctrl Pts',(0.761915336443515,1.,-1.80351583877334));
#32040=CARTESIAN_POINT('Ctrl Pts',(0.762546129464036,1.,-1.80938551463989));
#32041=CARTESIAN_POINT('Ctrl Pts',(0.763132003836783,1.,-1.81532118405566));
#32042=CARTESIAN_POINT('Ctrl Pts',(0.763673465462854,1.,-1.82131873145297));
#32043=CARTESIAN_POINT('Ctrl Pts',(0.764165902606055,1.,-1.8273599120008));
#32044=CARTESIAN_POINT('Ctrl Pts',(0.764602549687845,1.,-1.8334207722714));
#32045=CARTESIAN_POINT('Ctrl Pts',(0.764978057881687,1.,-1.83948181064823));
#32046=CARTESIAN_POINT('Ctrl Pts',(0.765291664861971,1.,-1.84553698875911));
#32047=CARTESIAN_POINT('Ctrl Pts',(0.765545710619023,1.,-1.85158945130054));
#32048=CARTESIAN_POINT('Ctrl Pts',(0.765744212909305,1.,-1.85764741390391));
#32049=CARTESIAN_POINT('Ctrl Pts',(0.765891519092557,1.,-1.86372027063315));
#32050=CARTESIAN_POINT('Ctrl Pts',(0.765990708546111,1.,-1.86981398314345));
#32051=CARTESIAN_POINT('Ctrl Pts',(0.766042837036759,1.,-1.87592888967886));
#32052=CARTESIAN_POINT('Ctrl Pts',(0.766047794851868,1.,-1.88206215302561));
#32053=CARTESIAN_POINT('Ctrl Pts',(0.76600483706209,1.,-1.88820926433409));
#32054=CARTESIAN_POINT('Ctrl Pts',(0.765913193856979,1.,-1.89436577771389));
#32055=CARTESIAN_POINT('Ctrl Pts',(0.765772772593395,1.,-1.90052930393599));
#32056=CARTESIAN_POINT('Ctrl Pts',(0.765584196937936,1.,-1.90669961402362));
#32057=CARTESIAN_POINT('Ctrl Pts',(0.765348465884739,1.,-1.91287765805174));
#32058=CARTESIAN_POINT('Ctrl Pts',(0.765066729667095,1.,-1.91906491634197));
#32059=CARTESIAN_POINT('Ctrl Pts',(0.764740025488189,1.,-1.92526263537041));
#32060=CARTESIAN_POINT('Ctrl Pts',(0.764369010673889,1.,-1.93147105496367));
#32061=CARTESIAN_POINT('Ctrl Pts',(0.763954049121393,1.,-1.93768964875867));
#32062=CARTESIAN_POINT('Ctrl Pts',(0.76349533353858,1.,-1.94391746617626));
#32063=CARTESIAN_POINT('Ctrl Pts',(0.762992990878774,1.,-1.95015342590025));
#32064=CARTESIAN_POINT('Ctrl Pts',(0.762447203806263,1.,-1.95639665309893));
#32065=CARTESIAN_POINT('Ctrl Pts',(0.761858300014575,1.,-1.96264672744229));
#32066=CARTESIAN_POINT('Ctrl Pts',(0.761226690483986,1.,-1.96890351582545));
#32067=CARTESIAN_POINT('Ctrl Pts',(0.760552825409855,1.,-1.97516705321521));
#32068=CARTESIAN_POINT('Ctrl Pts',(0.759837147452135,1.,-1.98143741418156));
#32069=CARTESIAN_POINT('Ctrl Pts',(0.759080037802242,1.,-1.98771456680806));
#32070=CARTESIAN_POINT('Ctrl Pts',(0.758281796766377,1.,-1.9939983109871));
#32071=CARTESIAN_POINT('Ctrl Pts',(0.757442676862341,1.,-2.00028834739072));
#32072=CARTESIAN_POINT('Ctrl Pts',(0.756562904646496,1.,-2.00658431587682));
#32073=CARTESIAN_POINT('Ctrl Pts',(0.7556427049581,1.,-2.01288584328149));
#32074=CARTESIAN_POINT('Ctrl Pts',(0.75468233072352,1.,-2.01919259406003));
#32075=CARTESIAN_POINT('Ctrl Pts',(0.753682061113765,1.,-2.02550428623587));
#32076=CARTESIAN_POINT('Ctrl Pts',(0.752642180488104,1.,-2.03182068456467));
#32077=CARTESIAN_POINT('Ctrl Pts',(0.751562963361383,1.,-2.03814160092173));
#32078=CARTESIAN_POINT('Ctrl Pts',(0.750444657874758,1.,-2.04446689147754));
#32079=CARTESIAN_POINT('Ctrl Pts',(0.749287468663053,1.,-2.05079645591606));
#32080=CARTESIAN_POINT('Ctrl Pts',(0.748091554181101,1.,-2.05713023030263));
#32081=CARTESIAN_POINT('Ctrl Pts',(0.747103932785504,1.,-2.06220058927162));
#32082=CARTESIAN_POINT('Ctrl Pts',(0.746345871542695,1.,-2.06600523016401));
#32083=CARTESIAN_POINT('Ctrl Pts',(0.74583279137781,1.,-2.06854248895575));
#32084=CARTESIAN_POINT('Ctrl Pts',(0.745574324794401,1.,-2.0698113262342));
#32085=CARTESIAN_POINT('',(0.693717979106306,0.,-1.60662857109684));
#32086=CARTESIAN_POINT('Origin',(0.,0.,0.));
#32087=CARTESIAN_POINT('',(0.892032620296855,1.,-1.5055822144029));
#32088=CARTESIAN_POINT('Origin',(0.,1.,0.));
#32089=CARTESIAN_POINT('',(0.892032620296855,0.,-1.5055822144029));
#32090=CARTESIAN_POINT('Ctrl Pts',(1.23627494547115,-1.,-1.81978687191668));
#32091=CARTESIAN_POINT('Ctrl Pts',(1.23627494547115,1.,-1.81978687191668));
#32092=CARTESIAN_POINT('Ctrl Pts',(1.23509651170476,-1.,-1.81925017193666));
#32093=CARTESIAN_POINT('Ctrl Pts',(1.23509651170476,1.,-1.81925017193666));
#32094=CARTESIAN_POINT('Ctrl Pts',(1.2327422452705,-1.,-1.81817389921279));
#32095=CARTESIAN_POINT('Ctrl Pts',(1.2327422452705,1.,-1.81817389921279));
#32096=CARTESIAN_POINT('Ctrl Pts',(1.2292186489137,-1.,-1.8165508718364));
#32097=CARTESIAN_POINT('Ctrl Pts',(1.2292186489137,1.,-1.8165508718364));
#32098=CARTESIAN_POINT('Ctrl Pts',(1.2245361330495,-1.,-1.81436959210434));
#32099=CARTESIAN_POINT('Ctrl Pts',(1.2245361330495,1.,-1.81436959210434));
#32100=CARTESIAN_POINT('Ctrl Pts',(1.21870906103557,-1.,-1.81161420806656));
#32101=CARTESIAN_POINT('Ctrl Pts',(1.21870906103557,1.,-1.81161420806656));
#32102=CARTESIAN_POINT('Ctrl Pts',(1.21290815708314,-1.,-1.80882996917129));
#32103=CARTESIAN_POINT('Ctrl Pts',(1.21290815708314,1.,-1.80882996917129));
#32104=CARTESIAN_POINT('Ctrl Pts',(1.20713356605475,-1.,-1.80601678480707));
#32105=CARTESIAN_POINT('Ctrl Pts',(1.20713356605475,1.,-1.80601678480707));
#32106=CARTESIAN_POINT('Ctrl Pts',(1.20138548938974,-1.,-1.80317454838603));
#32107=CARTESIAN_POINT('Ctrl Pts',(1.20138548938974,1.,-1.80317454838603));
#32108=CARTESIAN_POINT('Ctrl Pts',(1.19566418930242,-1.,-1.80030314369879));
#32109=CARTESIAN_POINT('Ctrl Pts',(1.19566418930242,1.,-1.80030314369879));
#32110=CARTESIAN_POINT('Ctrl Pts',(1.18996997934445,-1.,-1.79740245923478));
#32111=CARTESIAN_POINT('Ctrl Pts',(1.18996997934445,1.,-1.79740245923478));
#32112=CARTESIAN_POINT('Ctrl Pts',(1.18430321697432,-1.,-1.79447240321515));
#32113=CARTESIAN_POINT('Ctrl Pts',(1.18430321697432,1.,-1.79447240321515));
#32114=CARTESIAN_POINT('Ctrl Pts',(1.17866429440809,-1.,-1.79151291552689));
#32115=CARTESIAN_POINT('Ctrl Pts',(1.17866429440809,1.,-1.79151291552689));
#32116=CARTESIAN_POINT('Ctrl Pts',(1.17305363177328,-1.,-1.78852398877617));
#32117=CARTESIAN_POINT('Ctrl Pts',(1.17305363177328,1.,-1.78852398877617));
#32118=CARTESIAN_POINT('Ctrl Pts',(1.16747166312303,-1.,-1.78550566040443));
#32119=CARTESIAN_POINT('Ctrl Pts',(1.16747166312303,1.,-1.78550566040443));
#32120=CARTESIAN_POINT('Ctrl Pts',(1.16191881298499,-1.,-1.78245795881009));
#32121=CARTESIAN_POINT('Ctrl Pts',(1.16191881298499,1.,-1.78245795881009));
#32122=CARTESIAN_POINT('Ctrl Pts',(1.15639547194698,-1.,-1.77938085564275));
#32123=CARTESIAN_POINT('Ctrl Pts',(1.15639547194698,1.,-1.77938085564275));
#32124=CARTESIAN_POINT('Ctrl Pts',(1.15090197841514,-1.,-1.7762742255701));
#32125=CARTESIAN_POINT('Ctrl Pts',(1.15090197841514,1.,-1.7762742255701));
#32126=CARTESIAN_POINT('Ctrl Pts',(1.1454385822692,-1.,-1.77313777896194));
#32127=CARTESIAN_POINT('Ctrl Pts',(1.1454385822692,1.,-1.77313777896194));
#32128=CARTESIAN_POINT('Ctrl Pts',(1.14000548336975,-1.,-1.76997111386769));
#32129=CARTESIAN_POINT('Ctrl Pts',(1.14000548336975,1.,-1.76997111386769));
#32130=CARTESIAN_POINT('Ctrl Pts',(1.1346029180462,-1.,-1.76677384551862));
#32131=CARTESIAN_POINT('Ctrl Pts',(1.1346029180462,1.,-1.76677384551862));
#32132=CARTESIAN_POINT('Ctrl Pts',(1.12923123555075,-1.,-1.7635457196617));
#32133=CARTESIAN_POINT('Ctrl Pts',(1.12923123555075,1.,-1.7635457196617));
#32134=CARTESIAN_POINT('Ctrl Pts',(1.12389096855086,-1.,-1.76028671825096));
#32135=CARTESIAN_POINT('Ctrl Pts',(1.12389096855086,1.,-1.76028671825096));
#32136=CARTESIAN_POINT('Ctrl Pts',(1.11858293216763,-1.,-1.75699720772105));
#32137=CARTESIAN_POINT('Ctrl Pts',(1.11858293216763,1.,-1.75699720772105));
#32138=CARTESIAN_POINT('Ctrl Pts',(1.11330807582551,-1.,-1.7536777209463));
#32139=CARTESIAN_POINT('Ctrl Pts',(1.11330807582551,1.,-1.7536777209463));
#32140=CARTESIAN_POINT('Ctrl Pts',(1.10806728183007,-1.,-1.7503286607592));
#32141=CARTESIAN_POINT('Ctrl Pts',(1.10806728183007,1.,-1.7503286607592));
#32142=CARTESIAN_POINT('Ctrl Pts',(1.10286118991143,-1.,-1.74695004214923));
#32143=CARTESIAN_POINT('Ctrl Pts',(1.10286118991143,1.,-1.74695004214923));
#32144=CARTESIAN_POINT('Ctrl Pts',(1.09768999241225,-1.,-1.74354119236208));
#32145=CARTESIAN_POINT('Ctrl Pts',(1.09768999241225,1.,-1.74354119236208));
#32146=CARTESIAN_POINT('Ctrl Pts',(1.09255329056493,-1.,-1.74010053962247));
#32147=CARTESIAN_POINT('Ctrl Pts',(1.09255329056493,1.,-1.74010053962247));
#32148=CARTESIAN_POINT('Ctrl Pts',(1.08745056285427,-1.,-1.73662628326091));
#32149=CARTESIAN_POINT('Ctrl Pts',(1.08745056285427,1.,-1.73662628326091));
#32150=CARTESIAN_POINT('Ctrl Pts',(1.08238162784749,-1.,-1.73311705663407));
#32151=CARTESIAN_POINT('Ctrl Pts',(1.08238162784749,1.,-1.73311705663407));
#32152=CARTESIAN_POINT('Ctrl Pts',(1.0773470373727,-1.,-1.72957248977424));
#32153=CARTESIAN_POINT('Ctrl Pts',(1.0773470373727,1.,-1.72957248977424));
#32154=CARTESIAN_POINT('Ctrl Pts',(1.07234866990252,-1.,-1.72599406198488));
#32155=CARTESIAN_POINT('Ctrl Pts',(1.07234866990252,1.,-1.72599406198488));
#32156=CARTESIAN_POINT('Ctrl Pts',(1.06738966975462,-1.,-1.72238500928453));
#32157=CARTESIAN_POINT('Ctrl Pts',(1.06738966975462,1.,-1.72238500928453));
#32158=CARTESIAN_POINT('Ctrl Pts',(1.06247324680647,-1.,-1.71874858456904));
#32159=CARTESIAN_POINT('Ctrl Pts',(1.06247324680647,1.,-1.71874858456904));
#32160=CARTESIAN_POINT('Ctrl Pts',(1.05760163192479,-1.,-1.7150865442702));
#32161=CARTESIAN_POINT('Ctrl Pts',(1.05760163192479,1.,-1.7150865442702));
#32162=CARTESIAN_POINT('Ctrl Pts',(1.05277517202855,-1.,-1.71139783543989));
#32163=CARTESIAN_POINT('Ctrl Pts',(1.05277517202855,1.,-1.71139783543989));
#32164=CARTESIAN_POINT('Ctrl Pts',(1.04799085404995,-1.,-1.70767646263649));
#32165=CARTESIAN_POINT('Ctrl Pts',(1.04799085404995,1.,-1.70767646263649));
#32166=CARTESIAN_POINT('Ctrl Pts',(1.04324363334554,-1.,-1.70391338707982));
#32167=CARTESIAN_POINT('Ctrl Pts',(1.04324363334554,1.,-1.70391338707982));
#32168=CARTESIAN_POINT('Ctrl Pts',(1.03852922490789,-1.,-1.70010052930962));
#32169=CARTESIAN_POINT('Ctrl Pts',(1.03852922490789,1.,-1.70010052930962));
#32170=CARTESIAN_POINT('Ctrl Pts',(1.03384646003588,-1.,-1.69623414782771));
#32171=CARTESIAN_POINT('Ctrl Pts',(1.03384646003588,1.,-1.69623414782771));
#32172=CARTESIAN_POINT('Ctrl Pts',(1.02919977579147,-1.,-1.69231840863458));
#32173=CARTESIAN_POINT('Ctrl Pts',(1.02919977579147,1.,-1.69231840863458));
#32174=CARTESIAN_POINT('Ctrl Pts',(1.02460180535255,-1.,-1.68836910178447));
#32175=CARTESIAN_POINT('Ctrl Pts',(1.02460180535255,1.,-1.68836910178447));
#32176=CARTESIAN_POINT('Ctrl Pts',(1.02006795074201,-1.,-1.68440578021706));
#32177=CARTESIAN_POINT('Ctrl Pts',(1.02006795074201,1.,-1.68440578021706));
#32178=CARTESIAN_POINT('Ctrl Pts',(1.01561026162773,-1.,-1.68044289894798));
#32179=CARTESIAN_POINT('Ctrl Pts',(1.01561026162773,1.,-1.68044289894798));
#32180=CARTESIAN_POINT('Ctrl Pts',(1.01123236493511,-1.,-1.67648246776464));
#32181=CARTESIAN_POINT('Ctrl Pts',(1.01123236493511,1.,-1.67648246776464));
#32182=CARTESIAN_POINT('Ctrl Pts',(1.00692206696414,-1.,-1.67250335383293));
#32183=CARTESIAN_POINT('Ctrl Pts',(1.00692206696414,1.,-1.67250335383293));
#32184=CARTESIAN_POINT('Ctrl Pts',(1.00265091003727,-1.,-1.66846059277303));
#32185=CARTESIAN_POINT('Ctrl Pts',(1.00265091003727,1.,-1.66846059277303));
#32186=CARTESIAN_POINT('Ctrl Pts',(0.998389654952757,-1.,-1.66430758030376));
#32187=CARTESIAN_POINT('Ctrl Pts',(0.998389654952757,1.,-1.66430758030376));
#32188=CARTESIAN_POINT('Ctrl Pts',(0.994121836661305,-1.,-1.66001553809947));
#32189=CARTESIAN_POINT('Ctrl Pts',(0.994121836661305,1.,-1.66001553809947));
#32190=CARTESIAN_POINT('Ctrl Pts',(0.989855627854164,-1.,-1.65559044289699));
#32191=CARTESIAN_POINT('Ctrl Pts',(0.989855627854164,1.,-1.65559044289699));
#32192=CARTESIAN_POINT('Ctrl Pts',(0.98564262292082,-1.,-1.65110016612638));
#32193=CARTESIAN_POINT('Ctrl Pts',(0.98564262292082,1.,-1.65110016612638));
#32194=CARTESIAN_POINT('Ctrl Pts',(0.981562530939489,-1.,-1.64665139190656));
#32195=CARTESIAN_POINT('Ctrl Pts',(0.981562530939489,1.,-1.64665139190656));
#32196=CARTESIAN_POINT('Ctrl Pts',(0.977689794119416,-1.,-1.64233990826687));
#32197=CARTESIAN_POINT('Ctrl Pts',(0.977689794119416,1.,-1.64233990826687));
#32198=CARTESIAN_POINT('Ctrl Pts',(0.974066058287418,-1.,-1.63820952658144));
#32199=CARTESIAN_POINT('Ctrl Pts',(0.974066058287418,1.,-1.63820952658144));
#32200=CARTESIAN_POINT('Ctrl Pts',(0.970669715997509,-1.,-1.63420665729798));
#32201=CARTESIAN_POINT('Ctrl Pts',(0.970669715997509,1.,-1.63420665729798));
#32202=CARTESIAN_POINT('Ctrl Pts',(0.967387853230345,-1.,-1.63013849959462));
#32203=CARTESIAN_POINT('Ctrl Pts',(0.967387853230345,1.,-1.63013849959462));
#32204=CARTESIAN_POINT('Ctrl Pts',(0.964046107040535,-1.,-1.62571930670187));
#32205=CARTESIAN_POINT('Ctrl Pts',(0.964046107040535,1.,-1.62571930670187));
#32206=CARTESIAN_POINT('Ctrl Pts',(0.960438326101728,-1.,-1.62061638140221));
#32207=CARTESIAN_POINT('Ctrl Pts',(0.960438326101728,1.,-1.62061638140221));
#32208=CARTESIAN_POINT('Ctrl Pts',(0.95635442292067,-1.,-1.61449324337085));
#32209=CARTESIAN_POINT('Ctrl Pts',(0.95635442292067,1.,-1.61449324337085));
#32210=CARTESIAN_POINT('Ctrl Pts',(0.951613284356035,-1.,-1.60706069896936));
#32211=CARTESIAN_POINT('Ctrl Pts',(0.951613284356035,1.,-1.60706069896936));
#32212=CARTESIAN_POINT('Ctrl Pts',(0.946078063315257,-1.,-1.59810042043673));
#32213=CARTESIAN_POINT('Ctrl Pts',(0.946078063315257,1.,-1.59810042043673));
#32214=CARTESIAN_POINT('Ctrl Pts',(0.939646377893399,-1.,-1.58744937487176));
#32215=CARTESIAN_POINT('Ctrl Pts',(0.939646377893399,1.,-1.58744937487176));
#32216=CARTESIAN_POINT('Ctrl Pts',(0.932246680108685,-1.,-1.57499388382243));
#32217=CARTESIAN_POINT('Ctrl Pts',(0.932246680108685,1.,-1.57499388382243));
#32218=CARTESIAN_POINT('Ctrl Pts',(0.923832188944341,-1.,-1.56065988578893));
#32219=CARTESIAN_POINT('Ctrl Pts',(0.923832188944341,1.,-1.56065988578893));
#32220=CARTESIAN_POINT('Ctrl Pts',(0.914375919026456,-1.,-1.54440491149498));
#32221=CARTESIAN_POINT('Ctrl Pts',(0.914375919026456,1.,-1.54440491149498));
#32222=CARTESIAN_POINT('Ctrl Pts',(0.905967409625651,-1.,-1.52984849887993));
#32223=CARTESIAN_POINT('Ctrl Pts',(0.905967409625651,1.,-1.52984849887993));
#32224=CARTESIAN_POINT('Ctrl Pts',(0.89918504748351,-1.,-1.51805569590094));
#32225=CARTESIAN_POINT('Ctrl Pts',(0.89918504748351,1.,-1.51805569590094));
#32226=CARTESIAN_POINT('Ctrl Pts',(0.894452006964543,-1.,-1.50980486806688));
#32227=CARTESIAN_POINT('Ctrl Pts',(0.894452006964543,1.,-1.50980486806688));
#32228=CARTESIAN_POINT('Ctrl Pts',(0.892032620296855,-1.,-1.5055822144029));
#32229=CARTESIAN_POINT('Ctrl Pts',(0.892032620296855,1.,-1.5055822144029));
#32230=CARTESIAN_POINT('',(1.23627494547115,1.,-1.81978687191668));
#32231=CARTESIAN_POINT('Ctrl Pts',(1.23627494547115,1.,-1.81978687191668));
#32232=CARTESIAN_POINT('Ctrl Pts',(1.23509651170476,1.,-1.81925017193666));
#32233=CARTESIAN_POINT('Ctrl Pts',(1.2327422452705,1.,-1.81817389921279));
#32234=CARTESIAN_POINT('Ctrl Pts',(1.2292186489137,1.,-1.8165508718364));
#32235=CARTESIAN_POINT('Ctrl Pts',(1.2245361330495,1.,-1.81436959210434));
#32236=CARTESIAN_POINT('Ctrl Pts',(1.21870906103557,1.,-1.81161420806656));
#32237=CARTESIAN_POINT('Ctrl Pts',(1.21290815708314,1.,-1.80882996917129));
#32238=CARTESIAN_POINT('Ctrl Pts',(1.20713356605475,1.,-1.80601678480707));
#32239=CARTESIAN_POINT('Ctrl Pts',(1.20138548938974,1.,-1.80317454838603));
#32240=CARTESIAN_POINT('Ctrl Pts',(1.19566418930242,1.,-1.80030314369879));
#32241=CARTESIAN_POINT('Ctrl Pts',(1.18996997934445,1.,-1.79740245923478));
#32242=CARTESIAN_POINT('Ctrl Pts',(1.18430321697432,1.,-1.79447240321515));
#32243=CARTESIAN_POINT('Ctrl Pts',(1.17866429440809,1.,-1.79151291552689));
#32244=CARTESIAN_POINT('Ctrl Pts',(1.17305363177328,1.,-1.78852398877617));
#32245=CARTESIAN_POINT('Ctrl Pts',(1.16747166312303,1.,-1.78550566040443));
#32246=CARTESIAN_POINT('Ctrl Pts',(1.16191881298499,1.,-1.78245795881009));
#32247=CARTESIAN_POINT('Ctrl Pts',(1.15639547194698,1.,-1.77938085564275));
#32248=CARTESIAN_POINT('Ctrl Pts',(1.15090197841514,1.,-1.7762742255701));
#32249=CARTESIAN_POINT('Ctrl Pts',(1.1454385822692,1.,-1.77313777896194));
#32250=CARTESIAN_POINT('Ctrl Pts',(1.14000548336975,1.,-1.76997111386769));
#32251=CARTESIAN_POINT('Ctrl Pts',(1.1346029180462,1.,-1.76677384551862));
#32252=CARTESIAN_POINT('Ctrl Pts',(1.12923123555075,1.,-1.7635457196617));
#32253=CARTESIAN_POINT('Ctrl Pts',(1.12389096855086,1.,-1.76028671825096));
#32254=CARTESIAN_POINT('Ctrl Pts',(1.11858293216763,1.,-1.75699720772105));
#32255=CARTESIAN_POINT('Ctrl Pts',(1.11330807582551,1.,-1.7536777209463));
#32256=CARTESIAN_POINT('Ctrl Pts',(1.10806728183007,1.,-1.7503286607592));
#32257=CARTESIAN_POINT('Ctrl Pts',(1.10286118991143,1.,-1.74695004214923));
#32258=CARTESIAN_POINT('Ctrl Pts',(1.09768999241225,1.,-1.74354119236208));
#32259=CARTESIAN_POINT('Ctrl Pts',(1.09255329056493,1.,-1.74010053962247));
#32260=CARTESIAN_POINT('Ctrl Pts',(1.08745056285427,1.,-1.73662628326091));
#32261=CARTESIAN_POINT('Ctrl Pts',(1.08238162784749,1.,-1.73311705663407));
#32262=CARTESIAN_POINT('Ctrl Pts',(1.0773470373727,1.,-1.72957248977424));
#32263=CARTESIAN_POINT('Ctrl Pts',(1.07234866990252,1.,-1.72599406198488));
#32264=CARTESIAN_POINT('Ctrl Pts',(1.06738966975462,1.,-1.72238500928453));
#32265=CARTESIAN_POINT('Ctrl Pts',(1.06247324680647,1.,-1.71874858456904));
#32266=CARTESIAN_POINT('Ctrl Pts',(1.05760163192479,1.,-1.7150865442702));
#32267=CARTESIAN_POINT('Ctrl Pts',(1.05277517202855,1.,-1.71139783543989));
#32268=CARTESIAN_POINT('Ctrl Pts',(1.04799085404995,1.,-1.70767646263649));
#32269=CARTESIAN_POINT('Ctrl Pts',(1.04324363334554,1.,-1.70391338707982));
#32270=CARTESIAN_POINT('Ctrl Pts',(1.03852922490789,1.,-1.70010052930962));
#32271=CARTESIAN_POINT('Ctrl Pts',(1.03384646003588,1.,-1.69623414782771));
#32272=CARTESIAN_POINT('Ctrl Pts',(1.02919977579147,1.,-1.69231840863458));
#32273=CARTESIAN_POINT('Ctrl Pts',(1.02460180535255,1.,-1.68836910178447));
#32274=CARTESIAN_POINT('Ctrl Pts',(1.02006795074201,1.,-1.68440578021706));
#32275=CARTESIAN_POINT('Ctrl Pts',(1.01561026162773,1.,-1.68044289894798));
#32276=CARTESIAN_POINT('Ctrl Pts',(1.01123236493511,1.,-1.67648246776464));
#32277=CARTESIAN_POINT('Ctrl Pts',(1.00692206696414,1.,-1.67250335383293));
#32278=CARTESIAN_POINT('Ctrl Pts',(1.00265091003727,1.,-1.66846059277303));
#32279=CARTESIAN_POINT('Ctrl Pts',(0.998389654952757,1.,-1.66430758030376));
#32280=CARTESIAN_POINT('Ctrl Pts',(0.994121836661305,1.,-1.66001553809947));
#32281=CARTESIAN_POINT('Ctrl Pts',(0.989855627854164,1.,-1.65559044289699));
#32282=CARTESIAN_POINT('Ctrl Pts',(0.98564262292082,1.,-1.65110016612638));
#32283=CARTESIAN_POINT('Ctrl Pts',(0.981562530939489,1.,-1.64665139190656));
#32284=CARTESIAN_POINT('Ctrl Pts',(0.977689794119416,1.,-1.64233990826687));
#32285=CARTESIAN_POINT('Ctrl Pts',(0.974066058287418,1.,-1.63820952658144));
#32286=CARTESIAN_POINT('Ctrl Pts',(0.970669715997509,1.,-1.63420665729798));
#32287=CARTESIAN_POINT('Ctrl Pts',(0.967387853230345,1.,-1.63013849959462));
#32288=CARTESIAN_POINT('Ctrl Pts',(0.964046107040535,1.,-1.62571930670187));
#32289=CARTESIAN_POINT('Ctrl Pts',(0.960438326101728,1.,-1.62061638140221));
#32290=CARTESIAN_POINT('Ctrl Pts',(0.95635442292067,1.,-1.61449324337085));
#32291=CARTESIAN_POINT('Ctrl Pts',(0.951613284356035,1.,-1.60706069896936));
#32292=CARTESIAN_POINT('Ctrl Pts',(0.946078063315257,1.,-1.59810042043673));
#32293=CARTESIAN_POINT('Ctrl Pts',(0.939646377893399,1.,-1.58744937487176));
#32294=CARTESIAN_POINT('Ctrl Pts',(0.932246680108685,1.,-1.57499388382243));
#32295=CARTESIAN_POINT('Ctrl Pts',(0.923832188944341,1.,-1.56065988578893));
#32296=CARTESIAN_POINT('Ctrl Pts',(0.914375919026456,1.,-1.54440491149498));
#32297=CARTESIAN_POINT('Ctrl Pts',(0.905967409625651,1.,-1.52984849887993));
#32298=CARTESIAN_POINT('Ctrl Pts',(0.89918504748351,1.,-1.51805569590094));
#32299=CARTESIAN_POINT('Ctrl Pts',(0.894452006964543,1.,-1.50980486806688));
#32300=CARTESIAN_POINT('Ctrl Pts',(0.892032620296855,1.,-1.5055822144029));
#32301=CARTESIAN_POINT('',(1.23627494547115,0.,-1.81978687191668));
#32302=CARTESIAN_POINT('Origin',(1.34869019493419,0.,-1.73811241238545));
#32303=CARTESIAN_POINT('',(1.34869019493419,1.,-1.73811241238545));
#32304=CARTESIAN_POINT('',(1.23627494547115,1.,-1.81978687191668));
#32305=CARTESIAN_POINT('',(1.34869019493419,0.,-1.73811241238545));
#32306=CARTESIAN_POINT('Ctrl Pts',(1.15624053661742,-1.,-1.31362392696032));
#32307=CARTESIAN_POINT('Ctrl Pts',(1.15624053661742,1.,-1.31362392696032));
#32308=CARTESIAN_POINT('Ctrl Pts',(1.15950888730809,-1.,-1.31722977216397));
#32309=CARTESIAN_POINT('Ctrl Pts',(1.15950888730809,1.,-1.31722977216397));
#32310=CARTESIAN_POINT('Ctrl Pts',(1.16589330093588,-1.,-1.32428080721772));
#32311=CARTESIAN_POINT('Ctrl Pts',(1.16589330093588,1.,-1.32428080721772));
#32312=CARTESIAN_POINT('Ctrl Pts',(1.17501305789857,-1.,-1.33437539347008));
#32313=CARTESIAN_POINT('Ctrl Pts',(1.17501305789857,1.,-1.33437539347008));
#32314=CARTESIAN_POINT('Ctrl Pts',(1.18625865667441,-1.,-1.34687054001093));
#32315=CARTESIAN_POINT('Ctrl Pts',(1.18625865667441,1.,-1.34687054001093));
#32316=CARTESIAN_POINT('Ctrl Pts',(1.1987959077932,-1.,-1.36088705043885));
#32317=CARTESIAN_POINT('Ctrl Pts',(1.1987959077932,1.,-1.36088705043885));
#32318=CARTESIAN_POINT('Ctrl Pts',(1.20982812925645,-1.,-1.37331915607905));
#32319=CARTESIAN_POINT('Ctrl Pts',(1.20982812925645,1.,-1.37331915607905));
#32320=CARTESIAN_POINT('Ctrl Pts',(1.21938737280852,-1.,-1.38420564527715));
#32321=CARTESIAN_POINT('Ctrl Pts',(1.21938737280852,1.,-1.38420564527715));
#32322=CARTESIAN_POINT('Ctrl Pts',(1.22752961899387,-1.,-1.39361389568796));
#32323=CARTESIAN_POINT('Ctrl Pts',(1.22752961899387,1.,-1.39361389568796));
#32324=CARTESIAN_POINT('Ctrl Pts',(1.23434087290423,-1.,-1.40164708206106));
#32325=CARTESIAN_POINT('Ctrl Pts',(1.23434087290423,1.,-1.40164708206106));
#32326=CARTESIAN_POINT('Ctrl Pts',(1.23994455029534,-1.,-1.40845295531283));
#32327=CARTESIAN_POINT('Ctrl Pts',(1.23994455029534,1.,-1.40845295531283));
#32328=CARTESIAN_POINT('Ctrl Pts',(1.24450600513056,-1.,-1.41422913175179));
#32329=CARTESIAN_POINT('Ctrl Pts',(1.24450600513056,1.,-1.41422913175179));
#32330=CARTESIAN_POINT('Ctrl Pts',(1.24824430986571,-1.,-1.41923722596025));
#32331=CARTESIAN_POINT('Ctrl Pts',(1.24824430986571,1.,-1.41923722596025));
#32332=CARTESIAN_POINT('Ctrl Pts',(1.2514145557001,-1.,-1.42378102115575));
#32333=CARTESIAN_POINT('Ctrl Pts',(1.2514145557001,1.,-1.42378102115575));
#32334=CARTESIAN_POINT('Ctrl Pts',(1.25426945222639,-1.,-1.42815938799387));
#32335=CARTESIAN_POINT('Ctrl Pts',(1.25426945222639,1.,-1.42815938799387));
#32336=CARTESIAN_POINT('Ctrl Pts',(1.25702687965755,-1.,-1.43262645609691));
#32337=CARTESIAN_POINT('Ctrl Pts',(1.25702687965755,1.,-1.43262645609691));
#32338=CARTESIAN_POINT('Ctrl Pts',(1.25983531012005,-1.,-1.43734919180848));
#32339=CARTESIAN_POINT('Ctrl Pts',(1.25983531012005,1.,-1.43734919180848));
#32340=CARTESIAN_POINT('Ctrl Pts',(1.26273903323858,-1.,-1.44236470511303));
#32341=CARTESIAN_POINT('Ctrl Pts',(1.26273903323858,1.,-1.44236470511303));
#32342=CARTESIAN_POINT('Ctrl Pts',(1.26570925118868,-1.,-1.44761985001662));
#32343=CARTESIAN_POINT('Ctrl Pts',(1.26570925118868,1.,-1.44761985001662));
#32344=CARTESIAN_POINT('Ctrl Pts',(1.2686778680489,-1.,-1.45301422764247));
#32345=CARTESIAN_POINT('Ctrl Pts',(1.2686778680489,1.,-1.45301422764247));
#32346=CARTESIAN_POINT('Ctrl Pts',(1.27156805265289,-1.,-1.45843906294697));
#32347=CARTESIAN_POINT('Ctrl Pts',(1.27156805265289,1.,-1.45843906294697));
#32348=CARTESIAN_POINT('Ctrl Pts',(1.27433119897822,-1.,-1.46382431332476));
#32349=CARTESIAN_POINT('Ctrl Pts',(1.27433119897822,1.,-1.46382431332476));
#32350=CARTESIAN_POINT('Ctrl Pts',(1.27696414831089,-1.,-1.46916035917133));
#32351=CARTESIAN_POINT('Ctrl Pts',(1.27696414831089,1.,-1.46916035917133));
#32352=CARTESIAN_POINT('Ctrl Pts',(1.2794891824849,-1.,-1.4744717526707));
#32353=CARTESIAN_POINT('Ctrl Pts',(1.2794891824849,1.,-1.4744717526707));
#32354=CARTESIAN_POINT('Ctrl Pts',(1.28194158939517,-1.,-1.47980070347096));
#32355=CARTESIAN_POINT('Ctrl Pts',(1.28194158939517,1.,-1.47980070347096));
#32356=CARTESIAN_POINT('Ctrl Pts',(1.28435533880201,-1.,-1.4851881711891));
#32357=CARTESIAN_POINT('Ctrl Pts',(1.28435533880201,1.,-1.4851881711891));
#32358=CARTESIAN_POINT('Ctrl Pts',(1.2867467611644,-1.,-1.4906522831278));
#32359=CARTESIAN_POINT('Ctrl Pts',(1.2867467611644,1.,-1.4906522831278));
#32360=CARTESIAN_POINT('Ctrl Pts',(1.28911506584254,-1.,-1.49618896881754));
#32361=CARTESIAN_POINT('Ctrl Pts',(1.28911506584254,1.,-1.49618896881754));
#32362=CARTESIAN_POINT('Ctrl Pts',(1.29145022885181,-1.,-1.50178230149776));
#32363=CARTESIAN_POINT('Ctrl Pts',(1.29145022885181,1.,-1.50178230149776));
#32364=CARTESIAN_POINT('Ctrl Pts',(1.29373841372842,-1.,-1.50741159078365));
#32365=CARTESIAN_POINT('Ctrl Pts',(1.29373841372842,1.,-1.50741159078365));
#32366=CARTESIAN_POINT('Ctrl Pts',(1.29596850710509,-1.,-1.51305994241402));
#32367=CARTESIAN_POINT('Ctrl Pts',(1.29596850710509,1.,-1.51305994241402));
#32368=CARTESIAN_POINT('Ctrl Pts',(1.29813791800747,-1.,-1.51872184912724));
#32369=CARTESIAN_POINT('Ctrl Pts',(1.29813791800747,1.,-1.51872184912724));
#32370=CARTESIAN_POINT('Ctrl Pts',(1.30024984366328,-1.,-1.52439957861062));
#32371=CARTESIAN_POINT('Ctrl Pts',(1.30024984366328,1.,-1.52439957861062));
#32372=CARTESIAN_POINT('Ctrl Pts',(1.30231064395568,-1.,-1.53009970283891));
#32373=CARTESIAN_POINT('Ctrl Pts',(1.30231064395568,1.,-1.53009970283891));
#32374=CARTESIAN_POINT('Ctrl Pts',(1.30432735639489,-1.,-1.53582981268977));
#32375=CARTESIAN_POINT('Ctrl Pts',(1.30432735639489,1.,-1.53582981268977));
#32376=CARTESIAN_POINT('Ctrl Pts',(1.30630475189556,-1.,-1.54159462645432));
#32377=CARTESIAN_POINT('Ctrl Pts',(1.30630475189556,1.,-1.54159462645432));
#32378=CARTESIAN_POINT('Ctrl Pts',(1.30824393907473,-1.,-1.54739413957185));
#32379=CARTESIAN_POINT('Ctrl Pts',(1.30824393907473,1.,-1.54739413957185));
#32380=CARTESIAN_POINT('Ctrl Pts',(1.31014393684222,-1.,-1.55322568759481));
#32381=CARTESIAN_POINT('Ctrl Pts',(1.31014393684222,1.,-1.55322568759481));
#32382=CARTESIAN_POINT('Ctrl Pts',(1.31200264341696,-1.,-1.55908521254821));
#32383=CARTESIAN_POINT('Ctrl Pts',(1.31200264341696,1.,-1.55908521254821));
#32384=CARTESIAN_POINT('Ctrl Pts',(1.31381795281002,-1.,-1.56496872402353));
#32385=CARTESIAN_POINT('Ctrl Pts',(1.31381795281002,1.,-1.56496872402353));
#32386=CARTESIAN_POINT('Ctrl Pts',(1.31558903860016,-1.,-1.57087397835723));
#32387=CARTESIAN_POINT('Ctrl Pts',(1.31558903860016,1.,-1.57087397835723));
#32388=CARTESIAN_POINT('Ctrl Pts',(1.31731642317187,-1.,-1.5768005650559));
#32389=CARTESIAN_POINT('Ctrl Pts',(1.31731642317187,1.,-1.5768005650559));
#32390=CARTESIAN_POINT('Ctrl Pts',(1.31900135021432,-1.,-1.58274907898834));
#32391=CARTESIAN_POINT('Ctrl Pts',(1.31900135021432,1.,-1.58274907898834));
#32392=CARTESIAN_POINT('Ctrl Pts',(1.32064537110892,-1.,-1.58872057258245));
#32393=CARTESIAN_POINT('Ctrl Pts',(1.32064537110892,1.,-1.58872057258245));
#32394=CARTESIAN_POINT('Ctrl Pts',(1.32224985747682,-1.,-1.59471591079403));
#32395=CARTESIAN_POINT('Ctrl Pts',(1.32224985747682,1.,-1.59471591079403));
#32396=CARTESIAN_POINT('Ctrl Pts',(1.32381550858256,-1.,-1.60073511858687));
#32397=CARTESIAN_POINT('Ctrl Pts',(1.32381550858256,1.,-1.60073511858687));
#32398=CARTESIAN_POINT('Ctrl Pts',(1.32534250785782,-1.,-1.60677758290954));
#32399=CARTESIAN_POINT('Ctrl Pts',(1.32534250785782,1.,-1.60677758290954));
#32400=CARTESIAN_POINT('Ctrl Pts',(1.32683074483356,-1.,-1.6128423401575));
#32401=CARTESIAN_POINT('Ctrl Pts',(1.32683074483356,1.,-1.6128423401575));
#32402=CARTESIAN_POINT('Ctrl Pts',(1.32828000610449,-1.,-1.61892832270724));
#32403=CARTESIAN_POINT('Ctrl Pts',(1.32828000610449,1.,-1.61892832270724));
#32404=CARTESIAN_POINT('Ctrl Pts',(1.3296901950568,-1.,-1.62503464209797));
#32405=CARTESIAN_POINT('Ctrl Pts',(1.3296901950568,1.,-1.62503464209797));
#32406=CARTESIAN_POINT('Ctrl Pts',(1.33106149345645,-1.,-1.63116079730923));
#32407=CARTESIAN_POINT('Ctrl Pts',(1.33106149345645,1.,-1.63116079730923));
#32408=CARTESIAN_POINT('Ctrl Pts',(1.33239425103724,-1.,-1.63730653475089));
#32409=CARTESIAN_POINT('Ctrl Pts',(1.33239425103724,1.,-1.63730653475089));
#32410=CARTESIAN_POINT('Ctrl Pts',(1.33368890676572,-1.,-1.6434717485603));
#32411=CARTESIAN_POINT('Ctrl Pts',(1.33368890676572,1.,-1.6434717485603));
#32412=CARTESIAN_POINT('Ctrl Pts',(1.33494590467993,-1.,-1.6496563728683));
#32413=CARTESIAN_POINT('Ctrl Pts',(1.33494590467993,1.,-1.6496563728683));
#32414=CARTESIAN_POINT('Ctrl Pts',(1.33616559745172,-1.,-1.65586025952593));
#32415=CARTESIAN_POINT('Ctrl Pts',(1.33616559745172,1.,-1.65586025952593));
#32416=CARTESIAN_POINT('Ctrl Pts',(1.33734820885262,-1.,-1.66208312541983));
#32417=CARTESIAN_POINT('Ctrl Pts',(1.33734820885262,1.,-1.66208312541983));
#32418=CARTESIAN_POINT('Ctrl Pts',(1.33849388654388,-1.,-1.66832460783989));
#32419=CARTESIAN_POINT('Ctrl Pts',(1.33849388654388,1.,-1.66832460783989));
#32420=CARTESIAN_POINT('Ctrl Pts',(1.3396027347034,-1.,-1.67458429426086));
#32421=CARTESIAN_POINT('Ctrl Pts',(1.3396027347034,1.,-1.67458429426086));
#32422=CARTESIAN_POINT('Ctrl Pts',(1.34067485185203,-1.,-1.68086176030362));
#32423=CARTESIAN_POINT('Ctrl Pts',(1.34067485185203,1.,-1.68086176030362));
#32424=CARTESIAN_POINT('Ctrl Pts',(1.341710374848,-1.,-1.68715660868764));
#32425=CARTESIAN_POINT('Ctrl Pts',(1.341710374848,1.,-1.68715660868764));
#32426=CARTESIAN_POINT('Ctrl Pts',(1.34270948206319,-1.,-1.6934684849687));
#32427=CARTESIAN_POINT('Ctrl Pts',(1.34270948206319,1.,-1.6934684849687));
#32428=CARTESIAN_POINT('Ctrl Pts',(1.34367237124483,-1.,-1.69979707754427));
#32429=CARTESIAN_POINT('Ctrl Pts',(1.34367237124483,1.,-1.69979707754427));
#32430=CARTESIAN_POINT('Ctrl Pts',(1.34459924533831,-1.,-1.70614212266738));
#32431=CARTESIAN_POINT('Ctrl Pts',(1.34459924533831,1.,-1.70614212266738));
#32432=CARTESIAN_POINT('Ctrl Pts',(1.34549029589416,-1.,-1.71250340686822));
#32433=CARTESIAN_POINT('Ctrl Pts',(1.34549029589416,1.,-1.71250340686822));
#32434=CARTESIAN_POINT('Ctrl Pts',(1.34634568653227,-1.,-1.7188807715049));
#32435=CARTESIAN_POINT('Ctrl Pts',(1.34634568653227,1.,-1.7188807715049));
#32436=CARTESIAN_POINT('Ctrl Pts',(1.34716554819527,-1.,-1.72527410680674));
#32437=CARTESIAN_POINT('Ctrl Pts',(1.34716554819527,1.,-1.72527410680674));
#32438=CARTESIAN_POINT('Ctrl Pts',(1.34779309152035,-1.,-1.7304014965394));
#32439=CARTESIAN_POINT('Ctrl Pts',(1.34779309152035,1.,-1.7304014965394));
#32440=CARTESIAN_POINT('Ctrl Pts',(1.34824783112887,-1.,-1.73425417885907));
#32441=CARTESIAN_POINT('Ctrl Pts',(1.34824783112887,1.,-1.73425417885907));
#32442=CARTESIAN_POINT('Ctrl Pts',(1.34854391898045,-1.,-1.73682580585691));
#32443=CARTESIAN_POINT('Ctrl Pts',(1.34854391898045,1.,-1.73682580585691));
#32444=CARTESIAN_POINT('Ctrl Pts',(1.34869019493419,-1.,-1.73811241238545));
#32445=CARTESIAN_POINT('Ctrl Pts',(1.34869019493419,1.,-1.73811241238545));
#32446=CARTESIAN_POINT('',(1.15624053661742,1.,-1.31362392696032));
#32447=CARTESIAN_POINT('Ctrl Pts',(1.15624053661742,1.,-1.31362392696032));
#32448=CARTESIAN_POINT('Ctrl Pts',(1.15950888730809,1.,-1.31722977216397));
#32449=CARTESIAN_POINT('Ctrl Pts',(1.16589330093588,1.,-1.32428080721772));
#32450=CARTESIAN_POINT('Ctrl Pts',(1.17501305789857,1.,-1.33437539347008));
#32451=CARTESIAN_POINT('Ctrl Pts',(1.18625865667441,1.,-1.34687054001093));
#32452=CARTESIAN_POINT('Ctrl Pts',(1.1987959077932,1.,-1.36088705043885));
#32453=CARTESIAN_POINT('Ctrl Pts',(1.20982812925645,1.,-1.37331915607905));
#32454=CARTESIAN_POINT('Ctrl Pts',(1.21938737280852,1.,-1.38420564527715));
#32455=CARTESIAN_POINT('Ctrl Pts',(1.22752961899387,1.,-1.39361389568796));
#32456=CARTESIAN_POINT('Ctrl Pts',(1.23434087290423,1.,-1.40164708206106));
#32457=CARTESIAN_POINT('Ctrl Pts',(1.23994455029534,1.,-1.40845295531283));
#32458=CARTESIAN_POINT('Ctrl Pts',(1.24450600513056,1.,-1.41422913175179));
#32459=CARTESIAN_POINT('Ctrl Pts',(1.24824430986571,1.,-1.41923722596025));
#32460=CARTESIAN_POINT('Ctrl Pts',(1.2514145557001,1.,-1.42378102115575));
#32461=CARTESIAN_POINT('Ctrl Pts',(1.25426945222639,1.,-1.42815938799387));
#32462=CARTESIAN_POINT('Ctrl Pts',(1.25702687965755,1.,-1.43262645609691));
#32463=CARTESIAN_POINT('Ctrl Pts',(1.25983531012005,1.,-1.43734919180848));
#32464=CARTESIAN_POINT('Ctrl Pts',(1.26273903323858,1.,-1.44236470511303));
#32465=CARTESIAN_POINT('Ctrl Pts',(1.26570925118868,1.,-1.44761985001662));
#32466=CARTESIAN_POINT('Ctrl Pts',(1.2686778680489,1.,-1.45301422764247));
#32467=CARTESIAN_POINT('Ctrl Pts',(1.27156805265289,1.,-1.45843906294697));
#32468=CARTESIAN_POINT('Ctrl Pts',(1.27433119897822,1.,-1.46382431332476));
#32469=CARTESIAN_POINT('Ctrl Pts',(1.27696414831089,1.,-1.46916035917133));
#32470=CARTESIAN_POINT('Ctrl Pts',(1.2794891824849,1.,-1.4744717526707));
#32471=CARTESIAN_POINT('Ctrl Pts',(1.28194158939517,1.,-1.47980070347096));
#32472=CARTESIAN_POINT('Ctrl Pts',(1.28435533880201,1.,-1.4851881711891));
#32473=CARTESIAN_POINT('Ctrl Pts',(1.2867467611644,1.,-1.4906522831278));
#32474=CARTESIAN_POINT('Ctrl Pts',(1.28911506584254,1.,-1.49618896881754));
#32475=CARTESIAN_POINT('Ctrl Pts',(1.29145022885181,1.,-1.50178230149776));
#32476=CARTESIAN_POINT('Ctrl Pts',(1.29373841372842,1.,-1.50741159078365));
#32477=CARTESIAN_POINT('Ctrl Pts',(1.29596850710509,1.,-1.51305994241402));
#32478=CARTESIAN_POINT('Ctrl Pts',(1.29813791800747,1.,-1.51872184912724));
#32479=CARTESIAN_POINT('Ctrl Pts',(1.30024984366328,1.,-1.52439957861062));
#32480=CARTESIAN_POINT('Ctrl Pts',(1.30231064395568,1.,-1.53009970283891));
#32481=CARTESIAN_POINT('Ctrl Pts',(1.30432735639489,1.,-1.53582981268977));
#32482=CARTESIAN_POINT('Ctrl Pts',(1.30630475189556,1.,-1.54159462645432));
#32483=CARTESIAN_POINT('Ctrl Pts',(1.30824393907473,1.,-1.54739413957185));
#32484=CARTESIAN_POINT('Ctrl Pts',(1.31014393684222,1.,-1.55322568759481));
#32485=CARTESIAN_POINT('Ctrl Pts',(1.31200264341696,1.,-1.55908521254821));
#32486=CARTESIAN_POINT('Ctrl Pts',(1.31381795281002,1.,-1.56496872402353));
#32487=CARTESIAN_POINT('Ctrl Pts',(1.31558903860016,1.,-1.57087397835723));
#32488=CARTESIAN_POINT('Ctrl Pts',(1.31731642317187,1.,-1.5768005650559));
#32489=CARTESIAN_POINT('Ctrl Pts',(1.31900135021432,1.,-1.58274907898834));
#32490=CARTESIAN_POINT('Ctrl Pts',(1.32064537110892,1.,-1.58872057258245));
#32491=CARTESIAN_POINT('Ctrl Pts',(1.32224985747682,1.,-1.59471591079403));
#32492=CARTESIAN_POINT('Ctrl Pts',(1.32381550858256,1.,-1.60073511858687));
#32493=CARTESIAN_POINT('Ctrl Pts',(1.32534250785782,1.,-1.60677758290954));
#32494=CARTESIAN_POINT('Ctrl Pts',(1.32683074483356,1.,-1.6128423401575));
#32495=CARTESIAN_POINT('Ctrl Pts',(1.32828000610449,1.,-1.61892832270724));
#32496=CARTESIAN_POINT('Ctrl Pts',(1.3296901950568,1.,-1.62503464209797));
#32497=CARTESIAN_POINT('Ctrl Pts',(1.33106149345645,1.,-1.63116079730923));
#32498=CARTESIAN_POINT('Ctrl Pts',(1.33239425103724,1.,-1.63730653475089));
#32499=CARTESIAN_POINT('Ctrl Pts',(1.33368890676572,1.,-1.6434717485603));
#32500=CARTESIAN_POINT('Ctrl Pts',(1.33494590467993,1.,-1.6496563728683));
#32501=CARTESIAN_POINT('Ctrl Pts',(1.33616559745172,1.,-1.65586025952593));
#32502=CARTESIAN_POINT('Ctrl Pts',(1.33734820885262,1.,-1.66208312541983));
#32503=CARTESIAN_POINT('Ctrl Pts',(1.33849388654388,1.,-1.66832460783989));
#32504=CARTESIAN_POINT('Ctrl Pts',(1.3396027347034,1.,-1.67458429426086));
#32505=CARTESIAN_POINT('Ctrl Pts',(1.34067485185203,1.,-1.68086176030362));
#32506=CARTESIAN_POINT('Ctrl Pts',(1.341710374848,1.,-1.68715660868764));
#32507=CARTESIAN_POINT('Ctrl Pts',(1.34270948206319,1.,-1.6934684849687));
#32508=CARTESIAN_POINT('Ctrl Pts',(1.34367237124483,1.,-1.69979707754427));
#32509=CARTESIAN_POINT('Ctrl Pts',(1.34459924533831,1.,-1.70614212266738));
#32510=CARTESIAN_POINT('Ctrl Pts',(1.34549029589416,1.,-1.71250340686822));
#32511=CARTESIAN_POINT('Ctrl Pts',(1.34634568653227,1.,-1.7188807715049));
#32512=CARTESIAN_POINT('Ctrl Pts',(1.34716554819527,1.,-1.72527410680674));
#32513=CARTESIAN_POINT('Ctrl Pts',(1.34779309152035,1.,-1.7304014965394));
#32514=CARTESIAN_POINT('Ctrl Pts',(1.34824783112887,1.,-1.73425417885907));
#32515=CARTESIAN_POINT('Ctrl Pts',(1.34854391898045,1.,-1.73682580585691));
#32516=CARTESIAN_POINT('Ctrl Pts',(1.34869019493419,1.,-1.73811241238545));
#32517=CARTESIAN_POINT('',(1.15624053661742,0.,-1.31362392696032));
#32518=CARTESIAN_POINT('Origin',(0.,0.,0.));
#32519=CARTESIAN_POINT('',(1.31362392696032,1.,-1.15624053661742));
#32520=CARTESIAN_POINT('Origin',(0.,1.,0.));
#32521=CARTESIAN_POINT('',(1.31362392696032,0.,-1.15624053661742));
#32522=CARTESIAN_POINT('Ctrl Pts',(1.73811241238545,-1.,-1.34869019493419));
#32523=CARTESIAN_POINT('Ctrl Pts',(1.73811241238545,1.,-1.34869019493419));
#32524=CARTESIAN_POINT('Ctrl Pts',(1.73682580585819,-1.,-1.34854391898145));
#32525=CARTESIAN_POINT('Ctrl Pts',(1.73682580585819,1.,-1.34854391898145));
#32526=CARTESIAN_POINT('Ctrl Pts',(1.73425417886254,-1.,-1.34824783113158));
#32527=CARTESIAN_POINT('Ctrl Pts',(1.73425417886254,1.,-1.34824783113158));
#32528=CARTESIAN_POINT('Ctrl Pts',(1.73040149654497,-1.,-1.3477930915247));
#32529=CARTESIAN_POINT('Ctrl Pts',(1.73040149654497,1.,-1.3477930915247));
#32530=CARTESIAN_POINT('Ctrl Pts',(1.72527410681298,-1.,-1.34716554820013));
#32531=CARTESIAN_POINT('Ctrl Pts',(1.72527410681298,1.,-1.34716554820013));
#32532=CARTESIAN_POINT('Ctrl Pts',(1.7188807715095,-1.,-1.34634568653586));
#32533=CARTESIAN_POINT('Ctrl Pts',(1.7188807715095,1.,-1.34634568653586));
#32534=CARTESIAN_POINT('Ctrl Pts',(1.71250340687011,-1.,-1.34549029589563));
#32535=CARTESIAN_POINT('Ctrl Pts',(1.71250340687011,1.,-1.34549029589563));
#32536=CARTESIAN_POINT('Ctrl Pts',(1.70614212266676,-1.,-1.34459924533783));
#32537=CARTESIAN_POINT('Ctrl Pts',(1.70614212266676,1.,-1.34459924533783));
#32538=CARTESIAN_POINT('Ctrl Pts',(1.69979707754221,-1.,-1.34367237124322));
#32539=CARTESIAN_POINT('Ctrl Pts',(1.69979707754221,1.,-1.34367237124322));
#32540=CARTESIAN_POINT('Ctrl Pts',(1.6934684849664,-1.,-1.34270948206139));
#32541=CARTESIAN_POINT('Ctrl Pts',(1.6934684849664,1.,-1.34270948206139));
#32542=CARTESIAN_POINT('Ctrl Pts',(1.68715660868602,-1.,-1.34171037484673));
#32543=CARTESIAN_POINT('Ctrl Pts',(1.68715660868602,1.,-1.34171037484673));
#32544=CARTESIAN_POINT('Ctrl Pts',(1.68086176030308,-1.,-1.3406748518516));
#32545=CARTESIAN_POINT('Ctrl Pts',(1.68086176030308,1.,-1.3406748518516));
#32546=CARTESIAN_POINT('Ctrl Pts',(1.67458429426126,-1.,-1.33960273470372));
#32547=CARTESIAN_POINT('Ctrl Pts',(1.67458429426126,1.,-1.33960273470372));
#32548=CARTESIAN_POINT('Ctrl Pts',(1.66832460784078,-1.,-1.33849388654458));
#32549=CARTESIAN_POINT('Ctrl Pts',(1.66832460784078,1.,-1.33849388654458));
#32550=CARTESIAN_POINT('Ctrl Pts',(1.66208312542073,-1.,-1.33734820885331));
#32551=CARTESIAN_POINT('Ctrl Pts',(1.66208312542073,1.,-1.33734820885331));
#32552=CARTESIAN_POINT('Ctrl Pts',(1.65586025952651,-1.,-1.33616559745217));
#32553=CARTESIAN_POINT('Ctrl Pts',(1.65586025952651,1.,-1.33616559745217));
#32554=CARTESIAN_POINT('Ctrl Pts',(1.64965637286843,-1.,-1.33494590468003));
#32555=CARTESIAN_POINT('Ctrl Pts',(1.64965637286843,1.,-1.33494590468003));
#32556=CARTESIAN_POINT('Ctrl Pts',(1.64347174856007,-1.,-1.33368890676554));
#32557=CARTESIAN_POINT('Ctrl Pts',(1.64347174856007,1.,-1.33368890676554));
#32558=CARTESIAN_POINT('Ctrl Pts',(1.63730653475049,-1.,-1.33239425103694));
#32559=CARTESIAN_POINT('Ctrl Pts',(1.63730653475049,1.,-1.33239425103694));
#32560=CARTESIAN_POINT('Ctrl Pts',(1.63116079730887,-1.,-1.33106149345618));
#32561=CARTESIAN_POINT('Ctrl Pts',(1.63116079730887,1.,-1.33106149345618));
#32562=CARTESIAN_POINT('Ctrl Pts',(1.62503464209777,-1.,-1.32969019505665));
#32563=CARTESIAN_POINT('Ctrl Pts',(1.62503464209777,1.,-1.32969019505665));
#32564=CARTESIAN_POINT('Ctrl Pts',(1.61892832270723,-1.,-1.32828000610448));
#32565=CARTESIAN_POINT('Ctrl Pts',(1.61892832270723,1.,-1.32828000610448));
#32566=CARTESIAN_POINT('Ctrl Pts',(1.61284234015762,-1.,-1.32683074483365));
#32567=CARTESIAN_POINT('Ctrl Pts',(1.61284234015762,1.,-1.32683074483365));
#32568=CARTESIAN_POINT('Ctrl Pts',(1.6067775829097,-1.,-1.32534250785794));
#32569=CARTESIAN_POINT('Ctrl Pts',(1.6067775829097,1.,-1.32534250785794));
#32570=CARTESIAN_POINT('Ctrl Pts',(1.600735118587,-1.,-1.32381550858266));
#32571=CARTESIAN_POINT('Ctrl Pts',(1.600735118587,1.,-1.32381550858266));
#32572=CARTESIAN_POINT('Ctrl Pts',(1.59471591079408,-1.,-1.32224985747686));
#32573=CARTESIAN_POINT('Ctrl Pts',(1.59471591079408,1.,-1.32224985747686));
#32574=CARTESIAN_POINT('Ctrl Pts',(1.58872057258244,-1.,-1.32064537110891));
#32575=CARTESIAN_POINT('Ctrl Pts',(1.58872057258244,1.,-1.32064537110891));
#32576=CARTESIAN_POINT('Ctrl Pts',(1.58274907898829,-1.,-1.31900135021428));
#32577=CARTESIAN_POINT('Ctrl Pts',(1.58274907898829,1.,-1.31900135021428));
#32578=CARTESIAN_POINT('Ctrl Pts',(1.57680056505585,-1.,-1.31731642317183));
#32579=CARTESIAN_POINT('Ctrl Pts',(1.57680056505585,1.,-1.31731642317183));
#32580=CARTESIAN_POINT('Ctrl Pts',(1.57087397835721,-1.,-1.31558903860015));
#32581=CARTESIAN_POINT('Ctrl Pts',(1.57087397835721,1.,-1.31558903860015));
#32582=CARTESIAN_POINT('Ctrl Pts',(1.56496872402352,-1.,-1.31381795281002));
#32583=CARTESIAN_POINT('Ctrl Pts',(1.56496872402352,1.,-1.31381795281002));
#32584=CARTESIAN_POINT('Ctrl Pts',(1.55908521254822,-1.,-1.31200264341696));
#32585=CARTESIAN_POINT('Ctrl Pts',(1.55908521254822,1.,-1.31200264341696));
#32586=CARTESIAN_POINT('Ctrl Pts',(1.55322568759481,-1.,-1.31014393684221));
#32587=CARTESIAN_POINT('Ctrl Pts',(1.55322568759481,1.,-1.31014393684221));
#32588=CARTESIAN_POINT('Ctrl Pts',(1.54739413957183,-1.,-1.30824393907471));
#32589=CARTESIAN_POINT('Ctrl Pts',(1.54739413957183,1.,-1.30824393907471));
#32590=CARTESIAN_POINT('Ctrl Pts',(1.54159462645428,-1.,-1.30630475189553));
#32591=CARTESIAN_POINT('Ctrl Pts',(1.54159462645428,1.,-1.30630475189553));
#32592=CARTESIAN_POINT('Ctrl Pts',(1.53582981268976,-1.,-1.30432735639487));
#32593=CARTESIAN_POINT('Ctrl Pts',(1.53582981268976,1.,-1.30432735639487));
#32594=CARTESIAN_POINT('Ctrl Pts',(1.53009970283893,-1.,-1.3023106439557));
#32595=CARTESIAN_POINT('Ctrl Pts',(1.53009970283893,1.,-1.3023106439557));
#32596=CARTESIAN_POINT('Ctrl Pts',(1.5243995786107,-1.,-1.30024984366334));
#32597=CARTESIAN_POINT('Ctrl Pts',(1.5243995786107,1.,-1.30024984366334));
#32598=CARTESIAN_POINT('Ctrl Pts',(1.51872184912735,-1.,-1.29813791800757));
#32599=CARTESIAN_POINT('Ctrl Pts',(1.51872184912735,1.,-1.29813791800757));
#32600=CARTESIAN_POINT('Ctrl Pts',(1.51305994241412,-1.,-1.29596850710518));
#32601=CARTESIAN_POINT('Ctrl Pts',(1.51305994241412,1.,-1.29596850710518));
#32602=CARTESIAN_POINT('Ctrl Pts',(1.50741159078367,-1.,-1.29373841372843));
#32603=CARTESIAN_POINT('Ctrl Pts',(1.50741159078367,1.,-1.29373841372843));
#32604=CARTESIAN_POINT('Ctrl Pts',(1.50178230149764,-1.,-1.29145022885171));
#32605=CARTESIAN_POINT('Ctrl Pts',(1.50178230149764,1.,-1.29145022885171));
#32606=CARTESIAN_POINT('Ctrl Pts',(1.49618896881729,-1.,-1.28911506584232));
#32607=CARTESIAN_POINT('Ctrl Pts',(1.49618896881729,1.,-1.28911506584232));
#32608=CARTESIAN_POINT('Ctrl Pts',(1.4906522831275,-1.,-1.28674676116415));
#32609=CARTESIAN_POINT('Ctrl Pts',(1.4906522831275,1.,-1.28674676116415));
#32610=CARTESIAN_POINT('Ctrl Pts',(1.48518817118891,-1.,-1.28435533880184));
#32611=CARTESIAN_POINT('Ctrl Pts',(1.48518817118891,1.,-1.28435533880184));
#32612=CARTESIAN_POINT('Ctrl Pts',(1.47980070347102,-1.,-1.28194158939522));
#32613=CARTESIAN_POINT('Ctrl Pts',(1.47980070347102,1.,-1.28194158939522));
#32614=CARTESIAN_POINT('Ctrl Pts',(1.4744717526711,-1.,-1.27948918248524));
#32615=CARTESIAN_POINT('Ctrl Pts',(1.4744717526711,1.,-1.27948918248524));
#32616=CARTESIAN_POINT('Ctrl Pts',(1.46916035917197,-1.,-1.27696414831144));
#32617=CARTESIAN_POINT('Ctrl Pts',(1.46916035917197,1.,-1.27696414831144));
#32618=CARTESIAN_POINT('Ctrl Pts',(1.4638243133254,-1.,-1.27433119897877));
#32619=CARTESIAN_POINT('Ctrl Pts',(1.4638243133254,1.,-1.27433119897877));
#32620=CARTESIAN_POINT('Ctrl Pts',(1.45843906294725,-1.,-1.27156805265312));
#32621=CARTESIAN_POINT('Ctrl Pts',(1.45843906294725,1.,-1.27156805265312));
#32622=CARTESIAN_POINT('Ctrl Pts',(1.45301422764205,-1.,-1.26867786804854));
#32623=CARTESIAN_POINT('Ctrl Pts',(1.45301422764205,1.,-1.26867786804854));
#32624=CARTESIAN_POINT('Ctrl Pts',(1.44761985001544,-1.,-1.26570925118767));
#32625=CARTESIAN_POINT('Ctrl Pts',(1.44761985001544,1.,-1.26570925118767));
#32626=CARTESIAN_POINT('Ctrl Pts',(1.44236470511145,-1.,-1.26273903323723));
#32627=CARTESIAN_POINT('Ctrl Pts',(1.44236470511145,1.,-1.26273903323723));
#32628=CARTESIAN_POINT('Ctrl Pts',(1.43734919180719,-1.,-1.25983531011894));
#32629=CARTESIAN_POINT('Ctrl Pts',(1.43734919180719,1.,-1.25983531011894));
#32630=CARTESIAN_POINT('Ctrl Pts',(1.43262645609679,-1.,-1.25702687965744));
#32631=CARTESIAN_POINT('Ctrl Pts',(1.43262645609679,1.,-1.25702687965744));
#32632=CARTESIAN_POINT('Ctrl Pts',(1.42815938799555,-1.,-1.25426945222783));
#32633=CARTESIAN_POINT('Ctrl Pts',(1.42815938799555,1.,-1.25426945222783));
#32634=CARTESIAN_POINT('Ctrl Pts',(1.42378102115911,-1.,-1.25141455570299));
#32635=CARTESIAN_POINT('Ctrl Pts',(1.42378102115911,1.,-1.25141455570299));
#32636=CARTESIAN_POINT('Ctrl Pts',(1.41923722596421,-1.,-1.24824430986911));
#32637=CARTESIAN_POINT('Ctrl Pts',(1.41923722596421,1.,-1.24824430986911));
#32638=CARTESIAN_POINT('Ctrl Pts',(1.41422913175437,-1.,-1.24450600513278));
#32639=CARTESIAN_POINT('Ctrl Pts',(1.41422913175437,1.,-1.24450600513278));
#32640=CARTESIAN_POINT('Ctrl Pts',(1.40845295531151,-1.,-1.23994455029421));
#32641=CARTESIAN_POINT('Ctrl Pts',(1.40845295531151,1.,-1.23994455029421));
#32642=CARTESIAN_POINT('Ctrl Pts',(1.40164708205345,-1.,-1.23434087289768));
#32643=CARTESIAN_POINT('Ctrl Pts',(1.40164708205345,1.,-1.23434087289768));
#32644=CARTESIAN_POINT('Ctrl Pts',(1.39361389567257,-1.,-1.22752961898063));
#32645=CARTESIAN_POINT('Ctrl Pts',(1.39361389567257,1.,-1.22752961898063));
#32646=CARTESIAN_POINT('Ctrl Pts',(1.38420564525391,-1.,-1.21938737278853));
#32647=CARTESIAN_POINT('Ctrl Pts',(1.38420564525391,1.,-1.21938737278853));
#32648=CARTESIAN_POINT('Ctrl Pts',(1.37331915604962,-1.,-1.20982812923113));
#32649=CARTESIAN_POINT('Ctrl Pts',(1.37331915604962,1.,-1.20982812923113));
#32650=CARTESIAN_POINT('Ctrl Pts',(1.36088705040677,-1.,-1.1987959077656));
#32651=CARTESIAN_POINT('Ctrl Pts',(1.36088705040677,1.,-1.1987959077656));
#32652=CARTESIAN_POINT('Ctrl Pts',(1.34687053998157,-1.,-1.18625865664915));
#32653=CARTESIAN_POINT('Ctrl Pts',(1.34687053998157,1.,-1.18625865664915));
#32654=CARTESIAN_POINT('Ctrl Pts',(1.33437539344842,-1.,-1.17501305787994));
#32655=CARTESIAN_POINT('Ctrl Pts',(1.33437539344842,1.,-1.17501305787994));
#32656=CARTESIAN_POINT('Ctrl Pts',(1.32428080720544,-1.,-1.16589330092532));
#32657=CARTESIAN_POINT('Ctrl Pts',(1.32428080720544,1.,-1.16589330092532));
#32658=CARTESIAN_POINT('Ctrl Pts',(1.3172297721596,-1.,-1.15950888730433));
#32659=CARTESIAN_POINT('Ctrl Pts',(1.3172297721596,1.,-1.15950888730433));
#32660=CARTESIAN_POINT('Ctrl Pts',(1.31362392696032,-1.,-1.15624053661742));
#32661=CARTESIAN_POINT('Ctrl Pts',(1.31362392696032,1.,-1.15624053661742));
#32662=CARTESIAN_POINT('',(1.73811241238545,1.,-1.34869019493419));
#32663=CARTESIAN_POINT('Ctrl Pts',(1.73811241238545,1.,-1.34869019493419));
#32664=CARTESIAN_POINT('Ctrl Pts',(1.73682580585819,1.,-1.34854391898145));
#32665=CARTESIAN_POINT('Ctrl Pts',(1.73425417886254,1.,-1.34824783113158));
#32666=CARTESIAN_POINT('Ctrl Pts',(1.73040149654497,1.,-1.3477930915247));
#32667=CARTESIAN_POINT('Ctrl Pts',(1.72527410681298,1.,-1.34716554820013));
#32668=CARTESIAN_POINT('Ctrl Pts',(1.7188807715095,1.,-1.34634568653586));
#32669=CARTESIAN_POINT('Ctrl Pts',(1.71250340687011,1.,-1.34549029589563));
#32670=CARTESIAN_POINT('Ctrl Pts',(1.70614212266676,1.,-1.34459924533783));
#32671=CARTESIAN_POINT('Ctrl Pts',(1.69979707754221,1.,-1.34367237124322));
#32672=CARTESIAN_POINT('Ctrl Pts',(1.6934684849664,1.,-1.34270948206139));
#32673=CARTESIAN_POINT('Ctrl Pts',(1.68715660868602,1.,-1.34171037484673));
#32674=CARTESIAN_POINT('Ctrl Pts',(1.68086176030308,1.,-1.3406748518516));
#32675=CARTESIAN_POINT('Ctrl Pts',(1.67458429426126,1.,-1.33960273470372));
#32676=CARTESIAN_POINT('Ctrl Pts',(1.66832460784078,1.,-1.33849388654458));
#32677=CARTESIAN_POINT('Ctrl Pts',(1.66208312542073,1.,-1.33734820885331));
#32678=CARTESIAN_POINT('Ctrl Pts',(1.65586025952651,1.,-1.33616559745217));
#32679=CARTESIAN_POINT('Ctrl Pts',(1.64965637286843,1.,-1.33494590468003));
#32680=CARTESIAN_POINT('Ctrl Pts',(1.64347174856007,1.,-1.33368890676554));
#32681=CARTESIAN_POINT('Ctrl Pts',(1.63730653475049,1.,-1.33239425103694));
#32682=CARTESIAN_POINT('Ctrl Pts',(1.63116079730887,1.,-1.33106149345618));
#32683=CARTESIAN_POINT('Ctrl Pts',(1.62503464209777,1.,-1.32969019505665));
#32684=CARTESIAN_POINT('Ctrl Pts',(1.61892832270723,1.,-1.32828000610448));
#32685=CARTESIAN_POINT('Ctrl Pts',(1.61284234015762,1.,-1.32683074483365));
#32686=CARTESIAN_POINT('Ctrl Pts',(1.6067775829097,1.,-1.32534250785794));
#32687=CARTESIAN_POINT('Ctrl Pts',(1.600735118587,1.,-1.32381550858266));
#32688=CARTESIAN_POINT('Ctrl Pts',(1.59471591079408,1.,-1.32224985747686));
#32689=CARTESIAN_POINT('Ctrl Pts',(1.58872057258244,1.,-1.32064537110891));
#32690=CARTESIAN_POINT('Ctrl Pts',(1.58274907898829,1.,-1.31900135021428));
#32691=CARTESIAN_POINT('Ctrl Pts',(1.57680056505585,1.,-1.31731642317183));
#32692=CARTESIAN_POINT('Ctrl Pts',(1.57087397835721,1.,-1.31558903860015));
#32693=CARTESIAN_POINT('Ctrl Pts',(1.56496872402352,1.,-1.31381795281002));
#32694=CARTESIAN_POINT('Ctrl Pts',(1.55908521254822,1.,-1.31200264341696));
#32695=CARTESIAN_POINT('Ctrl Pts',(1.55322568759481,1.,-1.31014393684221));
#32696=CARTESIAN_POINT('Ctrl Pts',(1.54739413957183,1.,-1.30824393907471));
#32697=CARTESIAN_POINT('Ctrl Pts',(1.54159462645428,1.,-1.30630475189553));
#32698=CARTESIAN_POINT('Ctrl Pts',(1.53582981268976,1.,-1.30432735639487));
#32699=CARTESIAN_POINT('Ctrl Pts',(1.53009970283893,1.,-1.3023106439557));
#32700=CARTESIAN_POINT('Ctrl Pts',(1.5243995786107,1.,-1.30024984366334));
#32701=CARTESIAN_POINT('Ctrl Pts',(1.51872184912735,1.,-1.29813791800757));
#32702=CARTESIAN_POINT('Ctrl Pts',(1.51305994241412,1.,-1.29596850710518));
#32703=CARTESIAN_POINT('Ctrl Pts',(1.50741159078367,1.,-1.29373841372843));
#32704=CARTESIAN_POINT('Ctrl Pts',(1.50178230149764,1.,-1.29145022885171));
#32705=CARTESIAN_POINT('Ctrl Pts',(1.49618896881729,1.,-1.28911506584232));
#32706=CARTESIAN_POINT('Ctrl Pts',(1.4906522831275,1.,-1.28674676116415));
#32707=CARTESIAN_POINT('Ctrl Pts',(1.48518817118891,1.,-1.28435533880184));
#32708=CARTESIAN_POINT('Ctrl Pts',(1.47980070347102,1.,-1.28194158939522));
#32709=CARTESIAN_POINT('Ctrl Pts',(1.4744717526711,1.,-1.27948918248524));
#32710=CARTESIAN_POINT('Ctrl Pts',(1.46916035917197,1.,-1.27696414831144));
#32711=CARTESIAN_POINT('Ctrl Pts',(1.4638243133254,1.,-1.27433119897877));
#32712=CARTESIAN_POINT('Ctrl Pts',(1.45843906294725,1.,-1.27156805265312));
#32713=CARTESIAN_POINT('Ctrl Pts',(1.45301422764205,1.,-1.26867786804854));
#32714=CARTESIAN_POINT('Ctrl Pts',(1.44761985001544,1.,-1.26570925118767));
#32715=CARTESIAN_POINT('Ctrl Pts',(1.44236470511145,1.,-1.26273903323723));
#32716=CARTESIAN_POINT('Ctrl Pts',(1.43734919180719,1.,-1.25983531011894));
#32717=CARTESIAN_POINT('Ctrl Pts',(1.43262645609679,1.,-1.25702687965744));
#32718=CARTESIAN_POINT('Ctrl Pts',(1.42815938799555,1.,-1.25426945222783));
#32719=CARTESIAN_POINT('Ctrl Pts',(1.42378102115911,1.,-1.25141455570299));
#32720=CARTESIAN_POINT('Ctrl Pts',(1.41923722596421,1.,-1.24824430986911));
#32721=CARTESIAN_POINT('Ctrl Pts',(1.41422913175437,1.,-1.24450600513278));
#32722=CARTESIAN_POINT('Ctrl Pts',(1.40845295531151,1.,-1.23994455029421));
#32723=CARTESIAN_POINT('Ctrl Pts',(1.40164708205345,1.,-1.23434087289768));
#32724=CARTESIAN_POINT('Ctrl Pts',(1.39361389567257,1.,-1.22752961898063));
#32725=CARTESIAN_POINT('Ctrl Pts',(1.38420564525391,1.,-1.21938737278853));
#32726=CARTESIAN_POINT('Ctrl Pts',(1.37331915604962,1.,-1.20982812923113));
#32727=CARTESIAN_POINT('Ctrl Pts',(1.36088705040677,1.,-1.1987959077656));
#32728=CARTESIAN_POINT('Ctrl Pts',(1.34687053998157,1.,-1.18625865664915));
#32729=CARTESIAN_POINT('Ctrl Pts',(1.33437539344842,1.,-1.17501305787994));
#32730=CARTESIAN_POINT('Ctrl Pts',(1.32428080720544,1.,-1.16589330092532));
#32731=CARTESIAN_POINT('Ctrl Pts',(1.3172297721596,1.,-1.15950888730433));
#32732=CARTESIAN_POINT('Ctrl Pts',(1.31362392696032,1.,-1.15624053661742));
#32733=CARTESIAN_POINT('',(1.73811241238545,0.,-1.34869019493419));
#32734=CARTESIAN_POINT('Origin',(1.81978687191668,0.,-1.23627494547115));
#32735=CARTESIAN_POINT('',(1.81978687191668,1.,-1.23627494547115));
#32736=CARTESIAN_POINT('',(1.73811241238545,1.,-1.34869019493419));
#32737=CARTESIAN_POINT('',(1.81978687191668,0.,-1.23627494547115));
#32738=CARTESIAN_POINT('Ctrl Pts',(1.5055822144029,-1.,-0.892032620296855));
#32739=CARTESIAN_POINT('Ctrl Pts',(1.5055822144029,1.,-0.892032620296855));
#32740=CARTESIAN_POINT('Ctrl Pts',(1.50980486807181,-1.,-0.894452006967538));
#32741=CARTESIAN_POINT('Ctrl Pts',(1.50980486807181,1.,-0.894452006967538));
#32742=CARTESIAN_POINT('Ctrl Pts',(1.51805569591479,-1.,-0.89918504749193));
#32743=CARTESIAN_POINT('Ctrl Pts',(1.51805569591479,1.,-0.89918504749193));
#32744=CARTESIAN_POINT('Ctrl Pts',(1.52984849890434,-1.,-0.905967409640499));
#32745=CARTESIAN_POINT('Ctrl Pts',(1.52984849890434,1.,-0.905967409640499));
#32746=CARTESIAN_POINT('Ctrl Pts',(1.54440491152807,-1.,-0.91437591904658));
#32747=CARTESIAN_POINT('Ctrl Pts',(1.54440491152807,1.,-0.91437591904658));
#32748=CARTESIAN_POINT('Ctrl Pts',(1.56065988582509,-1.,-0.923832188966322));
#32749=CARTESIAN_POINT('Ctrl Pts',(1.56065988582509,1.,-0.923832188966322));
#32750=CARTESIAN_POINT('Ctrl Pts',(1.57499388385561,-1.,-0.932246680128849));
#32751=CARTESIAN_POINT('Ctrl Pts',(1.57499388385561,1.,-0.932246680128849));
#32752=CARTESIAN_POINT('Ctrl Pts',(1.58744937489796,-1.,-0.939646377909319));
#32753=CARTESIAN_POINT('Ctrl Pts',(1.58744937489796,1.,-0.939646377909319));
#32754=CARTESIAN_POINT('Ctrl Pts',(1.59810042045408,-1.,-0.946078063325796));
#32755=CARTESIAN_POINT('Ctrl Pts',(1.59810042045408,1.,-0.946078063325796));
#32756=CARTESIAN_POINT('Ctrl Pts',(1.60706069897794,-1.,-0.951613284361248));
#32757=CARTESIAN_POINT('Ctrl Pts',(1.60706069897794,1.,-0.951613284361248));
#32758=CARTESIAN_POINT('Ctrl Pts',(1.61449324337233,-1.,-0.956354422921573));
#32759=CARTESIAN_POINT('Ctrl Pts',(1.61449324337233,1.,-0.956354422921573));
#32760=CARTESIAN_POINT('Ctrl Pts',(1.62061638139929,-1.,-0.960438326099958));
#32761=CARTESIAN_POINT('Ctrl Pts',(1.62061638139929,1.,-0.960438326099958));
#32762=CARTESIAN_POINT('Ctrl Pts',(1.6257193066974,-1.,-0.964046107037821));
#32763=CARTESIAN_POINT('Ctrl Pts',(1.6257193066974,1.,-0.964046107037821));
#32764=CARTESIAN_POINT('Ctrl Pts',(1.63013849959083,-1.,-0.967387853228041));
#32765=CARTESIAN_POINT('Ctrl Pts',(1.63013849959083,1.,-0.967387853228041));
#32766=CARTESIAN_POINT('Ctrl Pts',(1.63420665729609,-1.,-0.970669715996356));
#32767=CARTESIAN_POINT('Ctrl Pts',(1.63420665729609,1.,-0.970669715996356));
#32768=CARTESIAN_POINT('Ctrl Pts',(1.63820952658157,-1.,-0.974066058287501));
#32769=CARTESIAN_POINT('Ctrl Pts',(1.63820952658157,1.,-0.974066058287501));
#32770=CARTESIAN_POINT('Ctrl Pts',(1.64233990826831,-1.,-0.977689794120297));
#32771=CARTESIAN_POINT('Ctrl Pts',(1.64233990826831,1.,-0.977689794120297));
#32772=CARTESIAN_POINT('Ctrl Pts',(1.64665139190834,-1.,-0.981562530940574));
#32773=CARTESIAN_POINT('Ctrl Pts',(1.64665139190834,1.,-0.981562530940574));
#32774=CARTESIAN_POINT('Ctrl Pts',(1.6511001661277,-1.,-0.985642622921626));
#32775=CARTESIAN_POINT('Ctrl Pts',(1.6511001661277,1.,-0.985642622921626));
#32776=CARTESIAN_POINT('Ctrl Pts',(1.65559044289746,-1.,-0.98985562785445));
#32777=CARTESIAN_POINT('Ctrl Pts',(1.65559044289746,1.,-0.98985562785445));
#32778=CARTESIAN_POINT('Ctrl Pts',(1.66001553809916,-1.,-0.994121836661116));
#32779=CARTESIAN_POINT('Ctrl Pts',(1.66001553809916,1.,-0.994121836661116));
#32780=CARTESIAN_POINT('Ctrl Pts',(1.66430758030304,-1.,-0.998389654952317));
#32781=CARTESIAN_POINT('Ctrl Pts',(1.66430758030304,1.,-0.998389654952317));
#32782=CARTESIAN_POINT('Ctrl Pts',(1.66846059277231,-1.,-1.00265091003682));
#32783=CARTESIAN_POINT('Ctrl Pts',(1.66846059277231,1.,-1.00265091003682));
#32784=CARTESIAN_POINT('Ctrl Pts',(1.67250335383248,-1.,-1.00692206696387));
#32785=CARTESIAN_POINT('Ctrl Pts',(1.67250335383248,1.,-1.00692206696387));
#32786=CARTESIAN_POINT('Ctrl Pts',(1.67648246776457,-1.,-1.01123236493507));
#32787=CARTESIAN_POINT('Ctrl Pts',(1.67648246776457,1.,-1.01123236493507));
#32788=CARTESIAN_POINT('Ctrl Pts',(1.6804428989482,-1.,-1.01561026162787));
#32789=CARTESIAN_POINT('Ctrl Pts',(1.6804428989482,1.,-1.01561026162787));
#32790=CARTESIAN_POINT('Ctrl Pts',(1.68440578021739,-1.,-1.02006795074222));
#32791=CARTESIAN_POINT('Ctrl Pts',(1.68440578021739,1.,-1.02006795074222));
#32792=CARTESIAN_POINT('Ctrl Pts',(1.68836910178475,-1.,-1.02460180535272));
#32793=CARTESIAN_POINT('Ctrl Pts',(1.68836910178475,1.,-1.02460180535272));
#32794=CARTESIAN_POINT('Ctrl Pts',(1.69231840863471,-1.,-1.02919977579155));
#32795=CARTESIAN_POINT('Ctrl Pts',(1.69231840863471,1.,-1.02919977579155));
#32796=CARTESIAN_POINT('Ctrl Pts',(1.69623414782769,-1.,-1.03384646003587));
#32797=CARTESIAN_POINT('Ctrl Pts',(1.69623414782769,1.,-1.03384646003587));
#32798=CARTESIAN_POINT('Ctrl Pts',(1.70010052930951,-1.,-1.03852922490782));
#32799=CARTESIAN_POINT('Ctrl Pts',(1.70010052930951,1.,-1.03852922490782));
#32800=CARTESIAN_POINT('Ctrl Pts',(1.70391338707969,-1.,-1.04324363334546));
#32801=CARTESIAN_POINT('Ctrl Pts',(1.70391338707969,1.,-1.04324363334546));
#32802=CARTESIAN_POINT('Ctrl Pts',(1.70767646263641,-1.,-1.0479908540499));
#32803=CARTESIAN_POINT('Ctrl Pts',(1.70767646263641,1.,-1.0479908540499));
#32804=CARTESIAN_POINT('Ctrl Pts',(1.71139783543986,-1.,-1.05277517202854));
#32805=CARTESIAN_POINT('Ctrl Pts',(1.71139783543986,1.,-1.05277517202854));
#32806=CARTESIAN_POINT('Ctrl Pts',(1.71508654427022,-1.,-1.05760163192481));
#32807=CARTESIAN_POINT('Ctrl Pts',(1.71508654427022,1.,-1.05760163192481));
#32808=CARTESIAN_POINT('Ctrl Pts',(1.71874858456908,-1.,-1.0624732468065));
#32809=CARTESIAN_POINT('Ctrl Pts',(1.71874858456908,1.,-1.0624732468065));
#32810=CARTESIAN_POINT('Ctrl Pts',(1.72238500928456,-1.,-1.06738966975463));
#32811=CARTESIAN_POINT('Ctrl Pts',(1.72238500928456,1.,-1.06738966975463));
#32812=CARTESIAN_POINT('Ctrl Pts',(1.72599406198489,-1.,-1.07234866990252));
#32813=CARTESIAN_POINT('Ctrl Pts',(1.72599406198489,1.,-1.07234866990252));
#32814=CARTESIAN_POINT('Ctrl Pts',(1.72957248977424,-1.,-1.0773470373727));
#32815=CARTESIAN_POINT('Ctrl Pts',(1.72957248977424,1.,-1.0773470373727));
#32816=CARTESIAN_POINT('Ctrl Pts',(1.73311705663407,-1.,-1.08238162784749));
#32817=CARTESIAN_POINT('Ctrl Pts',(1.73311705663407,1.,-1.08238162784749));
#32818=CARTESIAN_POINT('Ctrl Pts',(1.73662628326093,-1.,-1.08745056285429));
#32819=CARTESIAN_POINT('Ctrl Pts',(1.73662628326093,1.,-1.08745056285429));
#32820=CARTESIAN_POINT('Ctrl Pts',(1.74010053962252,-1.,-1.09255329056496));
#32821=CARTESIAN_POINT('Ctrl Pts',(1.74010053962252,1.,-1.09255329056496));
#32822=CARTESIAN_POINT('Ctrl Pts',(1.74354119236212,-1.,-1.09768999241229));
#32823=CARTESIAN_POINT('Ctrl Pts',(1.74354119236212,1.,-1.09768999241229));
#32824=CARTESIAN_POINT('Ctrl Pts',(1.74695004214924,-1.,-1.10286118991144));
#32825=CARTESIAN_POINT('Ctrl Pts',(1.74695004214924,1.,-1.10286118991144));
#32826=CARTESIAN_POINT('Ctrl Pts',(1.75032866075914,-1.,-1.10806728183003));
#32827=CARTESIAN_POINT('Ctrl Pts',(1.75032866075914,1.,-1.10806728183003));
#32828=CARTESIAN_POINT('Ctrl Pts',(1.75367772094617,-1.,-1.11330807582542));
#32829=CARTESIAN_POINT('Ctrl Pts',(1.75367772094617,1.,-1.11330807582542));
#32830=CARTESIAN_POINT('Ctrl Pts',(1.75699720772089,-1.,-1.11858293216752));
#32831=CARTESIAN_POINT('Ctrl Pts',(1.75699720772089,1.,-1.11858293216752));
#32832=CARTESIAN_POINT('Ctrl Pts',(1.76028671825084,-1.,-1.12389096855078));
#32833=CARTESIAN_POINT('Ctrl Pts',(1.76028671825084,1.,-1.12389096855078));
#32834=CARTESIAN_POINT('Ctrl Pts',(1.76354571966171,-1.,-1.12923123555076));
#32835=CARTESIAN_POINT('Ctrl Pts',(1.76354571966171,1.,-1.12923123555076));
#32836=CARTESIAN_POINT('Ctrl Pts',(1.76677384551883,-1.,-1.13460291804635));
#32837=CARTESIAN_POINT('Ctrl Pts',(1.76677384551883,1.,-1.13460291804635));
#32838=CARTESIAN_POINT('Ctrl Pts',(1.76997111386806,-1.,-1.14000548337));
#32839=CARTESIAN_POINT('Ctrl Pts',(1.76997111386806,1.,-1.14000548337));
#32840=CARTESIAN_POINT('Ctrl Pts',(1.77313777896234,-1.,-1.14543858226948));
#32841=CARTESIAN_POINT('Ctrl Pts',(1.77313777896234,1.,-1.14543858226948));
#32842=CARTESIAN_POINT('Ctrl Pts',(1.77627422557034,-1.,-1.15090197841531));
#32843=CARTESIAN_POINT('Ctrl Pts',(1.77627422557034,1.,-1.15090197841531));
#32844=CARTESIAN_POINT('Ctrl Pts',(1.77938085564261,-1.,-1.15639547194689));
#32845=CARTESIAN_POINT('Ctrl Pts',(1.77938085564261,1.,-1.15639547194689));
#32846=CARTESIAN_POINT('Ctrl Pts',(1.78245795880949,-1.,-1.16191881298458));
#32847=CARTESIAN_POINT('Ctrl Pts',(1.78245795880949,1.,-1.16191881298458));
#32848=CARTESIAN_POINT('Ctrl Pts',(1.78550566040349,-1.,-1.16747166312239));
#32849=CARTESIAN_POINT('Ctrl Pts',(1.78550566040349,1.,-1.16747166312239));
#32850=CARTESIAN_POINT('Ctrl Pts',(1.78852398877523,-1.,-1.17305363177265));
#32851=CARTESIAN_POINT('Ctrl Pts',(1.78852398877523,1.,-1.17305363177265));
#32852=CARTESIAN_POINT('Ctrl Pts',(1.79151291552646,-1.,-1.17866429440781));
#32853=CARTESIAN_POINT('Ctrl Pts',(1.79151291552646,1.,-1.17866429440781));
#32854=CARTESIAN_POINT('Ctrl Pts',(1.79447240321572,-1.,-1.18430321697471));
#32855=CARTESIAN_POINT('Ctrl Pts',(1.79447240321572,1.,-1.18430321697471));
#32856=CARTESIAN_POINT('Ctrl Pts',(1.79740245923649,-1.,-1.1899699793456));
#32857=CARTESIAN_POINT('Ctrl Pts',(1.79740245923649,1.,-1.1899699793456));
#32858=CARTESIAN_POINT('Ctrl Pts',(1.80030314370121,-1.,-1.19566418930405));
#32859=CARTESIAN_POINT('Ctrl Pts',(1.80030314370121,1.,-1.19566418930405));
#32860=CARTESIAN_POINT('Ctrl Pts',(1.8031745483882,-1.,-1.2013854893912));
#32861=CARTESIAN_POINT('Ctrl Pts',(1.8031745483882,1.,-1.2013854893912));
#32862=CARTESIAN_POINT('Ctrl Pts',(1.80601678480772,-1.,-1.20713356605519));
#32863=CARTESIAN_POINT('Ctrl Pts',(1.80601678480772,1.,-1.20713356605519));
#32864=CARTESIAN_POINT('Ctrl Pts',(1.80882996916931,-1.,-1.2129081570818));
#32865=CARTESIAN_POINT('Ctrl Pts',(1.80882996916931,1.,-1.2129081570818));
#32866=CARTESIAN_POINT('Ctrl Pts',(1.81161420806172,-1.,-1.2187090610323));
#32867=CARTESIAN_POINT('Ctrl Pts',(1.81161420806172,1.,-1.2187090610323));
#32868=CARTESIAN_POINT('Ctrl Pts',(1.81436959209778,-1.,-1.22453613304507));
#32869=CARTESIAN_POINT('Ctrl Pts',(1.81436959209778,1.,-1.22453613304507));
#32870=CARTESIAN_POINT('Ctrl Pts',(1.81655087183054,-1.,-1.22921864890975));
#32871=CARTESIAN_POINT('Ctrl Pts',(1.81655087183054,1.,-1.22921864890975));
#32872=CARTESIAN_POINT('Ctrl Pts',(1.81817389920914,-1.,-1.23274224526804));
#32873=CARTESIAN_POINT('Ctrl Pts',(1.81817389920914,1.,-1.23274224526804));
#32874=CARTESIAN_POINT('Ctrl Pts',(1.81925017193531,-1.,-1.23509651170384));
#32875=CARTESIAN_POINT('Ctrl Pts',(1.81925017193531,1.,-1.23509651170384));
#32876=CARTESIAN_POINT('Ctrl Pts',(1.81978687191668,-1.,-1.23627494547115));
#32877=CARTESIAN_POINT('Ctrl Pts',(1.81978687191668,1.,-1.23627494547115));
#32878=CARTESIAN_POINT('',(1.5055822144029,1.,-0.892032620296855));
#32879=CARTESIAN_POINT('Ctrl Pts',(1.5055822144029,1.,-0.892032620296855));
#32880=CARTESIAN_POINT('Ctrl Pts',(1.50980486807181,1.,-0.894452006967538));
#32881=CARTESIAN_POINT('Ctrl Pts',(1.51805569591479,1.,-0.89918504749193));
#32882=CARTESIAN_POINT('Ctrl Pts',(1.52984849890434,1.,-0.905967409640499));
#32883=CARTESIAN_POINT('Ctrl Pts',(1.54440491152807,1.,-0.91437591904658));
#32884=CARTESIAN_POINT('Ctrl Pts',(1.56065988582509,1.,-0.923832188966322));
#32885=CARTESIAN_POINT('Ctrl Pts',(1.57499388385561,1.,-0.932246680128849));
#32886=CARTESIAN_POINT('Ctrl Pts',(1.58744937489796,1.,-0.939646377909319));
#32887=CARTESIAN_POINT('Ctrl Pts',(1.59810042045408,1.,-0.946078063325796));
#32888=CARTESIAN_POINT('Ctrl Pts',(1.60706069897794,1.,-0.951613284361248));
#32889=CARTESIAN_POINT('Ctrl Pts',(1.61449324337233,1.,-0.956354422921573));
#32890=CARTESIAN_POINT('Ctrl Pts',(1.62061638139929,1.,-0.960438326099958));
#32891=CARTESIAN_POINT('Ctrl Pts',(1.6257193066974,1.,-0.964046107037821));
#32892=CARTESIAN_POINT('Ctrl Pts',(1.63013849959083,1.,-0.967387853228041));
#32893=CARTESIAN_POINT('Ctrl Pts',(1.63420665729609,1.,-0.970669715996356));
#32894=CARTESIAN_POINT('Ctrl Pts',(1.63820952658157,1.,-0.974066058287501));
#32895=CARTESIAN_POINT('Ctrl Pts',(1.64233990826831,1.,-0.977689794120297));
#32896=CARTESIAN_POINT('Ctrl Pts',(1.64665139190834,1.,-0.981562530940574));
#32897=CARTESIAN_POINT('Ctrl Pts',(1.6511001661277,1.,-0.985642622921626));
#32898=CARTESIAN_POINT('Ctrl Pts',(1.65559044289746,1.,-0.98985562785445));
#32899=CARTESIAN_POINT('Ctrl Pts',(1.66001553809916,1.,-0.994121836661116));
#32900=CARTESIAN_POINT('Ctrl Pts',(1.66430758030304,1.,-0.998389654952317));
#32901=CARTESIAN_POINT('Ctrl Pts',(1.66846059277231,1.,-1.00265091003682));
#32902=CARTESIAN_POINT('Ctrl Pts',(1.67250335383248,1.,-1.00692206696387));
#32903=CARTESIAN_POINT('Ctrl Pts',(1.67648246776457,1.,-1.01123236493507));
#32904=CARTESIAN_POINT('Ctrl Pts',(1.6804428989482,1.,-1.01561026162787));
#32905=CARTESIAN_POINT('Ctrl Pts',(1.68440578021739,1.,-1.02006795074222));
#32906=CARTESIAN_POINT('Ctrl Pts',(1.68836910178475,1.,-1.02460180535272));
#32907=CARTESIAN_POINT('Ctrl Pts',(1.69231840863471,1.,-1.02919977579155));
#32908=CARTESIAN_POINT('Ctrl Pts',(1.69623414782769,1.,-1.03384646003587));
#32909=CARTESIAN_POINT('Ctrl Pts',(1.70010052930951,1.,-1.03852922490782));
#32910=CARTESIAN_POINT('Ctrl Pts',(1.70391338707969,1.,-1.04324363334546));
#32911=CARTESIAN_POINT('Ctrl Pts',(1.70767646263641,1.,-1.0479908540499));
#32912=CARTESIAN_POINT('Ctrl Pts',(1.71139783543986,1.,-1.05277517202854));
#32913=CARTESIAN_POINT('Ctrl Pts',(1.71508654427022,1.,-1.05760163192481));
#32914=CARTESIAN_POINT('Ctrl Pts',(1.71874858456908,1.,-1.0624732468065));
#32915=CARTESIAN_POINT('Ctrl Pts',(1.72238500928456,1.,-1.06738966975463));
#32916=CARTESIAN_POINT('Ctrl Pts',(1.72599406198489,1.,-1.07234866990252));
#32917=CARTESIAN_POINT('Ctrl Pts',(1.72957248977424,1.,-1.0773470373727));
#32918=CARTESIAN_POINT('Ctrl Pts',(1.73311705663407,1.,-1.08238162784749));
#32919=CARTESIAN_POINT('Ctrl Pts',(1.73662628326093,1.,-1.08745056285429));
#32920=CARTESIAN_POINT('Ctrl Pts',(1.74010053962252,1.,-1.09255329056496));
#32921=CARTESIAN_POINT('Ctrl Pts',(1.74354119236212,1.,-1.09768999241229));
#32922=CARTESIAN_POINT('Ctrl Pts',(1.74695004214924,1.,-1.10286118991144));
#32923=CARTESIAN_POINT('Ctrl Pts',(1.75032866075914,1.,-1.10806728183003));
#32924=CARTESIAN_POINT('Ctrl Pts',(1.75367772094617,1.,-1.11330807582542));
#32925=CARTESIAN_POINT('Ctrl Pts',(1.75699720772089,1.,-1.11858293216752));
#32926=CARTESIAN_POINT('Ctrl Pts',(1.76028671825084,1.,-1.12389096855078));
#32927=CARTESIAN_POINT('Ctrl Pts',(1.76354571966171,1.,-1.12923123555076));
#32928=CARTESIAN_POINT('Ctrl Pts',(1.76677384551883,1.,-1.13460291804635));
#32929=CARTESIAN_POINT('Ctrl Pts',(1.76997111386806,1.,-1.14000548337));
#32930=CARTESIAN_POINT('Ctrl Pts',(1.77313777896234,1.,-1.14543858226948));
#32931=CARTESIAN_POINT('Ctrl Pts',(1.77627422557034,1.,-1.15090197841531));
#32932=CARTESIAN_POINT('Ctrl Pts',(1.77938085564261,1.,-1.15639547194689));
#32933=CARTESIAN_POINT('Ctrl Pts',(1.78245795880949,1.,-1.16191881298458));
#32934=CARTESIAN_POINT('Ctrl Pts',(1.78550566040349,1.,-1.16747166312239));
#32935=CARTESIAN_POINT('Ctrl Pts',(1.78852398877523,1.,-1.17305363177265));
#32936=CARTESIAN_POINT('Ctrl Pts',(1.79151291552646,1.,-1.17866429440781));
#32937=CARTESIAN_POINT('Ctrl Pts',(1.79447240321572,1.,-1.18430321697471));
#32938=CARTESIAN_POINT('Ctrl Pts',(1.79740245923649,1.,-1.1899699793456));
#32939=CARTESIAN_POINT('Ctrl Pts',(1.80030314370121,1.,-1.19566418930405));
#32940=CARTESIAN_POINT('Ctrl Pts',(1.8031745483882,1.,-1.2013854893912));
#32941=CARTESIAN_POINT('Ctrl Pts',(1.80601678480772,1.,-1.20713356605519));
#32942=CARTESIAN_POINT('Ctrl Pts',(1.80882996916931,1.,-1.2129081570818));
#32943=CARTESIAN_POINT('Ctrl Pts',(1.81161420806172,1.,-1.2187090610323));
#32944=CARTESIAN_POINT('Ctrl Pts',(1.81436959209778,1.,-1.22453613304507));
#32945=CARTESIAN_POINT('Ctrl Pts',(1.81655087183054,1.,-1.22921864890975));
#32946=CARTESIAN_POINT('Ctrl Pts',(1.81817389920914,1.,-1.23274224526804));
#32947=CARTESIAN_POINT('Ctrl Pts',(1.81925017193531,1.,-1.23509651170384));
#32948=CARTESIAN_POINT('Ctrl Pts',(1.81978687191668,1.,-1.23627494547115));
#32949=CARTESIAN_POINT('',(1.5055822144029,0.,-0.892032620296855));
#32950=CARTESIAN_POINT('Origin',(0.,0.,0.));
#32951=CARTESIAN_POINT('',(1.60662857109684,1.,-0.693717979106306));
#32952=CARTESIAN_POINT('Origin',(0.,1.,0.));
#32953=CARTESIAN_POINT('',(1.60662857109684,0.,-0.693717979106308));
#32954=CARTESIAN_POINT('Ctrl Pts',(2.0698113262342,-1.,-0.745574324794401));
#32955=CARTESIAN_POINT('Ctrl Pts',(2.0698113262342,1.,-0.745574324794401));
#32956=CARTESIAN_POINT('Ctrl Pts',(2.06854248895728,-1.,-0.745832791378367));
#32957=CARTESIAN_POINT('Ctrl Pts',(2.06854248895728,1.,-0.745832791378367));
#32958=CARTESIAN_POINT('Ctrl Pts',(2.06600523016815,-1.,-0.746345871544201));
#32959=CARTESIAN_POINT('Ctrl Pts',(2.06600523016815,1.,-0.746345871544201));
#32960=CARTESIAN_POINT('Ctrl Pts',(2.06220058927826,-1.,-0.74710393278792));
#32961=CARTESIAN_POINT('Ctrl Pts',(2.06220058927826,1.,-0.74710393278792));
#32962=CARTESIAN_POINT('Ctrl Pts',(2.05713023031006,-1.,-0.748091554183803));
#32963=CARTESIAN_POINT('Ctrl Pts',(2.05713023031006,1.,-0.748091554183803));
#32964=CARTESIAN_POINT('Ctrl Pts',(2.05079645592154,-1.,-0.749287468665046));
#32965=CARTESIAN_POINT('Ctrl Pts',(2.05079645592154,1.,-0.749287468665046));
#32966=CARTESIAN_POINT('Ctrl Pts',(2.04446689147979,-1.,-0.750444657875576));
#32967=CARTESIAN_POINT('Ctrl Pts',(2.04446689147979,1.,-0.750444657875576));
#32968=CARTESIAN_POINT('Ctrl Pts',(2.03814160092099,-1.,-0.751562963361115));
#32969=CARTESIAN_POINT('Ctrl Pts',(2.03814160092099,1.,-0.751562963361115));
#32970=CARTESIAN_POINT('Ctrl Pts',(2.03182068456221,-1.,-0.752642180487211));
#32971=CARTESIAN_POINT('Ctrl Pts',(2.03182068456221,1.,-0.752642180487211));
#32972=CARTESIAN_POINT('Ctrl Pts',(2.02550428623313,-1.,-0.753682061112768));
#32973=CARTESIAN_POINT('Ctrl Pts',(2.02550428623313,1.,-0.753682061112768));
#32974=CARTESIAN_POINT('Ctrl Pts',(2.01919259405809,-1.,-0.754682330722816));
#32975=CARTESIAN_POINT('Ctrl Pts',(2.01919259405809,1.,-0.754682330722816));
#32976=CARTESIAN_POINT('Ctrl Pts',(2.01288584328084,-1.,-0.755642704957865));
#32977=CARTESIAN_POINT('Ctrl Pts',(2.01288584328084,1.,-0.755642704957865));
#32978=CARTESIAN_POINT('Ctrl Pts',(2.0065843158773,-1.,-0.756562904646671));
#32979=CARTESIAN_POINT('Ctrl Pts',(2.0065843158773,1.,-0.756562904646671));
#32980=CARTESIAN_POINT('Ctrl Pts',(2.00028834739178,-1.,-0.757442676862724));
#32981=CARTESIAN_POINT('Ctrl Pts',(2.00028834739178,1.,-0.757442676862724));
#32982=CARTESIAN_POINT('Ctrl Pts',(1.99399831098817,-1.,-0.758281796766761));
#32983=CARTESIAN_POINT('Ctrl Pts',(1.99399831098817,1.,-0.758281796766761));
#32984=CARTESIAN_POINT('Ctrl Pts',(1.98771456680874,-1.,-0.759080037802488));
#32985=CARTESIAN_POINT('Ctrl Pts',(1.98771456680874,1.,-0.759080037802488));
#32986=CARTESIAN_POINT('Ctrl Pts',(1.98143741418172,-1.,-0.75983714745219));
#32987=CARTESIAN_POINT('Ctrl Pts',(1.98143741418172,1.,-0.75983714745219));
#32988=CARTESIAN_POINT('Ctrl Pts',(1.97516705321494,-1.,-0.760552825409757));
#32989=CARTESIAN_POINT('Ctrl Pts',(1.97516705321494,1.,-0.760552825409757));
#32990=CARTESIAN_POINT('Ctrl Pts',(1.96890351582499,-1.,-0.761226690483821));
#32991=CARTESIAN_POINT('Ctrl Pts',(1.96890351582499,1.,-0.761226690483821));
#32992=CARTESIAN_POINT('Ctrl Pts',(1.96264672744186,-1.,-0.761858300014424));
#32993=CARTESIAN_POINT('Ctrl Pts',(1.96264672744186,1.,-0.761858300014424));
#32994=CARTESIAN_POINT('Ctrl Pts',(1.95639665309869,-1.,-0.762447203806179));
#32995=CARTESIAN_POINT('Ctrl Pts',(1.95639665309869,1.,-0.762447203806179));
#32996=CARTESIAN_POINT('Ctrl Pts',(1.95015342590024,-1.,-0.762992990878769));
#32997=CARTESIAN_POINT('Ctrl Pts',(1.95015342590024,1.,-0.762992990878769));
#32998=CARTESIAN_POINT('Ctrl Pts',(1.9439174661764,-1.,-0.763495333538629));
#32999=CARTESIAN_POINT('Ctrl Pts',(1.9439174661764,1.,-0.763495333538629));
#33000=CARTESIAN_POINT('Ctrl Pts',(1.93768964875886,-1.,-0.763954049121459));
#33001=CARTESIAN_POINT('Ctrl Pts',(1.93768964875886,1.,-0.763954049121459));
#33002=CARTESIAN_POINT('Ctrl Pts',(1.93147105496382,-1.,-0.764369010673941));
#33003=CARTESIAN_POINT('Ctrl Pts',(1.93147105496382,1.,-0.764369010673941));
#33004=CARTESIAN_POINT('Ctrl Pts',(1.92526263537048,-1.,-0.764740025488212));
#33005=CARTESIAN_POINT('Ctrl Pts',(1.92526263537048,1.,-0.764740025488212));
#33006=CARTESIAN_POINT('Ctrl Pts',(1.91906491634196,-1.,-0.765066729667089));
#33007=CARTESIAN_POINT('Ctrl Pts',(1.91906491634196,1.,-0.765066729667089));
#33008=CARTESIAN_POINT('Ctrl Pts',(1.91287765805169,-1.,-0.765348465884722));
#33009=CARTESIAN_POINT('Ctrl Pts',(1.91287765805169,1.,-0.765348465884722));
#33010=CARTESIAN_POINT('Ctrl Pts',(1.90669961402356,-1.,-0.765584196937919));
#33011=CARTESIAN_POINT('Ctrl Pts',(1.90669961402356,1.,-0.765584196937919));
#33012=CARTESIAN_POINT('Ctrl Pts',(1.90052930393596,-1.,-0.765772772593386));
#33013=CARTESIAN_POINT('Ctrl Pts',(1.90052930393596,1.,-0.765772772593386));
#33014=CARTESIAN_POINT('Ctrl Pts',(1.89436577771388,-1.,-0.765913193856978));
#33015=CARTESIAN_POINT('Ctrl Pts',(1.89436577771388,1.,-0.765913193856978));
#33016=CARTESIAN_POINT('Ctrl Pts',(1.88820926433409,-1.,-0.766004837062091));
#33017=CARTESIAN_POINT('Ctrl Pts',(1.88820926433409,1.,-0.766004837062091));
#33018=CARTESIAN_POINT('Ctrl Pts',(1.88206215302561,-1.,-0.766047794851865));
#33019=CARTESIAN_POINT('Ctrl Pts',(1.88206215302561,1.,-0.766047794851865));
#33020=CARTESIAN_POINT('Ctrl Pts',(1.87592888967883,-1.,-0.766042837036744));
#33021=CARTESIAN_POINT('Ctrl Pts',(1.87592888967883,1.,-0.766042837036744));
#33022=CARTESIAN_POINT('Ctrl Pts',(1.86981398314341,-1.,-0.765990708546091));
#33023=CARTESIAN_POINT('Ctrl Pts',(1.86981398314341,1.,-0.765990708546091));
#33024=CARTESIAN_POINT('Ctrl Pts',(1.86372027063312,-1.,-0.765891519092547));
#33025=CARTESIAN_POINT('Ctrl Pts',(1.86372027063312,1.,-0.765891519092547));
#33026=CARTESIAN_POINT('Ctrl Pts',(1.85764741390394,-1.,-0.765744212909319));
#33027=CARTESIAN_POINT('Ctrl Pts',(1.85764741390394,1.,-0.765744212909319));
#33028=CARTESIAN_POINT('Ctrl Pts',(1.85158945130063,-1.,-0.765545710619063));
#33029=CARTESIAN_POINT('Ctrl Pts',(1.85158945130063,1.,-0.765545710619063));
#33030=CARTESIAN_POINT('Ctrl Pts',(1.84553698875924,-1.,-0.765291664862029));
#33031=CARTESIAN_POINT('Ctrl Pts',(1.84553698875924,1.,-0.765291664862029));
#33032=CARTESIAN_POINT('Ctrl Pts',(1.83948181064835,-1.,-0.764978057881738));
#33033=CARTESIAN_POINT('Ctrl Pts',(1.83948181064835,1.,-0.764978057881738));
#33034=CARTESIAN_POINT('Ctrl Pts',(1.83342077227142,-1.,-0.764602549687853));
#33035=CARTESIAN_POINT('Ctrl Pts',(1.83342077227142,1.,-0.764602549687853));
#33036=CARTESIAN_POINT('Ctrl Pts',(1.82735991200065,-1.,-0.764165902605995));
#33037=CARTESIAN_POINT('Ctrl Pts',(1.82735991200065,1.,-0.764165902605995));
#33038=CARTESIAN_POINT('Ctrl Pts',(1.82131873145266,-1.,-0.763673465462727));
#33039=CARTESIAN_POINT('Ctrl Pts',(1.82131873145266,1.,-0.763673465462727));
#33040=CARTESIAN_POINT('Ctrl Pts',(1.8153211840553,-1.,-0.763132003836634));
#33041=CARTESIAN_POINT('Ctrl Pts',(1.8153211840553,1.,-0.763132003836634));
#33042=CARTESIAN_POINT('Ctrl Pts',(1.80938551463965,-1.,-0.762546129463938));
#33043=CARTESIAN_POINT('Ctrl Pts',(1.80938551463965,1.,-0.762546129463938));
#33044=CARTESIAN_POINT('Ctrl Pts',(1.80351583877342,-1.,-0.761915336443547));
#33045=CARTESIAN_POINT('Ctrl Pts',(1.80351583877342,1.,-0.761915336443547));
#33046=CARTESIAN_POINT('Ctrl Pts',(1.79768986997783,-1.,-0.761229695230558));
#33047=CARTESIAN_POINT('Ctrl Pts',(1.79768986997783,1.,-0.761229695230558));
#33048=CARTESIAN_POINT('Ctrl Pts',(1.7918581561088,-1.,-0.760469555880749));
#33049=CARTESIAN_POINT('Ctrl Pts',(1.7918581561088,1.,-0.760469555880749));
#33050=CARTESIAN_POINT('Ctrl Pts',(1.78596964884604,-1.,-0.75961440111019));
#33051=CARTESIAN_POINT('Ctrl Pts',(1.78596964884604,1.,-0.75961440111019));
#33052=CARTESIAN_POINT('Ctrl Pts',(1.77999411220945,-1.,-0.758650626677519));
#33053=CARTESIAN_POINT('Ctrl Pts',(1.77999411220945,1.,-0.758650626677519));
#33054=CARTESIAN_POINT('Ctrl Pts',(1.77394167108292,-1.,-0.757578264077029));
#33055=CARTESIAN_POINT('Ctrl Pts',(1.77394167108292,1.,-0.757578264077029));
#33056=CARTESIAN_POINT('Ctrl Pts',(1.76789396002998,-1.,-0.75642189602781));
#33057=CARTESIAN_POINT('Ctrl Pts',(1.76789396002998,1.,-0.75642189602781));
#33058=CARTESIAN_POINT('Ctrl Pts',(1.76197817240128,-1.,-0.755220979974462));
#33059=CARTESIAN_POINT('Ctrl Pts',(1.76197817240128,1.,-0.755220979974462));
#33060=CARTESIAN_POINT('Ctrl Pts',(1.75631083600019,-1.,-0.754009254027829));
#33061=CARTESIAN_POINT('Ctrl Pts',(1.75631083600019,1.,-0.754009254027829));
#33062=CARTESIAN_POINT('Ctrl Pts',(1.75095139468794,-1.,-0.752797683531314));
#33063=CARTESIAN_POINT('Ctrl Pts',(1.75095139468794,1.,-0.752797683531314));
#33064=CARTESIAN_POINT('Ctrl Pts',(1.74585086852502,-1.,-0.751555614164483));
#33065=CARTESIAN_POINT('Ctrl Pts',(1.74585086852502,1.,-0.751555614164483));
#33066=CARTESIAN_POINT('Ctrl Pts',(1.74080458267114,-1.,-0.75019343598125));
#33067=CARTESIAN_POINT('Ctrl Pts',(1.74080458267114,1.,-0.75019343598125));
#33068=CARTESIAN_POINT('Ctrl Pts',(1.7355035168033,-1.,-0.74858246295687));
#33069=CARTESIAN_POINT('Ctrl Pts',(1.7355035168033,1.,-0.74858246295687));
#33070=CARTESIAN_POINT('Ctrl Pts',(1.72958533647714,-1.,-0.746574710097752));
#33071=CARTESIAN_POINT('Ctrl Pts',(1.72958533647714,1.,-0.746574710097752));
#33072=CARTESIAN_POINT('Ctrl Pts',(1.72268229916769,-1.,-0.744021445433094));
#33073=CARTESIAN_POINT('Ctrl Pts',(1.72268229916769,1.,-0.744021445433094));
#33074=CARTESIAN_POINT('Ctrl Pts',(1.71447789751001,-1.,-0.74079516202821));
#33075=CARTESIAN_POINT('Ctrl Pts',(1.71447789751001,1.,-0.74079516202821));
#33076=CARTESIAN_POINT('Ctrl Pts',(1.70473309004249,-1.,-0.736799665716932));
#33077=CARTESIAN_POINT('Ctrl Pts',(1.70473309004249,1.,-0.736799665716932));
#33078=CARTESIAN_POINT('Ctrl Pts',(1.69326921972915,-1.,-0.731963238685357));
#33079=CARTESIAN_POINT('Ctrl Pts',(1.69326921972915,1.,-0.731963238685357));
#33080=CARTESIAN_POINT('Ctrl Pts',(1.67996158451922,-1.,-0.726235967982445));
#33081=CARTESIAN_POINT('Ctrl Pts',(1.67996158451922,1.,-0.726235967982445));
#33082=CARTESIAN_POINT('Ctrl Pts',(1.66472880551777,-1.,-0.71958543378795));
#33083=CARTESIAN_POINT('Ctrl Pts',(1.66472880551777,1.,-0.71958543378795));
#33084=CARTESIAN_POINT('Ctrl Pts',(1.64752408828442,-1.,-0.711993139340448));
#33085=CARTESIAN_POINT('Ctrl Pts',(1.64752408828442,1.,-0.711993139340448));
#33086=CARTESIAN_POINT('Ctrl Pts',(1.6321654166204,-1.,-0.705159151977294));
#33087=CARTESIAN_POINT('Ctrl Pts',(1.6321654166204,1.,-0.705159151977294));
#33088=CARTESIAN_POINT('Ctrl Pts',(1.61974673471117,-1.,-0.699605146398837));
#33089=CARTESIAN_POINT('Ctrl Pts',(1.61974673471117,1.,-0.699605146398837));
#33090=CARTESIAN_POINT('Ctrl Pts',(1.61106790957619,-1.,-0.69571209787897));
#33091=CARTESIAN_POINT('Ctrl Pts',(1.61106790957619,1.,-0.69571209787897));
#33092=CARTESIAN_POINT('Ctrl Pts',(1.60662857109684,-1.,-0.693717979106306));
#33093=CARTESIAN_POINT('Ctrl Pts',(1.60662857109684,1.,-0.693717979106306));
#33094=CARTESIAN_POINT('',(2.0698113262342,1.,-0.745574324794401));
#33095=CARTESIAN_POINT('Ctrl Pts',(2.0698113262342,1.,-0.745574324794401));
#33096=CARTESIAN_POINT('Ctrl Pts',(2.06854248895728,1.,-0.745832791378367));
#33097=CARTESIAN_POINT('Ctrl Pts',(2.06600523016815,1.,-0.746345871544201));
#33098=CARTESIAN_POINT('Ctrl Pts',(2.06220058927826,1.,-0.74710393278792));
#33099=CARTESIAN_POINT('Ctrl Pts',(2.05713023031006,1.,-0.748091554183803));
#33100=CARTESIAN_POINT('Ctrl Pts',(2.05079645592154,1.,-0.749287468665046));
#33101=CARTESIAN_POINT('Ctrl Pts',(2.04446689147979,1.,-0.750444657875576));
#33102=CARTESIAN_POINT('Ctrl Pts',(2.03814160092099,1.,-0.751562963361115));
#33103=CARTESIAN_POINT('Ctrl Pts',(2.03182068456221,1.,-0.752642180487211));
#33104=CARTESIAN_POINT('Ctrl Pts',(2.02550428623313,1.,-0.753682061112768));
#33105=CARTESIAN_POINT('Ctrl Pts',(2.01919259405809,1.,-0.754682330722816));
#33106=CARTESIAN_POINT('Ctrl Pts',(2.01288584328084,1.,-0.755642704957865));
#33107=CARTESIAN_POINT('Ctrl Pts',(2.0065843158773,1.,-0.756562904646671));
#33108=CARTESIAN_POINT('Ctrl Pts',(2.00028834739178,1.,-0.757442676862724));
#33109=CARTESIAN_POINT('Ctrl Pts',(1.99399831098817,1.,-0.758281796766761));
#33110=CARTESIAN_POINT('Ctrl Pts',(1.98771456680874,1.,-0.759080037802488));
#33111=CARTESIAN_POINT('Ctrl Pts',(1.98143741418172,1.,-0.75983714745219));
#33112=CARTESIAN_POINT('Ctrl Pts',(1.97516705321494,1.,-0.760552825409757));
#33113=CARTESIAN_POINT('Ctrl Pts',(1.96890351582499,1.,-0.761226690483821));
#33114=CARTESIAN_POINT('Ctrl Pts',(1.96264672744186,1.,-0.761858300014424));
#33115=CARTESIAN_POINT('Ctrl Pts',(1.95639665309869,1.,-0.762447203806179));
#33116=CARTESIAN_POINT('Ctrl Pts',(1.95015342590024,1.,-0.762992990878769));
#33117=CARTESIAN_POINT('Ctrl Pts',(1.9439174661764,1.,-0.763495333538629));
#33118=CARTESIAN_POINT('Ctrl Pts',(1.93768964875886,1.,-0.763954049121459));
#33119=CARTESIAN_POINT('Ctrl Pts',(1.93147105496382,1.,-0.764369010673941));
#33120=CARTESIAN_POINT('Ctrl Pts',(1.92526263537048,1.,-0.764740025488212));
#33121=CARTESIAN_POINT('Ctrl Pts',(1.91906491634196,1.,-0.765066729667089));
#33122=CARTESIAN_POINT('Ctrl Pts',(1.91287765805169,1.,-0.765348465884722));
#33123=CARTESIAN_POINT('Ctrl Pts',(1.90669961402356,1.,-0.765584196937919));
#33124=CARTESIAN_POINT('Ctrl Pts',(1.90052930393596,1.,-0.765772772593386));
#33125=CARTESIAN_POINT('Ctrl Pts',(1.89436577771388,1.,-0.765913193856978));
#33126=CARTESIAN_POINT('Ctrl Pts',(1.88820926433409,1.,-0.766004837062091));
#33127=CARTESIAN_POINT('Ctrl Pts',(1.88206215302561,1.,-0.766047794851865));
#33128=CARTESIAN_POINT('Ctrl Pts',(1.87592888967883,1.,-0.766042837036744));
#33129=CARTESIAN_POINT('Ctrl Pts',(1.86981398314341,1.,-0.765990708546091));
#33130=CARTESIAN_POINT('Ctrl Pts',(1.86372027063312,1.,-0.765891519092547));
#33131=CARTESIAN_POINT('Ctrl Pts',(1.85764741390394,1.,-0.765744212909319));
#33132=CARTESIAN_POINT('Ctrl Pts',(1.85158945130063,1.,-0.765545710619063));
#33133=CARTESIAN_POINT('Ctrl Pts',(1.84553698875924,1.,-0.765291664862029));
#33134=CARTESIAN_POINT('Ctrl Pts',(1.83948181064835,1.,-0.764978057881738));
#33135=CARTESIAN_POINT('Ctrl Pts',(1.83342077227142,1.,-0.764602549687853));
#33136=CARTESIAN_POINT('Ctrl Pts',(1.82735991200065,1.,-0.764165902605995));
#33137=CARTESIAN_POINT('Ctrl Pts',(1.82131873145266,1.,-0.763673465462727));
#33138=CARTESIAN_POINT('Ctrl Pts',(1.8153211840553,1.,-0.763132003836634));
#33139=CARTESIAN_POINT('Ctrl Pts',(1.80938551463965,1.,-0.762546129463938));
#33140=CARTESIAN_POINT('Ctrl Pts',(1.80351583877342,1.,-0.761915336443547));
#33141=CARTESIAN_POINT('Ctrl Pts',(1.79768986997783,1.,-0.761229695230558));
#33142=CARTESIAN_POINT('Ctrl Pts',(1.7918581561088,1.,-0.760469555880749));
#33143=CARTESIAN_POINT('Ctrl Pts',(1.78596964884604,1.,-0.75961440111019));
#33144=CARTESIAN_POINT('Ctrl Pts',(1.77999411220945,1.,-0.758650626677519));
#33145=CARTESIAN_POINT('Ctrl Pts',(1.77394167108292,1.,-0.757578264077029));
#33146=CARTESIAN_POINT('Ctrl Pts',(1.76789396002998,1.,-0.75642189602781));
#33147=CARTESIAN_POINT('Ctrl Pts',(1.76197817240128,1.,-0.755220979974462));
#33148=CARTESIAN_POINT('Ctrl Pts',(1.75631083600019,1.,-0.754009254027829));
#33149=CARTESIAN_POINT('Ctrl Pts',(1.75095139468794,1.,-0.752797683531314));
#33150=CARTESIAN_POINT('Ctrl Pts',(1.74585086852502,1.,-0.751555614164483));
#33151=CARTESIAN_POINT('Ctrl Pts',(1.74080458267114,1.,-0.75019343598125));
#33152=CARTESIAN_POINT('Ctrl Pts',(1.7355035168033,1.,-0.74858246295687));
#33153=CARTESIAN_POINT('Ctrl Pts',(1.72958533647714,1.,-0.746574710097752));
#33154=CARTESIAN_POINT('Ctrl Pts',(1.72268229916769,1.,-0.744021445433094));
#33155=CARTESIAN_POINT('Ctrl Pts',(1.71447789751001,1.,-0.74079516202821));
#33156=CARTESIAN_POINT('Ctrl Pts',(1.70473309004249,1.,-0.736799665716932));
#33157=CARTESIAN_POINT('Ctrl Pts',(1.69326921972915,1.,-0.731963238685357));
#33158=CARTESIAN_POINT('Ctrl Pts',(1.67996158451922,1.,-0.726235967982445));
#33159=CARTESIAN_POINT('Ctrl Pts',(1.66472880551777,1.,-0.71958543378795));
#33160=CARTESIAN_POINT('Ctrl Pts',(1.64752408828442,1.,-0.711993139340448));
#33161=CARTESIAN_POINT('Ctrl Pts',(1.6321654166204,1.,-0.705159151977294));
#33162=CARTESIAN_POINT('Ctrl Pts',(1.61974673471117,1.,-0.699605146398837));
#33163=CARTESIAN_POINT('Ctrl Pts',(1.61106790957619,1.,-0.69571209787897));
#33164=CARTESIAN_POINT('Ctrl Pts',(1.60662857109684,1.,-0.693717979106306));
#33165=CARTESIAN_POINT('',(2.0698113262342,0.,-0.745574324794401));
#33166=CARTESIAN_POINT('Origin',(2.11275013067528,0.,-0.61342227326009));
#33167=CARTESIAN_POINT('',(2.11275013067528,1.,-0.61342227326009));
#33168=CARTESIAN_POINT('',(2.0698113262342,1.,-0.745574324794401));
#33169=CARTESIAN_POINT('',(2.11275013067528,0.,-0.61342227326009));
#33170=CARTESIAN_POINT('Ctrl Pts',(1.7075470150345,-1.,-0.383122945602004));
#33171=CARTESIAN_POINT('Ctrl Pts',(1.7075470150345,1.,-0.383122945602004));
#33172=CARTESIAN_POINT('Ctrl Pts',(1.71231062891958,-1.,-0.384119047315542));
#33173=CARTESIAN_POINT('Ctrl Pts',(1.71231062891958,1.,-0.384119047315542));
#33174=CARTESIAN_POINT('Ctrl Pts',(1.72162022246158,-1.,-0.38607079032701));
#33175=CARTESIAN_POINT('Ctrl Pts',(1.72162022246158,1.,-0.38607079032701));
#33176=CARTESIAN_POINT('Ctrl Pts',(1.7349317097561,-1.,-0.388877023509192));
#33177=CARTESIAN_POINT('Ctrl Pts',(1.7349317097561,1.,-0.388877023509192));
#33178=CARTESIAN_POINT('Ctrl Pts',(1.75137405313962,-1.,-0.392375812294307));
#33179=CARTESIAN_POINT('Ctrl Pts',(1.75137405313962,1.,-0.392375812294307));
#33180=CARTESIAN_POINT('Ctrl Pts',(1.7697556004756,-1.,-0.39634619612042));
#33181=CARTESIAN_POINT('Ctrl Pts',(1.7697556004756,1.,-0.39634619612042));
#33182=CARTESIAN_POINT('Ctrl Pts',(1.78598826347533,-1.,-0.399919403783081));
#33183=CARTESIAN_POINT('Ctrl Pts',(1.78598826347533,1.,-0.399919403783081));
#33184=CARTESIAN_POINT('Ctrl Pts',(1.80012077176221,-1.,-0.403107976170441));
#33185=CARTESIAN_POINT('Ctrl Pts',(1.80012077176221,1.,-0.403107976170441));
#33186=CARTESIAN_POINT('Ctrl Pts',(1.81223801813988,-1.,-0.405933518411838));
#33187=CARTESIAN_POINT('Ctrl Pts',(1.81223801813988,1.,-0.405933518411838));
#33188=CARTESIAN_POINT('Ctrl Pts',(1.8224702267854,-1.,-0.408428948108534));
#33189=CARTESIAN_POINT('Ctrl Pts',(1.8224702267854,1.,-0.408428948108534));
#33190=CARTESIAN_POINT('Ctrl Pts',(1.83100408895216,-1.,-0.410641256301675));
#33191=CARTESIAN_POINT('Ctrl Pts',(1.83100408895216,1.,-0.410641256301675));
#33192=CARTESIAN_POINT('Ctrl Pts',(1.83808953475839,-1.,-0.412633125322162));
#33193=CARTESIAN_POINT('Ctrl Pts',(1.83808953475839,1.,-0.412633125322162));
#33194=CARTESIAN_POINT('Ctrl Pts',(1.8440575707371,-1.,-0.41448743825434));
#33195=CARTESIAN_POINT('Ctrl Pts',(1.8440575707371,1.,-0.41448743825434));
#33196=CARTESIAN_POINT('Ctrl Pts',(1.84929312929882,-1.,-0.416300022038864));
#33197=CARTESIAN_POINT('Ctrl Pts',(1.84929312929882,1.,-0.416300022038864));
#33198=CARTESIAN_POINT('Ctrl Pts',(1.85417632856234,-1.,-0.418164129143534));
#33199=CARTESIAN_POINT('Ctrl Pts',(1.85417632856234,1.,-0.418164129143534));
#33200=CARTESIAN_POINT('Ctrl Pts',(1.85903281096686,-1.,-0.42015728797562));
#33201=CARTESIAN_POINT('Ctrl Pts',(1.85903281096686,1.,-0.42015728797562));
#33202=CARTESIAN_POINT('Ctrl Pts',(1.86408083334028,-1.,-0.422327307418275));
#33203=CARTESIAN_POINT('Ctrl Pts',(1.86408083334028,1.,-0.422327307418275));
#33204=CARTESIAN_POINT('Ctrl Pts',(1.86937803944323,-1.,-0.424678177291359));
#33205=CARTESIAN_POINT('Ctrl Pts',(1.86937803944323,1.,-0.424678177291359));
#33206=CARTESIAN_POINT('Ctrl Pts',(1.87486989291484,-1.,-0.427183828519102));
#33207=CARTESIAN_POINT('Ctrl Pts',(1.87486989291484,1.,-0.427183828519102));
#33208=CARTESIAN_POINT('Ctrl Pts',(1.88044229001832,-1.,-0.429803062482345));
#33209=CARTESIAN_POINT('Ctrl Pts',(1.88044229001832,1.,-0.429803062482345));
#33210=CARTESIAN_POINT('Ctrl Pts',(1.88596913666793,-1.,-0.432493038548748));
#33211=CARTESIAN_POINT('Ctrl Pts',(1.88596913666793,1.,-0.432493038548748));
#33212=CARTESIAN_POINT('Ctrl Pts',(1.89136993975504,-1.,-0.435225660963383));
#33213=CARTESIAN_POINT('Ctrl Pts',(1.89136993975504,1.,-0.435225660963383));
#33214=CARTESIAN_POINT('Ctrl Pts',(1.89663648956466,-1.,-0.437995003948244));
#33215=CARTESIAN_POINT('Ctrl Pts',(1.89663648956466,1.,-0.437995003948244));
#33216=CARTESIAN_POINT('Ctrl Pts',(1.90180124389086,-1.,-0.440807833704038));
#33217=CARTESIAN_POINT('Ctrl Pts',(1.90180124389086,1.,-0.440807833704038));
#33218=CARTESIAN_POINT('Ctrl Pts',(1.90691756144898,-1.,-0.443677556849151));
#33219=CARTESIAN_POINT('Ctrl Pts',(1.90691756144898,1.,-0.443677556849151));
#33220=CARTESIAN_POINT('Ctrl Pts',(1.9120369998112,-1.,-0.446617343485711));
#33221=CARTESIAN_POINT('Ctrl Pts',(1.9120369998112,1.,-0.446617343485711));
#33222=CARTESIAN_POINT('Ctrl Pts',(1.91718342555755,-1.,-0.449632260106662));
#33223=CARTESIAN_POINT('Ctrl Pts',(1.91718342555755,1.,-0.449632260106662));
#33224=CARTESIAN_POINT('Ctrl Pts',(1.92235380648502,-1.,-0.452719478359433));
#33225=CARTESIAN_POINT('Ctrl Pts',(1.92235380648502,1.,-0.452719478359433));
#33226=CARTESIAN_POINT('Ctrl Pts',(1.92753067150476,-1.,-0.455872005174371));
#33227=CARTESIAN_POINT('Ctrl Pts',(1.92753067150476,1.,-0.455872005174371));
#33228=CARTESIAN_POINT('Ctrl Pts',(1.93269066517934,-1.,-0.459081234547926));
#33229=CARTESIAN_POINT('Ctrl Pts',(1.93269066517934,1.,-0.459081234547926));
#33230=CARTESIAN_POINT('Ctrl Pts',(1.93781486640821,-1.,-0.462340031009057));
#33231=CARTESIAN_POINT('Ctrl Pts',(1.93781486640821,1.,-0.462340031009057));
#33232=CARTESIAN_POINT('Ctrl Pts',(1.9428979419619,-1.,-0.46564546202603));
#33233=CARTESIAN_POINT('Ctrl Pts',(1.9428979419619,1.,-0.46564546202603));
#33234=CARTESIAN_POINT('Ctrl Pts',(1.94794381136514,-1.,-0.468997482913135));
#33235=CARTESIAN_POINT('Ctrl Pts',(1.94794381136514,1.,-0.468997482913135));
#33236=CARTESIAN_POINT('Ctrl Pts',(1.95296148278133,-1.,-0.472397672264072));
#33237=CARTESIAN_POINT('Ctrl Pts',(1.95296148278133,1.,-0.472397672264072));
#33238=CARTESIAN_POINT('Ctrl Pts',(1.95796111148177,-1.,-0.475848034683176));
#33239=CARTESIAN_POINT('Ctrl Pts',(1.95796111148177,1.,-0.475848034683176));
#33240=CARTESIAN_POINT('Ctrl Pts',(1.96294933055943,-1.,-0.479349583074855));
#33241=CARTESIAN_POINT('Ctrl Pts',(1.96294933055943,1.,-0.479349583074855));
#33242=CARTESIAN_POINT('Ctrl Pts',(1.96792703422362,-1.,-0.482901662120691));
#33243=CARTESIAN_POINT('Ctrl Pts',(1.96792703422362,1.,-0.482901662120691));
#33244=CARTESIAN_POINT('Ctrl Pts',(1.97289186263272,-1.,-0.486502692907659));
#33245=CARTESIAN_POINT('Ctrl Pts',(1.97289186263272,1.,-0.486502692907659));
#33246=CARTESIAN_POINT('Ctrl Pts',(1.97783973019229,-1.,-0.490150627860953));
#33247=CARTESIAN_POINT('Ctrl Pts',(1.97783973019229,1.,-0.490150627860953));
#33248=CARTESIAN_POINT('Ctrl Pts',(1.98276658761821,-1.,-0.493843476541495));
#33249=CARTESIAN_POINT('Ctrl Pts',(1.98276658761821,1.,-0.493843476541495));
#33250=CARTESIAN_POINT('Ctrl Pts',(1.98767044752932,-1.,-0.497579909545574));
#33251=CARTESIAN_POINT('Ctrl Pts',(1.98767044752932,1.,-0.497579909545574));
#33252=CARTESIAN_POINT('Ctrl Pts',(1.99255149126155,-1.,-0.501359287727146));
#33253=CARTESIAN_POINT('Ctrl Pts',(1.99255149126155,1.,-0.501359287727146));
#33254=CARTESIAN_POINT('Ctrl Pts',(1.99741107463572,-1.,-0.505181361323026));
#33255=CARTESIAN_POINT('Ctrl Pts',(1.99741107463572,1.,-0.505181361323026));
#33256=CARTESIAN_POINT('Ctrl Pts',(2.00225107134734,-1.,-0.509046069886157));
#33257=CARTESIAN_POINT('Ctrl Pts',(2.00225107134734,1.,-0.509046069886157));
#33258=CARTESIAN_POINT('Ctrl Pts',(2.00707309946949,-1.,-0.512953306961793));
#33259=CARTESIAN_POINT('Ctrl Pts',(2.00707309946949,1.,-0.512953306961793));
#33260=CARTESIAN_POINT('Ctrl Pts',(2.01187773939242,-1.,-0.516902681728687));
#33261=CARTESIAN_POINT('Ctrl Pts',(2.01187773939242,1.,-0.516902681728687));
#33262=CARTESIAN_POINT('Ctrl Pts',(2.01666477917286,-1.,-0.520893590399371));
#33263=CARTESIAN_POINT('Ctrl Pts',(2.01666477917286,1.,-0.520893590399371));
#33264=CARTESIAN_POINT('Ctrl Pts',(2.02143356304698,-1.,-0.524925318333476));
#33265=CARTESIAN_POINT('Ctrl Pts',(2.02143356304698,1.,-0.524925318333476));
#33266=CARTESIAN_POINT('Ctrl Pts',(2.0261832908329,-1.,-0.528997127241914));
#33267=CARTESIAN_POINT('Ctrl Pts',(2.0261832908329,1.,-0.528997127241914));
#33268=CARTESIAN_POINT('Ctrl Pts',(2.03091336214426,-1.,-0.533108355132977));
#33269=CARTESIAN_POINT('Ctrl Pts',(2.03091336214426,1.,-0.533108355132977));
#33270=CARTESIAN_POINT('Ctrl Pts',(2.03562362954037,-1.,-0.537258489833262));
#33271=CARTESIAN_POINT('Ctrl Pts',(2.03562362954037,1.,-0.537258489833262));
#33272=CARTESIAN_POINT('Ctrl Pts',(2.04031422690527,-1.,-0.541447120615659));
#33273=CARTESIAN_POINT('Ctrl Pts',(2.04031422690527,1.,-0.541447120615659));
#33274=CARTESIAN_POINT('Ctrl Pts',(2.04498544714588,-1.,-0.54567390381743));
#33275=CARTESIAN_POINT('Ctrl Pts',(2.04498544714588,1.,-0.54567390381743));
#33276=CARTESIAN_POINT('Ctrl Pts',(2.04963761077958,-1.,-0.549938525150295));
#33277=CARTESIAN_POINT('Ctrl Pts',(2.04963761077958,1.,-0.549938525150295));
#33278=CARTESIAN_POINT('Ctrl Pts',(2.05427091604413,-1.,-0.554240657463906));
#33279=CARTESIAN_POINT('Ctrl Pts',(2.05427091604413,1.,-0.554240657463906));
#33280=CARTESIAN_POINT('Ctrl Pts',(2.05888537756462,-1.,-0.558579940185152));
#33281=CARTESIAN_POINT('Ctrl Pts',(2.05888537756462,1.,-0.558579940185152));
#33282=CARTESIAN_POINT('Ctrl Pts',(2.06348090160589,-1.,-0.562955993082262));
#33283=CARTESIAN_POINT('Ctrl Pts',(2.06348090160589,1.,-0.562955993082262));
#33284=CARTESIAN_POINT('Ctrl Pts',(2.06805732997334,-1.,-0.567368421181087));
#33285=CARTESIAN_POINT('Ctrl Pts',(2.06805732997334,1.,-0.567368421181087));
#33286=CARTESIAN_POINT('Ctrl Pts',(2.07261449292824,-1.,-0.571816823242603));
#33287=CARTESIAN_POINT('Ctrl Pts',(2.07261449292824,1.,-0.571816823242603));
#33288=CARTESIAN_POINT('Ctrl Pts',(2.07715226767559,-1.,-0.576300797416845));
#33289=CARTESIAN_POINT('Ctrl Pts',(2.07715226767559,1.,-0.576300797416845));
#33290=CARTESIAN_POINT('Ctrl Pts',(2.08167059018418,-1.,-0.580819952108064));
#33291=CARTESIAN_POINT('Ctrl Pts',(2.08167059018418,1.,-0.580819952108064));
#33292=CARTESIAN_POINT('Ctrl Pts',(2.08616943727951,-1.,-0.585373918991617));
#33293=CARTESIAN_POINT('Ctrl Pts',(2.08616943727951,1.,-0.585373918991617));
#33294=CARTESIAN_POINT('Ctrl Pts',(2.09064881812129,-1.,-0.589962365403406));
#33295=CARTESIAN_POINT('Ctrl Pts',(2.09064881812129,1.,-0.589962365403406));
#33296=CARTESIAN_POINT('Ctrl Pts',(2.0951087622027,-1.,-0.594585006052162));
#33297=CARTESIAN_POINT('Ctrl Pts',(2.0951087622027,1.,-0.594585006052162));
#33298=CARTESIAN_POINT('Ctrl Pts',(2.0995493086477,-1.,-0.599241616420534));
#33299=CARTESIAN_POINT('Ctrl Pts',(2.0995493086477,1.,-0.599241616420534));
#33300=CARTESIAN_POINT('Ctrl Pts',(2.10397049886949,-1.,-0.60393203073603));
#33301=CARTESIAN_POINT('Ctrl Pts',(2.10397049886949,1.,-0.60393203073603));
#33302=CARTESIAN_POINT('Ctrl Pts',(2.1074919961518,-1.,-0.607711315454876));
#33303=CARTESIAN_POINT('Ctrl Pts',(2.1074919961518,1.,-0.607711315454876));
#33304=CARTESIAN_POINT('Ctrl Pts',(2.11012443807238,-1.,-0.610560911689899));
#33305=CARTESIAN_POINT('Ctrl Pts',(2.11012443807238,1.,-0.610560911689899));
#33306=CARTESIAN_POINT('Ctrl Pts',(2.11187554259986,-1.,-0.6124673655618));
#33307=CARTESIAN_POINT('Ctrl Pts',(2.11187554259986,1.,-0.6124673655618));
#33308=CARTESIAN_POINT('Ctrl Pts',(2.11275013067528,-1.,-0.61342227326009));
#33309=CARTESIAN_POINT('Ctrl Pts',(2.11275013067528,1.,-0.61342227326009));
#33310=CARTESIAN_POINT('',(1.7075470150345,1.,-0.383122945602004));
#33311=CARTESIAN_POINT('Ctrl Pts',(1.7075470150345,1.,-0.383122945602004));
#33312=CARTESIAN_POINT('Ctrl Pts',(1.71231062891958,1.,-0.384119047315542));
#33313=CARTESIAN_POINT('Ctrl Pts',(1.72162022246158,1.,-0.38607079032701));
#33314=CARTESIAN_POINT('Ctrl Pts',(1.7349317097561,1.,-0.388877023509192));
#33315=CARTESIAN_POINT('Ctrl Pts',(1.75137405313962,1.,-0.392375812294307));
#33316=CARTESIAN_POINT('Ctrl Pts',(1.7697556004756,1.,-0.39634619612042));
#33317=CARTESIAN_POINT('Ctrl Pts',(1.78598826347533,1.,-0.399919403783081));
#33318=CARTESIAN_POINT('Ctrl Pts',(1.80012077176221,1.,-0.403107976170441));
#33319=CARTESIAN_POINT('Ctrl Pts',(1.81223801813988,1.,-0.405933518411838));
#33320=CARTESIAN_POINT('Ctrl Pts',(1.8224702267854,1.,-0.408428948108534));
#33321=CARTESIAN_POINT('Ctrl Pts',(1.83100408895216,1.,-0.410641256301675));
#33322=CARTESIAN_POINT('Ctrl Pts',(1.83808953475839,1.,-0.412633125322162));
#33323=CARTESIAN_POINT('Ctrl Pts',(1.8440575707371,1.,-0.41448743825434));
#33324=CARTESIAN_POINT('Ctrl Pts',(1.84929312929882,1.,-0.416300022038864));
#33325=CARTESIAN_POINT('Ctrl Pts',(1.85417632856234,1.,-0.418164129143534));
#33326=CARTESIAN_POINT('Ctrl Pts',(1.85903281096686,1.,-0.42015728797562));
#33327=CARTESIAN_POINT('Ctrl Pts',(1.86408083334028,1.,-0.422327307418275));
#33328=CARTESIAN_POINT('Ctrl Pts',(1.86937803944323,1.,-0.424678177291359));
#33329=CARTESIAN_POINT('Ctrl Pts',(1.87486989291484,1.,-0.427183828519102));
#33330=CARTESIAN_POINT('Ctrl Pts',(1.88044229001832,1.,-0.429803062482345));
#33331=CARTESIAN_POINT('Ctrl Pts',(1.88596913666793,1.,-0.432493038548748));
#33332=CARTESIAN_POINT('Ctrl Pts',(1.89136993975504,1.,-0.435225660963383));
#33333=CARTESIAN_POINT('Ctrl Pts',(1.89663648956466,1.,-0.437995003948244));
#33334=CARTESIAN_POINT('Ctrl Pts',(1.90180124389086,1.,-0.440807833704038));
#33335=CARTESIAN_POINT('Ctrl Pts',(1.90691756144898,1.,-0.443677556849151));
#33336=CARTESIAN_POINT('Ctrl Pts',(1.9120369998112,1.,-0.446617343485711));
#33337=CARTESIAN_POINT('Ctrl Pts',(1.91718342555755,1.,-0.449632260106662));
#33338=CARTESIAN_POINT('Ctrl Pts',(1.92235380648502,1.,-0.452719478359433));
#33339=CARTESIAN_POINT('Ctrl Pts',(1.92753067150476,1.,-0.455872005174371));
#33340=CARTESIAN_POINT('Ctrl Pts',(1.93269066517934,1.,-0.459081234547926));
#33341=CARTESIAN_POINT('Ctrl Pts',(1.93781486640821,1.,-0.462340031009057));
#33342=CARTESIAN_POINT('Ctrl Pts',(1.9428979419619,1.,-0.46564546202603));
#33343=CARTESIAN_POINT('Ctrl Pts',(1.94794381136514,1.,-0.468997482913135));
#33344=CARTESIAN_POINT('Ctrl Pts',(1.95296148278133,1.,-0.472397672264072));
#33345=CARTESIAN_POINT('Ctrl Pts',(1.95796111148177,1.,-0.475848034683176));
#33346=CARTESIAN_POINT('Ctrl Pts',(1.96294933055943,1.,-0.479349583074855));
#33347=CARTESIAN_POINT('Ctrl Pts',(1.96792703422362,1.,-0.482901662120691));
#33348=CARTESIAN_POINT('Ctrl Pts',(1.97289186263272,1.,-0.486502692907659));
#33349=CARTESIAN_POINT('Ctrl Pts',(1.97783973019229,1.,-0.490150627860953));
#33350=CARTESIAN_POINT('Ctrl Pts',(1.98276658761821,1.,-0.493843476541495));
#33351=CARTESIAN_POINT('Ctrl Pts',(1.98767044752932,1.,-0.497579909545574));
#33352=CARTESIAN_POINT('Ctrl Pts',(1.99255149126155,1.,-0.501359287727146));
#33353=CARTESIAN_POINT('Ctrl Pts',(1.99741107463572,1.,-0.505181361323026));
#33354=CARTESIAN_POINT('Ctrl Pts',(2.00225107134734,1.,-0.509046069886157));
#33355=CARTESIAN_POINT('Ctrl Pts',(2.00707309946949,1.,-0.512953306961793));
#33356=CARTESIAN_POINT('Ctrl Pts',(2.01187773939242,1.,-0.516902681728687));
#33357=CARTESIAN_POINT('Ctrl Pts',(2.01666477917286,1.,-0.520893590399371));
#33358=CARTESIAN_POINT('Ctrl Pts',(2.02143356304698,1.,-0.524925318333476));
#33359=CARTESIAN_POINT('Ctrl Pts',(2.0261832908329,1.,-0.528997127241914));
#33360=CARTESIAN_POINT('Ctrl Pts',(2.03091336214426,1.,-0.533108355132977));
#33361=CARTESIAN_POINT('Ctrl Pts',(2.03562362954037,1.,-0.537258489833262));
#33362=CARTESIAN_POINT('Ctrl Pts',(2.04031422690527,1.,-0.541447120615659));
#33363=CARTESIAN_POINT('Ctrl Pts',(2.04498544714588,1.,-0.54567390381743));
#33364=CARTESIAN_POINT('Ctrl Pts',(2.04963761077958,1.,-0.549938525150295));
#33365=CARTESIAN_POINT('Ctrl Pts',(2.05427091604413,1.,-0.554240657463906));
#33366=CARTESIAN_POINT('Ctrl Pts',(2.05888537756462,1.,-0.558579940185152));
#33367=CARTESIAN_POINT('Ctrl Pts',(2.06348090160589,1.,-0.562955993082262));
#33368=CARTESIAN_POINT('Ctrl Pts',(2.06805732997334,1.,-0.567368421181087));
#33369=CARTESIAN_POINT('Ctrl Pts',(2.07261449292824,1.,-0.571816823242603));
#33370=CARTESIAN_POINT('Ctrl Pts',(2.07715226767559,1.,-0.576300797416845));
#33371=CARTESIAN_POINT('Ctrl Pts',(2.08167059018418,1.,-0.580819952108064));
#33372=CARTESIAN_POINT('Ctrl Pts',(2.08616943727951,1.,-0.585373918991617));
#33373=CARTESIAN_POINT('Ctrl Pts',(2.09064881812129,1.,-0.589962365403406));
#33374=CARTESIAN_POINT('Ctrl Pts',(2.0951087622027,1.,-0.594585006052162));
#33375=CARTESIAN_POINT('Ctrl Pts',(2.0995493086477,1.,-0.599241616420534));
#33376=CARTESIAN_POINT('Ctrl Pts',(2.10397049886949,1.,-0.60393203073603));
#33377=CARTESIAN_POINT('Ctrl Pts',(2.1074919961518,1.,-0.607711315454876));
#33378=CARTESIAN_POINT('Ctrl Pts',(2.11012443807238,1.,-0.610560911689899));
#33379=CARTESIAN_POINT('Ctrl Pts',(2.11187554259986,1.,-0.6124673655618));
#33380=CARTESIAN_POINT('Ctrl Pts',(2.11275013067528,1.,-0.61342227326009));
#33381=CARTESIAN_POINT('',(1.7075470150345,0.,-0.383122945602001));
#33382=CARTESIAN_POINT('Origin',(0.,0.,0.));
#33383=CARTESIAN_POINT('',(1.74236521665491,1.,-0.163289472382896));
#33384=CARTESIAN_POINT('Origin',(0.,1.,0.));
#33385=CARTESIAN_POINT('',(1.74236521665491,0.,-0.163289472382896));
#33386=CARTESIAN_POINT('Ctrl Pts',(2.19890268624765,-1.,-0.0694764450219582));
#33387=CARTESIAN_POINT('Ctrl Pts',(2.19890268624765,1.,-0.0694764450219582));
#33388=CARTESIAN_POINT('Ctrl Pts',(2.19777582085423,-1.,-0.0701143536325491));
#33389=CARTESIAN_POINT('Ctrl Pts',(2.19777582085423,1.,-0.0701143536325491));
#33390=CARTESIAN_POINT('Ctrl Pts',(2.19552129484002,-1.,-0.0713863779526155));
#33391=CARTESIAN_POINT('Ctrl Pts',(2.19552129484002,1.,-0.0713863779526155));
#33392=CARTESIAN_POINT('Ctrl Pts',(2.19213712013662,-1.,-0.0732830357306726));
#33393=CARTESIAN_POINT('Ctrl Pts',(2.19213712013662,1.,-0.0732830357306726));
#33394=CARTESIAN_POINT('Ctrl Pts',(2.1876201139953,-1.,-0.0757891465836149));
#33395=CARTESIAN_POINT('Ctrl Pts',(2.1876201139953,1.,-0.0757891465836149));
#33396=CARTESIAN_POINT('Ctrl Pts',(2.18196589448887,-1.,-0.0788837727685244));
#33397=CARTESIAN_POINT('Ctrl Pts',(2.18196589448887,1.,-0.0788837727685244));
#33398=CARTESIAN_POINT('Ctrl Pts',(2.176303712113,-1.,-0.0819402680872767));
#33399=CARTESIAN_POINT('Ctrl Pts',(2.176303712113,1.,-0.0819402680872767));
#33400=CARTESIAN_POINT('Ctrl Pts',(2.17063357870952,-1.,-0.0849584620835374));
#33401=CARTESIAN_POINT('Ctrl Pts',(2.17063357870952,1.,-0.0849584620835374));
#33402=CARTESIAN_POINT('Ctrl Pts',(2.16495552645014,-1.,-0.0879381291386924));
#33403=CARTESIAN_POINT('Ctrl Pts',(2.16495552645014,1.,-0.0879381291386924));
#33404=CARTESIAN_POINT('Ctrl Pts',(2.15926961544516,-1.,-0.0908789888107267));
#33405=CARTESIAN_POINT('Ctrl Pts',(2.15926961544516,1.,-0.0908789888107267));
#33406=CARTESIAN_POINT('Ctrl Pts',(2.1535759397817,-1.,-0.0937807218867645));
#33407=CARTESIAN_POINT('Ctrl Pts',(2.1535759397817,1.,-0.0937807218867645));
#33408=CARTESIAN_POINT('Ctrl Pts',(2.14787463531795,-1.,-0.096642985230546));
#33409=CARTESIAN_POINT('Ctrl Pts',(2.14787463531795,1.,-0.096642985230546));
#33410=CARTESIAN_POINT('Ctrl Pts',(2.14216588396025,-1.,-0.0994654261990917));
#33411=CARTESIAN_POINT('Ctrl Pts',(2.14216588396025,1.,-0.0994654261990917));
#33412=CARTESIAN_POINT('Ctrl Pts',(2.13644992667165,-1.,-0.102247700556101));
#33413=CARTESIAN_POINT('Ctrl Pts',(2.13644992667165,1.,-0.102247700556101));
#33414=CARTESIAN_POINT('Ctrl Pts',(2.13072704887293,-1.,-0.10498947915274));
#33415=CARTESIAN_POINT('Ctrl Pts',(2.13072704887293,1.,-0.10498947915274));
#33416=CARTESIAN_POINT('Ctrl Pts',(2.12499752307,-1.,-0.10769043523109));
#33417=CARTESIAN_POINT('Ctrl Pts',(2.12499752307,1.,-0.10769043523109));
#33418=CARTESIAN_POINT('Ctrl Pts',(2.11926155590865,-1.,-0.110350236135025));
#33419=CARTESIAN_POINT('Ctrl Pts',(2.11926155590865,1.,-0.110350236135025));
#33420=CARTESIAN_POINT('Ctrl Pts',(2.11351924490306,-1.,-0.112968534419737));
#33421=CARTESIAN_POINT('Ctrl Pts',(2.11351924490306,1.,-0.112968534419737));
#33422=CARTESIAN_POINT('Ctrl Pts',(2.10777050261309,-1.,-0.115544957687927));
#33423=CARTESIAN_POINT('Ctrl Pts',(2.10777050261309,1.,-0.115544957687927));
#33424=CARTESIAN_POINT('Ctrl Pts',(2.102015121329,-1.,-0.118079107988356));
#33425=CARTESIAN_POINT('Ctrl Pts',(2.102015121329,1.,-0.118079107988356));
#33426=CARTESIAN_POINT('Ctrl Pts',(2.0962529286773,-1.,-0.120570567965122));
#33427=CARTESIAN_POINT('Ctrl Pts',(2.0962529286773,1.,-0.120570567965122));
#33428=CARTESIAN_POINT('Ctrl Pts',(2.09048392424825,-1.,-0.123018905621083));
#33429=CARTESIAN_POINT('Ctrl Pts',(2.09048392424825,1.,-0.123018905621083));
#33430=CARTESIAN_POINT('Ctrl Pts',(2.08470840653643,-1.,-0.125423679412062));
#33431=CARTESIAN_POINT('Ctrl Pts',(2.08470840653643,1.,-0.125423679412062));
#33432=CARTESIAN_POINT('Ctrl Pts',(2.07892715110987,-1.,-0.12778444527612));
#33433=CARTESIAN_POINT('Ctrl Pts',(2.07892715110987,1.,-0.12778444527612));
#33434=CARTESIAN_POINT('Ctrl Pts',(2.07314114713063,-1.,-0.130100748328404));
#33435=CARTESIAN_POINT('Ctrl Pts',(2.07314114713063,1.,-0.130100748328404));
#33436=CARTESIAN_POINT('Ctrl Pts',(2.06735123910326,-1.,-0.132372111547711));
#33437=CARTESIAN_POINT('Ctrl Pts',(2.06735123910326,1.,-0.132372111547711));
#33438=CARTESIAN_POINT('Ctrl Pts',(2.06155781517842,-1.,-0.134598026192106));
#33439=CARTESIAN_POINT('Ctrl Pts',(2.06155781517842,1.,-0.134598026192106));
#33440=CARTESIAN_POINT('Ctrl Pts',(2.05576044414264,-1.,-0.136777941218044));
#33441=CARTESIAN_POINT('Ctrl Pts',(2.05576044414264,1.,-0.136777941218044));
#33442=CARTESIAN_POINT('Ctrl Pts',(2.04995762001328,-1.,-0.138911255368966));
#33443=CARTESIAN_POINT('Ctrl Pts',(2.04995762001328,1.,-0.138911255368966));
#33444=CARTESIAN_POINT('Ctrl Pts',(2.04414757947916,-1.,-0.140997332152546));
#33445=CARTESIAN_POINT('Ctrl Pts',(2.04414757947916,1.,-0.140997332152546));
#33446=CARTESIAN_POINT('Ctrl Pts',(2.03832911025912,-1.,-0.143035515058209));
#33447=CARTESIAN_POINT('Ctrl Pts',(2.03832911025912,1.,-0.143035515058209));
#33448=CARTESIAN_POINT('Ctrl Pts',(2.03250223739942,-1.,-0.145025140186058));
#33449=CARTESIAN_POINT('Ctrl Pts',(2.03250223739942,1.,-0.145025140186058));
#33450=CARTESIAN_POINT('Ctrl Pts',(2.02666926182017,-1.,-0.146965557332583));
#33451=CARTESIAN_POINT('Ctrl Pts',(2.02666926182017,1.,-0.146965557332583));
#33452=CARTESIAN_POINT('Ctrl Pts',(2.02083464969894,-1.,-0.148856124775337));
#33453=CARTESIAN_POINT('Ctrl Pts',(2.02083464969894,1.,-0.148856124775337));
#33454=CARTESIAN_POINT('Ctrl Pts',(2.01500291940238,-1.,-0.150696157673078));
#33455=CARTESIAN_POINT('Ctrl Pts',(2.01500291940238,1.,-0.150696157673078));
#33456=CARTESIAN_POINT('Ctrl Pts',(2.00917680318424,-1.,-0.15248488362145));
#33457=CARTESIAN_POINT('Ctrl Pts',(2.00917680318424,1.,-0.15248488362145));
#33458=CARTESIAN_POINT('Ctrl Pts',(2.00335565310543,-1.,-0.154221403049722));
#33459=CARTESIAN_POINT('Ctrl Pts',(2.00335565310543,1.,-0.154221403049722));
#33460=CARTESIAN_POINT('Ctrl Pts',(1.99753284771497,-1.,-0.155904629548784));
#33461=CARTESIAN_POINT('Ctrl Pts',(1.99753284771497,1.,-0.155904629548784));
#33462=CARTESIAN_POINT('Ctrl Pts',(1.99169810931908,-1.,-0.157533331459227));
#33463=CARTESIAN_POINT('Ctrl Pts',(1.99169810931908,1.,-0.157533331459227));
#33464=CARTESIAN_POINT('Ctrl Pts',(1.98584238283292,-1.,-0.159106226437299));
#33465=CARTESIAN_POINT('Ctrl Pts',(1.98584238283292,1.,-0.159106226437299));
#33466=CARTESIAN_POINT('Ctrl Pts',(1.97996195437559,-1.,-0.160622060784611));
#33467=CARTESIAN_POINT('Ctrl Pts',(1.97996195437559,1.,-0.160622060784611));
#33468=CARTESIAN_POINT('Ctrl Pts',(1.97406280235188,-1.,-0.162079693556289));
#33469=CARTESIAN_POINT('Ctrl Pts',(1.97406280235188,1.,-0.162079693556289));
#33470=CARTESIAN_POINT('Ctrl Pts',(1.96816512677967,-1.,-0.163478185457734));
#33471=CARTESIAN_POINT('Ctrl Pts',(1.96816512677967,1.,-0.163478185457734));
#33472=CARTESIAN_POINT('Ctrl Pts',(1.96229379940136,-1.,-0.164816568920269));
#33473=CARTESIAN_POINT('Ctrl Pts',(1.96229379940136,1.,-0.164816568920269));
#33474=CARTESIAN_POINT('Ctrl Pts',(1.9564675971873,-1.,-0.166093592002813));
#33475=CARTESIAN_POINT('Ctrl Pts',(1.9564675971873,1.,-0.166093592002813));
#33476=CARTESIAN_POINT('Ctrl Pts',(1.95069027794294,-1.,-0.167307501784476));
#33477=CARTESIAN_POINT('Ctrl Pts',(1.95069027794294,1.,-0.167307501784476));
#33478=CARTESIAN_POINT('Ctrl Pts',(1.94493757756931,-1.,-0.168455741607556));
#33479=CARTESIAN_POINT('Ctrl Pts',(1.94493757756931,1.,-0.168455741607556));
#33480=CARTESIAN_POINT('Ctrl Pts',(1.93915639211581,-1.,-0.169534904817491));
#33481=CARTESIAN_POINT('Ctrl Pts',(1.93915639211581,1.,-0.169534904817491));
#33482=CARTESIAN_POINT('Ctrl Pts',(1.93329183155539,-1.,-0.170541253116202));
#33483=CARTESIAN_POINT('Ctrl Pts',(1.93329183155539,1.,-0.170541253116202));
#33484=CARTESIAN_POINT('Ctrl Pts',(1.92731093582036,-1.,-0.171471191532988));
#33485=CARTESIAN_POINT('Ctrl Pts',(1.92731093582036,1.,-0.171471191532988));
#33486=CARTESIAN_POINT('Ctrl Pts',(1.9212233439798,-1.,-0.172321621259514));
#33487=CARTESIAN_POINT('Ctrl Pts',(1.9212233439798,1.,-0.172321621259514));
#33488=CARTESIAN_POINT('Ctrl Pts',(1.91511429159527,-1.,-0.173090695383496));
#33489=CARTESIAN_POINT('Ctrl Pts',(1.91511429159527,1.,-0.173090695383496));
#33490=CARTESIAN_POINT('Ctrl Pts',(1.90911693975267,-1.,-0.173776635257817));
#33491=CARTESIAN_POINT('Ctrl Pts',(1.90911693975267,1.,-0.173776635257817));
#33492=CARTESIAN_POINT('Ctrl Pts',(1.90335253862834,-1.,-0.174375518661085));
#33493=CARTESIAN_POINT('Ctrl Pts',(1.90335253862834,1.,-0.174375518661085));
#33494=CARTESIAN_POINT('Ctrl Pts',(1.89788101117132,-1.,-0.174879405091263));
#33495=CARTESIAN_POINT('Ctrl Pts',(1.89788101117132,1.,-0.174879405091263));
#33496=CARTESIAN_POINT('Ctrl Pts',(1.892646301985,-1.,-0.175274276190844));
#33497=CARTESIAN_POINT('Ctrl Pts',(1.892646301985,1.,-0.175274276190844));
#33498=CARTESIAN_POINT('Ctrl Pts',(1.88742606273259,-1.,-0.175538155840648));
#33499=CARTESIAN_POINT('Ctrl Pts',(1.88742606273259,1.,-0.175538155840648));
#33500=CARTESIAN_POINT('Ctrl Pts',(1.88188663145367,-1.,-0.175644148889699));
#33501=CARTESIAN_POINT('Ctrl Pts',(1.88188663145367,1.,-0.175644148889699));
#33502=CARTESIAN_POINT('Ctrl Pts',(1.87563767773588,-1.,-0.175563480746485));
#33503=CARTESIAN_POINT('Ctrl Pts',(1.87563767773588,1.,-0.175563480746485));
#33504=CARTESIAN_POINT('Ctrl Pts',(1.86828349694799,-1.,-0.175268337590758));
#33505=CARTESIAN_POINT('Ctrl Pts',(1.86828349694799,1.,-0.175268337590758));
#33506=CARTESIAN_POINT('Ctrl Pts',(1.85948367088837,-1.,-0.17473525927603));
#33507=CARTESIAN_POINT('Ctrl Pts',(1.85948367088837,1.,-0.17473525927603));
#33508=CARTESIAN_POINT('Ctrl Pts',(1.8489811319852,-1.,-0.173946627587732));
#33509=CARTESIAN_POINT('Ctrl Pts',(1.8489811319852,1.,-0.173946627587732));
#33510=CARTESIAN_POINT('Ctrl Pts',(1.83658380527692,-1.,-0.1728894428919));
#33511=CARTESIAN_POINT('Ctrl Pts',(1.83658380527692,1.,-0.1728894428919));
#33512=CARTESIAN_POINT('Ctrl Pts',(1.82215766811545,-1.,-0.171554770204119));
#33513=CARTESIAN_POINT('Ctrl Pts',(1.82215766811545,1.,-0.171554770204119));
#33514=CARTESIAN_POINT('Ctrl Pts',(1.80561530629706,-1.,-0.169936923904608));
#33515=CARTESIAN_POINT('Ctrl Pts',(1.80561530629706,1.,-0.169936923904608));
#33516=CARTESIAN_POINT('Ctrl Pts',(1.7869064998507,-1.,-0.168032772805197));
#33517=CARTESIAN_POINT('Ctrl Pts',(1.7869064998507,1.,-0.168032772805197));
#33518=CARTESIAN_POINT('Ctrl Pts',(1.77018771684844,-1.,-0.1662793551464));
#33519=CARTESIAN_POINT('Ctrl Pts',(1.77018771684844,1.,-0.1662793551464));
#33520=CARTESIAN_POINT('Ctrl Pts',(1.75666056638427,-1.,-0.164834765707159));
#33521=CARTESIAN_POINT('Ctrl Pts',(1.75666056638427,1.,-0.164834765707159));
#33522=CARTESIAN_POINT('Ctrl Pts',(1.7472034950333,-1.,-0.163814161002002));
#33523=CARTESIAN_POINT('Ctrl Pts',(1.7472034950333,1.,-0.163814161002002));
#33524=CARTESIAN_POINT('Ctrl Pts',(1.74236521665491,-1.,-0.163289472382896));
#33525=CARTESIAN_POINT('Ctrl Pts',(1.74236521665491,1.,-0.163289472382896));
#33526=CARTESIAN_POINT('',(2.19890268624765,1.,-0.0694764450219582));
#33527=CARTESIAN_POINT('Ctrl Pts',(2.19890268624765,1.,-0.0694764450219582));
#33528=CARTESIAN_POINT('Ctrl Pts',(2.19777582085423,1.,-0.0701143536325491));
#33529=CARTESIAN_POINT('Ctrl Pts',(2.19552129484002,1.,-0.0713863779526155));
#33530=CARTESIAN_POINT('Ctrl Pts',(2.19213712013662,1.,-0.0732830357306726));
#33531=CARTESIAN_POINT('Ctrl Pts',(2.1876201139953,1.,-0.0757891465836149));
#33532=CARTESIAN_POINT('Ctrl Pts',(2.18196589448887,1.,-0.0788837727685244));
#33533=CARTESIAN_POINT('Ctrl Pts',(2.176303712113,1.,-0.0819402680872767));
#33534=CARTESIAN_POINT('Ctrl Pts',(2.17063357870952,1.,-0.0849584620835374));
#33535=CARTESIAN_POINT('Ctrl Pts',(2.16495552645014,1.,-0.0879381291386924));
#33536=CARTESIAN_POINT('Ctrl Pts',(2.15926961544516,1.,-0.0908789888107267));
#33537=CARTESIAN_POINT('Ctrl Pts',(2.1535759397817,1.,-0.0937807218867645));
#33538=CARTESIAN_POINT('Ctrl Pts',(2.14787463531795,1.,-0.096642985230546));
#33539=CARTESIAN_POINT('Ctrl Pts',(2.14216588396025,1.,-0.0994654261990917));
#33540=CARTESIAN_POINT('Ctrl Pts',(2.13644992667165,1.,-0.102247700556101));
#33541=CARTESIAN_POINT('Ctrl Pts',(2.13072704887293,1.,-0.10498947915274));
#33542=CARTESIAN_POINT('Ctrl Pts',(2.12499752307,1.,-0.10769043523109));
#33543=CARTESIAN_POINT('Ctrl Pts',(2.11926155590865,1.,-0.110350236135025));
#33544=CARTESIAN_POINT('Ctrl Pts',(2.11351924490306,1.,-0.112968534419737));
#33545=CARTESIAN_POINT('Ctrl Pts',(2.10777050261309,1.,-0.115544957687927));
#33546=CARTESIAN_POINT('Ctrl Pts',(2.102015121329,1.,-0.118079107988356));
#33547=CARTESIAN_POINT('Ctrl Pts',(2.0962529286773,1.,-0.120570567965122));
#33548=CARTESIAN_POINT('Ctrl Pts',(2.09048392424825,1.,-0.123018905621083));
#33549=CARTESIAN_POINT('Ctrl Pts',(2.08470840653643,1.,-0.125423679412062));
#33550=CARTESIAN_POINT('Ctrl Pts',(2.07892715110987,1.,-0.12778444527612));
#33551=CARTESIAN_POINT('Ctrl Pts',(2.07314114713063,1.,-0.130100748328404));
#33552=CARTESIAN_POINT('Ctrl Pts',(2.06735123910326,1.,-0.132372111547711));
#33553=CARTESIAN_POINT('Ctrl Pts',(2.06155781517842,1.,-0.134598026192106));
#33554=CARTESIAN_POINT('Ctrl Pts',(2.05576044414264,1.,-0.136777941218044));
#33555=CARTESIAN_POINT('Ctrl Pts',(2.04995762001328,1.,-0.138911255368966));
#33556=CARTESIAN_POINT('Ctrl Pts',(2.04414757947916,1.,-0.140997332152546));
#33557=CARTESIAN_POINT('Ctrl Pts',(2.03832911025912,1.,-0.143035515058209));
#33558=CARTESIAN_POINT('Ctrl Pts',(2.03250223739942,1.,-0.145025140186058));
#33559=CARTESIAN_POINT('Ctrl Pts',(2.02666926182017,1.,-0.146965557332583));
#33560=CARTESIAN_POINT('Ctrl Pts',(2.02083464969894,1.,-0.148856124775337));
#33561=CARTESIAN_POINT('Ctrl Pts',(2.01500291940238,1.,-0.150696157673078));
#33562=CARTESIAN_POINT('Ctrl Pts',(2.00917680318424,1.,-0.15248488362145));
#33563=CARTESIAN_POINT('Ctrl Pts',(2.00335565310543,1.,-0.154221403049722));
#33564=CARTESIAN_POINT('Ctrl Pts',(1.99753284771497,1.,-0.155904629548784));
#33565=CARTESIAN_POINT('Ctrl Pts',(1.99169810931908,1.,-0.157533331459227));
#33566=CARTESIAN_POINT('Ctrl Pts',(1.98584238283292,1.,-0.159106226437299));
#33567=CARTESIAN_POINT('Ctrl Pts',(1.97996195437559,1.,-0.160622060784611));
#33568=CARTESIAN_POINT('Ctrl Pts',(1.97406280235188,1.,-0.162079693556289));
#33569=CARTESIAN_POINT('Ctrl Pts',(1.96816512677967,1.,-0.163478185457734));
#33570=CARTESIAN_POINT('Ctrl Pts',(1.96229379940136,1.,-0.164816568920269));
#33571=CARTESIAN_POINT('Ctrl Pts',(1.9564675971873,1.,-0.166093592002813));
#33572=CARTESIAN_POINT('Ctrl Pts',(1.95069027794294,1.,-0.167307501784476));
#33573=CARTESIAN_POINT('Ctrl Pts',(1.94493757756931,1.,-0.168455741607556));
#33574=CARTESIAN_POINT('Ctrl Pts',(1.93915639211581,1.,-0.169534904817491));
#33575=CARTESIAN_POINT('Ctrl Pts',(1.93329183155539,1.,-0.170541253116202));
#33576=CARTESIAN_POINT('Ctrl Pts',(1.92731093582036,1.,-0.171471191532988));
#33577=CARTESIAN_POINT('Ctrl Pts',(1.9212233439798,1.,-0.172321621259514));
#33578=CARTESIAN_POINT('Ctrl Pts',(1.91511429159527,1.,-0.173090695383496));
#33579=CARTESIAN_POINT('Ctrl Pts',(1.90911693975267,1.,-0.173776635257817));
#33580=CARTESIAN_POINT('Ctrl Pts',(1.90335253862834,1.,-0.174375518661085));
#33581=CARTESIAN_POINT('Ctrl Pts',(1.89788101117132,1.,-0.174879405091263));
#33582=CARTESIAN_POINT('Ctrl Pts',(1.892646301985,1.,-0.175274276190844));
#33583=CARTESIAN_POINT('Ctrl Pts',(1.88742606273259,1.,-0.175538155840648));
#33584=CARTESIAN_POINT('Ctrl Pts',(1.88188663145367,1.,-0.175644148889699));
#33585=CARTESIAN_POINT('Ctrl Pts',(1.87563767773588,1.,-0.175563480746485));
#33586=CARTESIAN_POINT('Ctrl Pts',(1.86828349694799,1.,-0.175268337590758));
#33587=CARTESIAN_POINT('Ctrl Pts',(1.85948367088837,1.,-0.17473525927603));
#33588=CARTESIAN_POINT('Ctrl Pts',(1.8489811319852,1.,-0.173946627587732));
#33589=CARTESIAN_POINT('Ctrl Pts',(1.83658380527692,1.,-0.1728894428919));
#33590=CARTESIAN_POINT('Ctrl Pts',(1.82215766811545,1.,-0.171554770204119));
#33591=CARTESIAN_POINT('Ctrl Pts',(1.80561530629706,1.,-0.169936923904608));
#33592=CARTESIAN_POINT('Ctrl Pts',(1.7869064998507,1.,-0.168032772805197));
#33593=CARTESIAN_POINT('Ctrl Pts',(1.77018771684844,1.,-0.1662793551464));
#33594=CARTESIAN_POINT('Ctrl Pts',(1.75666056638427,1.,-0.164834765707159));
#33595=CARTESIAN_POINT('Ctrl Pts',(1.7472034950333,1.,-0.163814161002002));
#33596=CARTESIAN_POINT('Ctrl Pts',(1.74236521665491,1.,-0.163289472382896));
#33597=CARTESIAN_POINT('',(2.19890268624765,0.,-0.0694764450219582));
#33598=CARTESIAN_POINT('Origin',(2.19890268624765,0.,0.0694764450219582));
#33599=CARTESIAN_POINT('',(2.19890268624765,1.,0.0694764450219582));
#33600=CARTESIAN_POINT('',(2.19890268624765,1.,-0.0694764450219582));
#33601=CARTESIAN_POINT('',(2.19890268624765,0.,0.0694764450219582));
#33602=CARTESIAN_POINT('Ctrl Pts',(1.74236521665491,-1.,0.163289472382896));
#33603=CARTESIAN_POINT('Ctrl Pts',(1.74236521665491,1.,0.163289472382896));
#33604=CARTESIAN_POINT('Ctrl Pts',(1.74720349503904,-1.,0.163814161002474));
#33605=CARTESIAN_POINT('Ctrl Pts',(1.74720349503904,1.,0.163814161002474));
#33606=CARTESIAN_POINT('Ctrl Pts',(1.75666056640041,-1.,0.164834765708484));
#33607=CARTESIAN_POINT('Ctrl Pts',(1.75666056640041,1.,0.164834765708484));
#33608=CARTESIAN_POINT('Ctrl Pts',(1.77018771687692,-1.,0.166279355148738));
#33609=CARTESIAN_POINT('Ctrl Pts',(1.77018771687692,1.,0.166279355148738));
#33610=CARTESIAN_POINT('Ctrl Pts',(1.78690649988931,-1.,0.16803277280837));
#33611=CARTESIAN_POINT('Ctrl Pts',(1.78690649988931,1.,0.16803277280837));
#33612=CARTESIAN_POINT('Ctrl Pts',(1.80561530633924,-1.,0.169936923908078));
#33613=CARTESIAN_POINT('Ctrl Pts',(1.80561530633924,1.,0.169936923908078));
#33614=CARTESIAN_POINT('Ctrl Pts',(1.82215766815414,-1.,0.171554770207306));
#33615=CARTESIAN_POINT('Ctrl Pts',(1.82215766815414,1.,0.171554770207306));
#33616=CARTESIAN_POINT('Ctrl Pts',(1.83658380530747,-1.,0.17288944289442));
#33617=CARTESIAN_POINT('Ctrl Pts',(1.83658380530747,1.,0.17288944289442));
#33618=CARTESIAN_POINT('Ctrl Pts',(1.84898113200543,-1.,0.173946627589401));
#33619=CARTESIAN_POINT('Ctrl Pts',(1.84898113200543,1.,0.173946627589401));
#33620=CARTESIAN_POINT('Ctrl Pts',(1.85948367089838,-1.,0.174735259276856));
#33621=CARTESIAN_POINT('Ctrl Pts',(1.85948367089838,1.,0.174735259276856));
#33622=CARTESIAN_POINT('Ctrl Pts',(1.86828349694972,-1.,0.1752683375909));
#33623=CARTESIAN_POINT('Ctrl Pts',(1.86828349694972,1.,0.1752683375909));
#33624=CARTESIAN_POINT('Ctrl Pts',(1.87563767773249,-1.,0.175563480746205));
#33625=CARTESIAN_POINT('Ctrl Pts',(1.87563767773249,1.,0.175563480746205));
#33626=CARTESIAN_POINT('Ctrl Pts',(1.88188663144846,-1.,0.175644148889271));
#33627=CARTESIAN_POINT('Ctrl Pts',(1.88188663144846,1.,0.175644148889271));
#33628=CARTESIAN_POINT('Ctrl Pts',(1.88742606272818,-1.,0.175538155840286));
#33629=CARTESIAN_POINT('Ctrl Pts',(1.88742606272818,1.,0.175538155840286));
#33630=CARTESIAN_POINT('Ctrl Pts',(1.89264630198279,-1.,0.175274276190664));
#33631=CARTESIAN_POINT('Ctrl Pts',(1.89264630198279,1.,0.175274276190664));
#33632=CARTESIAN_POINT('Ctrl Pts',(1.89788101117148,-1.,0.174879405091277));
#33633=CARTESIAN_POINT('Ctrl Pts',(1.89788101117148,1.,0.174879405091277));
#33634=CARTESIAN_POINT('Ctrl Pts',(1.90335253863003,-1.,0.174375518661222));
#33635=CARTESIAN_POINT('Ctrl Pts',(1.90335253863003,1.,0.174375518661222));
#33636=CARTESIAN_POINT('Ctrl Pts',(1.90911693975475,-1.,0.173776635257983));
#33637=CARTESIAN_POINT('Ctrl Pts',(1.90911693975475,1.,0.173776635257983));
#33638=CARTESIAN_POINT('Ctrl Pts',(1.91511429159681,-1.,0.173090695383619));
#33639=CARTESIAN_POINT('Ctrl Pts',(1.91511429159681,1.,0.173090695383619));
#33640=CARTESIAN_POINT('Ctrl Pts',(1.92122334398034,-1.,0.172321621259556));
#33641=CARTESIAN_POINT('Ctrl Pts',(1.92122334398034,1.,0.172321621259556));
#33642=CARTESIAN_POINT('Ctrl Pts',(1.92731093582,-1.,0.17147119153296));
#33643=CARTESIAN_POINT('Ctrl Pts',(1.92731093582,1.,0.17147119153296));
#33644=CARTESIAN_POINT('Ctrl Pts',(1.93329183155455,-1.,0.170541253116136));
#33645=CARTESIAN_POINT('Ctrl Pts',(1.93329183155455,1.,0.170541253116136));
#33646=CARTESIAN_POINT('Ctrl Pts',(1.93915639211497,-1.,0.169534904817425));
#33647=CARTESIAN_POINT('Ctrl Pts',(1.93915639211497,1.,0.169534904817425));
#33648=CARTESIAN_POINT('Ctrl Pts',(1.94493757756879,-1.,0.168455741607515));
#33649=CARTESIAN_POINT('Ctrl Pts',(1.94493757756879,1.,0.168455741607515));
#33650=CARTESIAN_POINT('Ctrl Pts',(1.95069027794286,-1.,0.167307501784469));
#33651=CARTESIAN_POINT('Ctrl Pts',(1.95069027794286,1.,0.167307501784469));
#33652=CARTESIAN_POINT('Ctrl Pts',(1.95646759718755,-1.,0.166093592002832));
#33653=CARTESIAN_POINT('Ctrl Pts',(1.95646759718755,1.,0.166093592002832));
#33654=CARTESIAN_POINT('Ctrl Pts',(1.96229379940174,-1.,0.1648165689203));
#33655=CARTESIAN_POINT('Ctrl Pts',(1.96229379940174,1.,0.1648165689203));
#33656=CARTESIAN_POINT('Ctrl Pts',(1.96816512678,-1.,0.16347818545776));
#33657=CARTESIAN_POINT('Ctrl Pts',(1.96816512678,1.,0.16347818545776));
#33658=CARTESIAN_POINT('Ctrl Pts',(1.97406280235204,-1.,0.162079693556302));
#33659=CARTESIAN_POINT('Ctrl Pts',(1.97406280235204,1.,0.162079693556302));
#33660=CARTESIAN_POINT('Ctrl Pts',(1.97996195437557,-1.,0.16062206078461));
#33661=CARTESIAN_POINT('Ctrl Pts',(1.97996195437557,1.,0.16062206078461));
#33662=CARTESIAN_POINT('Ctrl Pts',(1.98584238283279,-1.,0.159106226437288));
#33663=CARTESIAN_POINT('Ctrl Pts',(1.98584238283279,1.,0.159106226437288));
#33664=CARTESIAN_POINT('Ctrl Pts',(1.99169810931893,-1.,0.157533331459215));
#33665=CARTESIAN_POINT('Ctrl Pts',(1.99169810931893,1.,0.157533331459215));
#33666=CARTESIAN_POINT('Ctrl Pts',(1.99753284771487,-1.,0.155904629548774));
#33667=CARTESIAN_POINT('Ctrl Pts',(1.99753284771487,1.,0.155904629548774));
#33668=CARTESIAN_POINT('Ctrl Pts',(2.00335565310539,-1.,0.154221403049719));
#33669=CARTESIAN_POINT('Ctrl Pts',(2.00335565310539,1.,0.154221403049719));
#33670=CARTESIAN_POINT('Ctrl Pts',(2.00917680318426,-1.,0.152484883621452));
#33671=CARTESIAN_POINT('Ctrl Pts',(2.00917680318426,1.,0.152484883621452));
#33672=CARTESIAN_POINT('Ctrl Pts',(2.01500291940243,-1.,0.150696157673084));
#33673=CARTESIAN_POINT('Ctrl Pts',(2.01500291940243,1.,0.150696157673084));
#33674=CARTESIAN_POINT('Ctrl Pts',(2.02083464969897,-1.,0.148856124775342));
#33675=CARTESIAN_POINT('Ctrl Pts',(2.02083464969897,1.,0.148856124775342));
#33676=CARTESIAN_POINT('Ctrl Pts',(2.02666926182017,-1.,0.146965557332586));
#33677=CARTESIAN_POINT('Ctrl Pts',(2.02666926182017,1.,0.146965557332586));
#33678=CARTESIAN_POINT('Ctrl Pts',(2.03250223739941,-1.,0.145025140186058));
#33679=CARTESIAN_POINT('Ctrl Pts',(2.03250223739941,1.,0.145025140186058));
#33680=CARTESIAN_POINT('Ctrl Pts',(2.03832911025913,-1.,0.143035515058208));
#33681=CARTESIAN_POINT('Ctrl Pts',(2.03832911025913,1.,0.143035515058208));
#33682=CARTESIAN_POINT('Ctrl Pts',(2.04414757947919,-1.,0.140997332152545));
#33683=CARTESIAN_POINT('Ctrl Pts',(2.04414757947919,1.,0.140997332152545));
#33684=CARTESIAN_POINT('Ctrl Pts',(2.04995762001333,-1.,0.138911255368966));
#33685=CARTESIAN_POINT('Ctrl Pts',(2.04995762001333,1.,0.138911255368966));
#33686=CARTESIAN_POINT('Ctrl Pts',(2.0557604441427,-1.,0.136777941218044));
#33687=CARTESIAN_POINT('Ctrl Pts',(2.0557604441427,1.,0.136777941218044));
#33688=CARTESIAN_POINT('Ctrl Pts',(2.06155781517844,-1.,0.134598026192107));
#33689=CARTESIAN_POINT('Ctrl Pts',(2.06155781517844,1.,0.134598026192107));
#33690=CARTESIAN_POINT('Ctrl Pts',(2.06735123910319,-1.,0.132372111547709));
#33691=CARTESIAN_POINT('Ctrl Pts',(2.06735123910319,1.,0.132372111547709));
#33692=CARTESIAN_POINT('Ctrl Pts',(2.07314114713047,-1.,0.1301007483284));
#33693=CARTESIAN_POINT('Ctrl Pts',(2.07314114713047,1.,0.1301007483284));
#33694=CARTESIAN_POINT('Ctrl Pts',(2.07892715110967,-1.,0.127784445276116));
#33695=CARTESIAN_POINT('Ctrl Pts',(2.07892715110967,1.,0.127784445276116));
#33696=CARTESIAN_POINT('Ctrl Pts',(2.08470840653628,-1.,0.125423679412058));
#33697=CARTESIAN_POINT('Ctrl Pts',(2.08470840653628,1.,0.125423679412058));
#33698=CARTESIAN_POINT('Ctrl Pts',(2.09048392424826,-1.,0.123018905621083));
#33699=CARTESIAN_POINT('Ctrl Pts',(2.09048392424826,1.,0.123018905621083));
#33700=CARTESIAN_POINT('Ctrl Pts',(2.09625292867756,-1.,0.120570567965129));
#33701=CARTESIAN_POINT('Ctrl Pts',(2.09625292867756,1.,0.120570567965129));
#33702=CARTESIAN_POINT('Ctrl Pts',(2.10201512132945,-1.,0.118079107988368));
#33703=CARTESIAN_POINT('Ctrl Pts',(2.10201512132945,1.,0.118079107988368));
#33704=CARTESIAN_POINT('Ctrl Pts',(2.10777050261359,-1.,0.11554495768794));
#33705=CARTESIAN_POINT('Ctrl Pts',(2.10777050261359,1.,0.11554495768794));
#33706=CARTESIAN_POINT('Ctrl Pts',(2.11351924490335,-1.,0.112968534419746));
#33707=CARTESIAN_POINT('Ctrl Pts',(2.11351924490335,1.,0.112968534419746));
#33708=CARTESIAN_POINT('Ctrl Pts',(2.11926155590849,-1.,0.11035023613502));
#33709=CARTESIAN_POINT('Ctrl Pts',(2.11926155590849,1.,0.11035023613502));
#33710=CARTESIAN_POINT('Ctrl Pts',(2.12499752306927,-1.,0.107690435231068));
#33711=CARTESIAN_POINT('Ctrl Pts',(2.12499752306927,1.,0.107690435231068));
#33712=CARTESIAN_POINT('Ctrl Pts',(2.1307270488718,-1.,0.104989479152703));
#33713=CARTESIAN_POINT('Ctrl Pts',(2.1307270488718,1.,0.104989479152703));
#33714=CARTESIAN_POINT('Ctrl Pts',(2.13644992667052,-1.,0.102247700556063));
#33715=CARTESIAN_POINT('Ctrl Pts',(2.13644992667052,1.,0.102247700556063));
#33716=CARTESIAN_POINT('Ctrl Pts',(2.14216588395974,-1.,0.0994654261990741));
#33717=CARTESIAN_POINT('Ctrl Pts',(2.14216588395974,1.,0.0994654261990741));
#33718=CARTESIAN_POINT('Ctrl Pts',(2.14787463531864,-1.,0.0966429852305688));
#33719=CARTESIAN_POINT('Ctrl Pts',(2.14787463531864,1.,0.0966429852305688));
#33720=CARTESIAN_POINT('Ctrl Pts',(2.15357593978377,-1.,0.0937807218868344));
#33721=CARTESIAN_POINT('Ctrl Pts',(2.15357593978377,1.,0.0937807218868344));
#33722=CARTESIAN_POINT('Ctrl Pts',(2.15926961544808,-1.,0.0908789888108265));
#33723=CARTESIAN_POINT('Ctrl Pts',(2.15926961544808,1.,0.0908789888108265));
#33724=CARTESIAN_POINT('Ctrl Pts',(2.16495552645275,-1.,0.0879381291387821));
#33725=CARTESIAN_POINT('Ctrl Pts',(2.16495552645275,1.,0.0879381291387821));
#33726=CARTESIAN_POINT('Ctrl Pts',(2.17063357871031,-1.,0.0849584620835642));
#33727=CARTESIAN_POINT('Ctrl Pts',(2.17063357871031,1.,0.0849584620835642));
#33728=CARTESIAN_POINT('Ctrl Pts',(2.1763037121106,-1.,0.0819402680871938));
#33729=CARTESIAN_POINT('Ctrl Pts',(2.1763037121106,1.,0.0819402680871938));
#33730=CARTESIAN_POINT('Ctrl Pts',(2.18196589448304,-1.,0.0788837727683226));
#33731=CARTESIAN_POINT('Ctrl Pts',(2.18196589448304,1.,0.0788837727683226));
#33732=CARTESIAN_POINT('Ctrl Pts',(2.1876201139874,-1.,0.075789146583341));
#33733=CARTESIAN_POINT('Ctrl Pts',(2.1876201139874,1.,0.075789146583341));
#33734=CARTESIAN_POINT('Ctrl Pts',(2.19213712012956,-1.,0.0732830357304275));
#33735=CARTESIAN_POINT('Ctrl Pts',(2.19213712012956,1.,0.0732830357304275));
#33736=CARTESIAN_POINT('Ctrl Pts',(2.19552129483562,-1.,0.0713863779524626));
#33737=CARTESIAN_POINT('Ctrl Pts',(2.19552129483562,1.,0.0713863779524626));
#33738=CARTESIAN_POINT('Ctrl Pts',(2.19777582085261,-1.,0.0701143536324925));
#33739=CARTESIAN_POINT('Ctrl Pts',(2.19777582085261,1.,0.0701143536324925));
#33740=CARTESIAN_POINT('Ctrl Pts',(2.19890268624765,-1.,0.0694764450219582));
#33741=CARTESIAN_POINT('Ctrl Pts',(2.19890268624765,1.,0.0694764450219582));
#33742=CARTESIAN_POINT('',(1.74236521665491,1.,0.163289472382896));
#33743=CARTESIAN_POINT('Ctrl Pts',(1.74236521665491,1.,0.163289472382896));
#33744=CARTESIAN_POINT('Ctrl Pts',(1.74720349503904,1.,0.163814161002474));
#33745=CARTESIAN_POINT('Ctrl Pts',(1.75666056640041,1.,0.164834765708484));
#33746=CARTESIAN_POINT('Ctrl Pts',(1.77018771687692,1.,0.166279355148738));
#33747=CARTESIAN_POINT('Ctrl Pts',(1.78690649988931,1.,0.16803277280837));
#33748=CARTESIAN_POINT('Ctrl Pts',(1.80561530633924,1.,0.169936923908078));
#33749=CARTESIAN_POINT('Ctrl Pts',(1.82215766815414,1.,0.171554770207306));
#33750=CARTESIAN_POINT('Ctrl Pts',(1.83658380530747,1.,0.17288944289442));
#33751=CARTESIAN_POINT('Ctrl Pts',(1.84898113200543,1.,0.173946627589401));
#33752=CARTESIAN_POINT('Ctrl Pts',(1.85948367089838,1.,0.174735259276856));
#33753=CARTESIAN_POINT('Ctrl Pts',(1.86828349694972,1.,0.1752683375909));
#33754=CARTESIAN_POINT('Ctrl Pts',(1.87563767773249,1.,0.175563480746205));
#33755=CARTESIAN_POINT('Ctrl Pts',(1.88188663144846,1.,0.175644148889271));
#33756=CARTESIAN_POINT('Ctrl Pts',(1.88742606272818,1.,0.175538155840286));
#33757=CARTESIAN_POINT('Ctrl Pts',(1.89264630198279,1.,0.175274276190664));
#33758=CARTESIAN_POINT('Ctrl Pts',(1.89788101117148,1.,0.174879405091277));
#33759=CARTESIAN_POINT('Ctrl Pts',(1.90335253863003,1.,0.174375518661222));
#33760=CARTESIAN_POINT('Ctrl Pts',(1.90911693975475,1.,0.173776635257983));
#33761=CARTESIAN_POINT('Ctrl Pts',(1.91511429159681,1.,0.173090695383619));
#33762=CARTESIAN_POINT('Ctrl Pts',(1.92122334398034,1.,0.172321621259556));
#33763=CARTESIAN_POINT('Ctrl Pts',(1.92731093582,1.,0.17147119153296));
#33764=CARTESIAN_POINT('Ctrl Pts',(1.93329183155455,1.,0.170541253116136));
#33765=CARTESIAN_POINT('Ctrl Pts',(1.93915639211497,1.,0.169534904817425));
#33766=CARTESIAN_POINT('Ctrl Pts',(1.94493757756879,1.,0.168455741607515));
#33767=CARTESIAN_POINT('Ctrl Pts',(1.95069027794286,1.,0.167307501784469));
#33768=CARTESIAN_POINT('Ctrl Pts',(1.95646759718755,1.,0.166093592002832));
#33769=CARTESIAN_POINT('Ctrl Pts',(1.96229379940174,1.,0.1648165689203));
#33770=CARTESIAN_POINT('Ctrl Pts',(1.96816512678,1.,0.16347818545776));
#33771=CARTESIAN_POINT('Ctrl Pts',(1.97406280235204,1.,0.162079693556302));
#33772=CARTESIAN_POINT('Ctrl Pts',(1.97996195437557,1.,0.16062206078461));
#33773=CARTESIAN_POINT('Ctrl Pts',(1.98584238283279,1.,0.159106226437288));
#33774=CARTESIAN_POINT('Ctrl Pts',(1.99169810931893,1.,0.157533331459215));
#33775=CARTESIAN_POINT('Ctrl Pts',(1.99753284771487,1.,0.155904629548774));
#33776=CARTESIAN_POINT('Ctrl Pts',(2.00335565310539,1.,0.154221403049719));
#33777=CARTESIAN_POINT('Ctrl Pts',(2.00917680318426,1.,0.152484883621452));
#33778=CARTESIAN_POINT('Ctrl Pts',(2.01500291940243,1.,0.150696157673084));
#33779=CARTESIAN_POINT('Ctrl Pts',(2.02083464969897,1.,0.148856124775342));
#33780=CARTESIAN_POINT('Ctrl Pts',(2.02666926182017,1.,0.146965557332586));
#33781=CARTESIAN_POINT('Ctrl Pts',(2.03250223739941,1.,0.145025140186058));
#33782=CARTESIAN_POINT('Ctrl Pts',(2.03832911025913,1.,0.143035515058208));
#33783=CARTESIAN_POINT('Ctrl Pts',(2.04414757947919,1.,0.140997332152545));
#33784=CARTESIAN_POINT('Ctrl Pts',(2.04995762001333,1.,0.138911255368966));
#33785=CARTESIAN_POINT('Ctrl Pts',(2.0557604441427,1.,0.136777941218044));
#33786=CARTESIAN_POINT('Ctrl Pts',(2.06155781517844,1.,0.134598026192107));
#33787=CARTESIAN_POINT('Ctrl Pts',(2.06735123910319,1.,0.132372111547709));
#33788=CARTESIAN_POINT('Ctrl Pts',(2.07314114713047,1.,0.1301007483284));
#33789=CARTESIAN_POINT('Ctrl Pts',(2.07892715110967,1.,0.127784445276116));
#33790=CARTESIAN_POINT('Ctrl Pts',(2.08470840653628,1.,0.125423679412058));
#33791=CARTESIAN_POINT('Ctrl Pts',(2.09048392424826,1.,0.123018905621083));
#33792=CARTESIAN_POINT('Ctrl Pts',(2.09625292867756,1.,0.120570567965129));
#33793=CARTESIAN_POINT('Ctrl Pts',(2.10201512132945,1.,0.118079107988368));
#33794=CARTESIAN_POINT('Ctrl Pts',(2.10777050261359,1.,0.11554495768794));
#33795=CARTESIAN_POINT('Ctrl Pts',(2.11351924490335,1.,0.112968534419746));
#33796=CARTESIAN_POINT('Ctrl Pts',(2.11926155590849,1.,0.11035023613502));
#33797=CARTESIAN_POINT('Ctrl Pts',(2.12499752306927,1.,0.107690435231068));
#33798=CARTESIAN_POINT('Ctrl Pts',(2.1307270488718,1.,0.104989479152703));
#33799=CARTESIAN_POINT('Ctrl Pts',(2.13644992667052,1.,0.102247700556063));
#33800=CARTESIAN_POINT('Ctrl Pts',(2.14216588395974,1.,0.0994654261990741));
#33801=CARTESIAN_POINT('Ctrl Pts',(2.14787463531864,1.,0.0966429852305688));
#33802=CARTESIAN_POINT('Ctrl Pts',(2.15357593978377,1.,0.0937807218868344));
#33803=CARTESIAN_POINT('Ctrl Pts',(2.15926961544808,1.,0.0908789888108265));
#33804=CARTESIAN_POINT('Ctrl Pts',(2.16495552645275,1.,0.0879381291387821));
#33805=CARTESIAN_POINT('Ctrl Pts',(2.17063357871031,1.,0.0849584620835642));
#33806=CARTESIAN_POINT('Ctrl Pts',(2.1763037121106,1.,0.0819402680871938));
#33807=CARTESIAN_POINT('Ctrl Pts',(2.18196589448304,1.,0.0788837727683226));
#33808=CARTESIAN_POINT('Ctrl Pts',(2.1876201139874,1.,0.075789146583341));
#33809=CARTESIAN_POINT('Ctrl Pts',(2.19213712012956,1.,0.0732830357304275));
#33810=CARTESIAN_POINT('Ctrl Pts',(2.19552129483562,1.,0.0713863779524626));
#33811=CARTESIAN_POINT('Ctrl Pts',(2.19777582085261,1.,0.0701143536324925));
#33812=CARTESIAN_POINT('Ctrl Pts',(2.19890268624765,1.,0.0694764450219582));
#33813=CARTESIAN_POINT('',(1.74236521665491,0.,0.163289472382896));
#33814=CARTESIAN_POINT('Origin',(0.,1.,0.));
#33815=CARTESIAN_POINT('Origin',(0.,1.,0.));
#33816=CARTESIAN_POINT('Origin',(0.,0.,0.));
#33817=CARTESIAN_POINT('',(0.,0.,0.));
#33818=CARTESIAN_POINT('',(0.,0.,0.));
#33819=CARTESIAN_POINT('Origin',(6.,0.,14.1));
#33820=CARTESIAN_POINT('',(5.835,-2.02066721859313E-17,14.1));
#33821=CARTESIAN_POINT('Origin',(6.,0.,14.1));
#33822=CARTESIAN_POINT('',(5.835,2.02066721859313E-17,15.));
#33823=CARTESIAN_POINT('',(5.835,-2.02066721859313E-17,14.1));
#33824=CARTESIAN_POINT('Origin',(6.,0.,15.));
#33825=CARTESIAN_POINT('Origin',(6.,0.,14.1));
#33826=CARTESIAN_POINT('Origin',(5.61461979457943,1.07307133838809,11.5));
#33827=CARTESIAN_POINT('',(5.62607959275755,0.927460796501737,13.5));
#33828=CARTESIAN_POINT('',(5.62607959275755,0.927460796501737,11.5));
#33829=CARTESIAN_POINT('',(5.62607959275755,0.927460796501737,5.));
#33830=CARTESIAN_POINT('',(5.64992638765696,0.62445853820818,13.5));
#33831=CARTESIAN_POINT('',(5.64992638765696,0.62445853820818,13.5));
#33832=CARTESIAN_POINT('',(5.64992638765696,0.62445853820818,11.5));
#33833=CARTESIAN_POINT('',(5.64992638765696,0.62445853820818,11.5));
#33834=CARTESIAN_POINT('',(5.64992638765696,0.62445853820818,11.5));
#33835=CARTESIAN_POINT('Origin',(5.93134829123814,0.872302667016487,11.5));
#33836=CARTESIAN_POINT('',(6.22422999299742,0.974536253938444,11.5));
#33837=CARTESIAN_POINT('Origin',(6.,0.,11.5));
#33838=CARTESIAN_POINT('',(6.24807678789684,0.671533995644887,11.5));
#33839=CARTESIAN_POINT('',(6.24807678789684,0.671533995644887,11.5));
#33840=CARTESIAN_POINT('',(6.21277019481931,1.12014679582479,11.5));
#33841=CARTESIAN_POINT('Origin',(5.64992638765696,0.62445853820818,11.5));
#33842=CARTESIAN_POINT('',(6.24807678789684,0.671533995644887,13.5));
#33843=CARTESIAN_POINT('',(6.24807678789684,0.671533995644887,13.5));
#33844=CARTESIAN_POINT('',(6.24807678789684,0.671533995644887,11.5));
#33845=CARTESIAN_POINT('Origin',(6.24807678789684,0.671533995644887,11.5));
#33846=CARTESIAN_POINT('',(6.22422999299742,0.974536253938444,13.5));
#33847=CARTESIAN_POINT('',(6.22422999299742,0.974536253938444,5.));
#33848=CARTESIAN_POINT('',(6.21277019481931,1.12014679582479,13.5));
#33849=CARTESIAN_POINT('Origin',(5.93134829123814,0.872302667016487,13.5));
#33850=CARTESIAN_POINT('Origin',(6.,0.,13.5));
#33851=CARTESIAN_POINT('Origin',(6.,0.,11.));
#33852=CARTESIAN_POINT('',(4.8,-1.46957615897682E-16,11.));
#33853=CARTESIAN_POINT('Origin',(6.,0.,11.));
#33854=CARTESIAN_POINT('',(5.,-1.22464679914735E-16,11.));
#33855=CARTESIAN_POINT('Origin',(6.,0.,11.));
#33856=CARTESIAN_POINT('Origin',(6.,0.,9.2));
#33857=CARTESIAN_POINT('',(4.8,-1.46957615897682E-16,9.2));
#33858=CARTESIAN_POINT('Origin',(6.,0.,9.2));
#33859=CARTESIAN_POINT('',(5.,1.22464679914735E-16,9.2));
#33860=CARTESIAN_POINT('Origin',(6.,0.,9.2));
#33861=CARTESIAN_POINT('Origin',(6.,0.,9.2));
#33862=CARTESIAN_POINT('',(4.8,-1.46957615897682E-16,9.2));
#33863=CARTESIAN_POINT('Origin',(6.,0.,5.));
#33864=CARTESIAN_POINT('',(5.,-1.22464679914735E-16,5.));
#33865=CARTESIAN_POINT('',(5.,-1.22464679914735E-16,5.));
#33866=CARTESIAN_POINT('Origin',(6.,0.,5.));
#33867=CARTESIAN_POINT('Origin',(6.,0.,5.));
#33868=CARTESIAN_POINT('',(5.,-1.22464679914735E-16,15.));
#33869=CARTESIAN_POINT('Origin',(6.,0.,15.));
#33870=CARTESIAN_POINT('',(5.,-1.22464679914735E-16,5.));
#33871=CARTESIAN_POINT('Origin',(6.,0.,15.));
#33872=CARTESIAN_POINT('Origin',(6.,0.,5.));
#33873=CARTESIAN_POINT('',(0.,0.,0.));
#33874=CARTESIAN_POINT('Origin',(6.,0.,7.2));
#33875=CARTESIAN_POINT('',(4.995,-1.23077003314309E-16,7.8));
#33876=CARTESIAN_POINT('Origin',(6.,0.,7.8));
#33877=CARTESIAN_POINT('',(4.995,-1.23077003314309E-16,7.2));
#33878=CARTESIAN_POINT('',(4.995,-1.23077003314309E-16,7.2));
#33879=CARTESIAN_POINT('Origin',(6.,0.,7.2));
#33880=CARTESIAN_POINT('Origin',(6.,0.,7.2));
#33881=CARTESIAN_POINT('',(4.8,-1.46957615897682E-16,7.8));
#33882=CARTESIAN_POINT('Origin',(6.,0.,7.8));
#33883=CARTESIAN_POINT('',(4.8,-1.46957615897682E-16,7.2));
#33884=CARTESIAN_POINT('',(4.8,-1.46957615897682E-16,7.2));
#33885=CARTESIAN_POINT('Origin',(6.,0.,7.2));
#33886=CARTESIAN_POINT('Origin',(6.,0.,7.8));
#33887=CARTESIAN_POINT('Origin',(6.,0.,7.2));
#33888=CARTESIAN_POINT('',(0.,0.,0.));
#33889=CARTESIAN_POINT('Origin',(6.,0.,14.2));
#33890=CARTESIAN_POINT('',(4.995,-1.23077003314309E-16,15.));
#33891=CARTESIAN_POINT('Origin',(6.,0.,15.));
#33892=CARTESIAN_POINT('',(4.995,-1.23077003314309E-16,14.2));
#33893=CARTESIAN_POINT('',(4.995,-1.23077003314309E-16,14.2));
#33894=CARTESIAN_POINT('Origin',(6.,0.,14.2));
#33895=CARTESIAN_POINT('Origin',(6.,0.,14.2));
#33896=CARTESIAN_POINT('',(4.8,-1.46957615897682E-16,15.));
#33897=CARTESIAN_POINT('Origin',(6.,0.,15.));
#33898=CARTESIAN_POINT('',(4.8,-1.46957615897682E-16,14.2));
#33899=CARTESIAN_POINT('',(4.8,-1.46957615897682E-16,14.2));
#33900=CARTESIAN_POINT('Origin',(6.,0.,14.2));
#33901=CARTESIAN_POINT('Origin',(6.,0.,15.));
#33902=CARTESIAN_POINT('Origin',(6.,0.,14.2));
#33903=CARTESIAN_POINT('',(0.,0.,0.));
#33904=CARTESIAN_POINT('Origin',(6.99,0.,5.4));
#33905=CARTESIAN_POINT('',(6.9913626985115,0.165,5.4));
#33906=CARTESIAN_POINT('',(7.005,-1.18380595689425E-17,5.565));
#33907=CARTESIAN_POINT('Ctrl Pts',(6.9913626985115,0.165,5.4));
#33908=CARTESIAN_POINT('Ctrl Pts',(6.9913626985115,0.165,5.42075846165316));
#33909=CARTESIAN_POINT('Ctrl Pts',(6.99208213234536,0.160843707720237,5.44287436269219));
#33910=CARTESIAN_POINT('Ctrl Pts',(6.99466757507705,0.143993298000807,5.48351551009448));
#33911=CARTESIAN_POINT('Ctrl Pts',(6.9964948147884,0.131301190829395,5.50204404696217));
#33912=CARTESIAN_POINT('Ctrl Pts',(6.99991441892026,0.102044414577984,5.53130082321358));
#33913=CARTESIAN_POINT('Ctrl Pts',(7.00173085232892,0.083515719765581,5.54399321874371));
#33914=CARTESIAN_POINT('Ctrl Pts',(7.00429148829838,0.0428740302308134,
5.56084383788794));
#33915=CARTESIAN_POINT('Ctrl Pts',(7.005,0.0207579399932887,5.565));
#33916=CARTESIAN_POINT('Ctrl Pts',(7.005,2.60208521396521E-17,5.565));
#33917=CARTESIAN_POINT('Ctrl Pts',(7.005,-2.08166817117217E-17,5.565));
#33918=CARTESIAN_POINT('Ctrl Pts',(7.005,-0.0207579399932887,5.565));
#33919=CARTESIAN_POINT('Ctrl Pts',(7.00429148829838,-0.0428740302308134,
5.56084383788794));
#33920=CARTESIAN_POINT('Ctrl Pts',(7.00173085232892,-0.083515719765581,
5.54399321874371));
#33921=CARTESIAN_POINT('Ctrl Pts',(6.99991441892026,-0.102044414577984,
5.53130082321358));
#33922=CARTESIAN_POINT('Ctrl Pts',(6.9964948147884,-0.131301190829395,5.50204404696217));
#33923=CARTESIAN_POINT('Ctrl Pts',(6.99466757507705,-0.143993298000807,
5.48351551009448));
#33924=CARTESIAN_POINT('Ctrl Pts',(6.99208213234536,-0.160843707720237,
5.44287436269219));
#33925=CARTESIAN_POINT('Ctrl Pts',(6.9913626985115,-0.165,5.42075846165316));
#33926=CARTESIAN_POINT('Ctrl Pts',(6.9913626985115,-0.165,5.37924153834684));
#33927=CARTESIAN_POINT('Ctrl Pts',(6.99208213234536,-0.160843707720237,
5.35712563730781));
#33928=CARTESIAN_POINT('Ctrl Pts',(6.99466757507705,-0.143993298000807,
5.31648448990552));
#33929=CARTESIAN_POINT('Ctrl Pts',(6.9964948147884,-0.131301190829395,5.29795595303784));
#33930=CARTESIAN_POINT('Ctrl Pts',(6.99991441892026,-0.102044414577984,
5.26869917678642));
#33931=CARTESIAN_POINT('Ctrl Pts',(7.00173085232892,-0.083515719765581,
5.25600678125629));
#33932=CARTESIAN_POINT('Ctrl Pts',(7.00429148829838,-0.0428740302308134,
5.23915616211206));
#33933=CARTESIAN_POINT('Ctrl Pts',(7.005,-0.0207579399932887,5.235));
#33934=CARTESIAN_POINT('Ctrl Pts',(7.005,0.0207579399932886,5.235));
#33935=CARTESIAN_POINT('Ctrl Pts',(7.00429148829838,0.0428740302308133,
5.23915616211206));
#33936=CARTESIAN_POINT('Ctrl Pts',(7.00173085232892,0.0835157197655809,
5.25600678125629));
#33937=CARTESIAN_POINT('Ctrl Pts',(6.99991441892026,0.102044414577984,5.26869917678642));
#33938=CARTESIAN_POINT('Ctrl Pts',(6.9964948147884,0.131301190829395,5.29795595303784));
#33939=CARTESIAN_POINT('Ctrl Pts',(6.99466757507705,0.143993298000807,5.31648448990552));
#33940=CARTESIAN_POINT('Ctrl Pts',(6.99208213234536,0.160843707720237,5.35712563730781));
#33941=CARTESIAN_POINT('Ctrl Pts',(6.9913626985115,0.165,5.37924153834685));
#33942=CARTESIAN_POINT('Ctrl Pts',(6.9913626985115,0.165,5.4));
#33943=CARTESIAN_POINT('',(7.5,-2.02066721859313E-17,5.565));
#33944=CARTESIAN_POINT('',(6.99,-2.02066721859313E-17,5.565));
#33945=CARTESIAN_POINT('',(7.49089738077441,0.165,5.4));
#33946=CARTESIAN_POINT('Ctrl Pts',(7.49089738077441,0.165,5.4));
#33947=CARTESIAN_POINT('Ctrl Pts',(7.49089738077441,0.165,5.37926416089502));
#33948=CARTESIAN_POINT('Ctrl Pts',(7.49137458218466,0.160852499025072,5.35715772909914));
#33949=CARTESIAN_POINT('Ctrl Pts',(7.49309518705251,0.144008447160945,5.31651015506895));
#33950=CARTESIAN_POINT('Ctrl Pts',(7.49431341615514,0.131312810193433,5.29796757240187));
#33951=CARTESIAN_POINT('Ctrl Pts',(7.49659781052538,0.102032500700889,5.26868726290933));
#33952=CARTESIAN_POINT('Ctrl Pts',(7.49781281581157,0.0834898860986566,
5.25599156878035));
#33953=CARTESIAN_POINT('Ctrl Pts',(7.49952603771524,0.042842204593242,5.2391474746158));
#33954=CARTESIAN_POINT('Ctrl Pts',(7.5,0.0207357355648687,5.235));
#33955=CARTESIAN_POINT('Ctrl Pts',(7.5,-0.0207357355648687,5.235));
#33956=CARTESIAN_POINT('Ctrl Pts',(7.49952603771524,-0.042842204593242,
5.2391474746158));
#33957=CARTESIAN_POINT('Ctrl Pts',(7.49781281581157,-0.0834898860986566,
5.25599156878035));
#33958=CARTESIAN_POINT('Ctrl Pts',(7.49659781052538,-0.102032500700889,
5.26868726290933));
#33959=CARTESIAN_POINT('Ctrl Pts',(7.49431341615514,-0.131312810193433,
5.29796757240187));
#33960=CARTESIAN_POINT('Ctrl Pts',(7.49309518705251,-0.144008447160945,
5.31651015506895));
#33961=CARTESIAN_POINT('Ctrl Pts',(7.49137458218466,-0.160852499025072,
5.35715772909914));
#33962=CARTESIAN_POINT('Ctrl Pts',(7.49089738077441,-0.165,5.37926416089502));
#33963=CARTESIAN_POINT('Ctrl Pts',(7.49089738077441,-0.165,5.42073583910498));
#33964=CARTESIAN_POINT('Ctrl Pts',(7.49137458218466,-0.160852499025072,
5.44284227090086));
#33965=CARTESIAN_POINT('Ctrl Pts',(7.49309518705251,-0.144008447160945,
5.48348984493105));
#33966=CARTESIAN_POINT('Ctrl Pts',(7.49431341615514,-0.131312810193433,
5.50203242759813));
#33967=CARTESIAN_POINT('Ctrl Pts',(7.49659781052538,-0.102032500700889,
5.53131273709067));
#33968=CARTESIAN_POINT('Ctrl Pts',(7.49781281581157,-0.0834898860986566,
5.54400843121965));
#33969=CARTESIAN_POINT('Ctrl Pts',(7.49952603771524,-0.042842204593242,
5.5608525253842));
#33970=CARTESIAN_POINT('Ctrl Pts',(7.5,-0.0207357355648688,5.565));
#33971=CARTESIAN_POINT('Ctrl Pts',(7.5,-8.32667268468867E-17,5.565));
#33972=CARTESIAN_POINT('Ctrl Pts',(7.5,4.85722573273506E-17,5.565));
#33973=CARTESIAN_POINT('Ctrl Pts',(7.5,0.0207357355648687,5.565));
#33974=CARTESIAN_POINT('Ctrl Pts',(7.49952603771524,0.0428422045932419,
5.5608525253842));
#33975=CARTESIAN_POINT('Ctrl Pts',(7.49781281581157,0.0834898860986566,
5.54400843121965));
#33976=CARTESIAN_POINT('Ctrl Pts',(7.49659781052538,0.102032500700889,5.53131273709067));
#33977=CARTESIAN_POINT('Ctrl Pts',(7.49431341615514,0.131312810193433,5.50203242759813));
#33978=CARTESIAN_POINT('Ctrl Pts',(7.49309518705251,0.144008447160945,5.48348984493105));
#33979=CARTESIAN_POINT('Ctrl Pts',(7.49137458218466,0.160852499025072,5.44284227090086));
#33980=CARTESIAN_POINT('Ctrl Pts',(7.49089738077441,0.165,5.42073583910498));
#33981=CARTESIAN_POINT('Ctrl Pts',(7.49089738077441,0.165,5.4));
#33982=CARTESIAN_POINT('Origin',(6.,0.,5.));
#33983=CARTESIAN_POINT('',(4.995,-1.23077003314309E-16,5.8));
#33984=CARTESIAN_POINT('Origin',(6.,0.,5.8));
#33985=CARTESIAN_POINT('',(4.995,-1.23077003314309E-16,5.));
#33986=CARTESIAN_POINT('',(4.995,-1.23077003314309E-16,5.));
#33987=CARTESIAN_POINT('Origin',(6.,0.,5.));
#33988=CARTESIAN_POINT('Origin',(6.,0.,5.));
#33989=CARTESIAN_POINT('',(4.5,-1.83697019872103E-16,5.8));
#33990=CARTESIAN_POINT('Origin',(6.,0.,5.8));
#33991=CARTESIAN_POINT('',(4.5,-1.83697019872103E-16,5.));
#33992=CARTESIAN_POINT('',(4.5,-1.83697019872103E-16,5.));
#33993=CARTESIAN_POINT('Origin',(6.,0.,5.));
#33994=CARTESIAN_POINT('Origin',(6.,0.,5.8));
#33995=CARTESIAN_POINT('Origin',(6.,0.,5.));
#33996=CARTESIAN_POINT('',(0.,0.,0.));
#33997=CARTESIAN_POINT('Origin',(5.64992638765696,0.62445853820818,11.5));
#33998=CARTESIAN_POINT('',(6.24807678789684,0.671533995644887,11.5));
#33999=CARTESIAN_POINT('',(5.64992638765696,0.62445853820818,11.5));
#34000=CARTESIAN_POINT('',(6.24807678789684,0.671533995644887,11.5));
#34001=CARTESIAN_POINT('',(6.24807678789684,0.671533995644887,13.5));
#34002=CARTESIAN_POINT('',(6.24807678789684,0.671533995644887,11.5));
#34003=CARTESIAN_POINT('',(5.64992638765696,0.62445853820818,13.5));
#34004=CARTESIAN_POINT('',(6.24807678789684,0.671533995644887,13.5));
#34005=CARTESIAN_POINT('',(5.64992638765696,0.62445853820818,11.5));
#34006=CARTESIAN_POINT('Origin',(5.60285093022026,1.22260893844806,11.5));
#34007=CARTESIAN_POINT('',(5.60285093022026,1.22260893844806,11.5));
#34008=CARTESIAN_POINT('',(5.64992638765696,0.62445853820818,11.5));
#34009=CARTESIAN_POINT('',(5.60285093022026,1.22260893844806,13.5));
#34010=CARTESIAN_POINT('',(5.64992638765696,0.62445853820818,13.5));
#34011=CARTESIAN_POINT('',(5.60285093022026,1.22260893844806,11.5));
#34012=CARTESIAN_POINT('Origin',(6.20100133046013,1.26968439588476,11.5));
#34013=CARTESIAN_POINT('',(6.20100133046013,1.26968439588476,11.5));
#34014=CARTESIAN_POINT('',(5.60285093022026,1.22260893844806,11.5));
#34015=CARTESIAN_POINT('',(6.20100133046013,1.26968439588476,13.5));
#34016=CARTESIAN_POINT('',(5.60285093022026,1.22260893844806,13.5));
#34017=CARTESIAN_POINT('',(6.20100133046013,1.26968439588476,11.5));
#34018=CARTESIAN_POINT('Origin',(6.24807678789684,0.671533995644887,11.5));
#34019=CARTESIAN_POINT('',(6.20100133046013,1.26968439588476,11.5));
#34020=CARTESIAN_POINT('',(6.20100133046013,1.26968439588476,13.5));
#34021=CARTESIAN_POINT('Origin',(5.92546385905855,0.947071467046472,13.5));
#34022=CARTESIAN_POINT('Origin',(5.92546385905855,0.947071467046472,11.5));
#34023=CARTESIAN_POINT('',(0.,0.,0.));
#34024=CARTESIAN_POINT('Origin',(6.,0.,15.));
#34025=CARTESIAN_POINT('',(5.775,-2.75545529808154E-17,15.2));
#34026=CARTESIAN_POINT('Origin',(6.,0.,15.2));
#34027=CARTESIAN_POINT('',(5.775,-2.75545529808154E-17,15.));
#34028=CARTESIAN_POINT('',(5.775,-2.75545529808154E-17,15.));
#34029=CARTESIAN_POINT('Origin',(6.,0.,15.));
#34030=CARTESIAN_POINT('Origin',(6.,0.,15.));
#34031=CARTESIAN_POINT('',(4.7,-1.59204083889156E-16,15.2));
#34032=CARTESIAN_POINT('Origin',(6.,0.,15.2));
#34033=CARTESIAN_POINT('',(4.7,-1.59204083889156E-16,15.));
#34034=CARTESIAN_POINT('',(4.7,-1.59204083889156E-16,15.));
#34035=CARTESIAN_POINT('Origin',(6.,0.,15.));
#34036=CARTESIAN_POINT('Origin',(6.,0.,15.2));
#34037=CARTESIAN_POINT('Origin',(6.,0.,15.));
#34038=CARTESIAN_POINT('',(0.,0.,0.));
#34039=CARTESIAN_POINT('Origin',(0.,-0.4,0.));
#34040=CARTESIAN_POINT('',(-0.1954,-0.4,2.39295984553393E-17));
#34041=CARTESIAN_POINT('Origin',(0.,-0.4,0.));
#34042=CARTESIAN_POINT('Origin',(0.0577350269189626,0.,-0.1));
#34043=CARTESIAN_POINT('',(0.0577350269189626,0.,-0.1));
#34044=CARTESIAN_POINT('',(0.115470053837925,0.,0.));
#34045=CARTESIAN_POINT('',(0.0934187836487032,0.,-0.0381939203391614));
#34046=CARTESIAN_POINT('',(0.0577350269189626,-0.2,-0.1));
#34047=CARTESIAN_POINT('',(0.0577350269189626,0.,-0.1));
#34048=CARTESIAN_POINT('',(0.115470053837925,-0.2,0.));
#34049=CARTESIAN_POINT('',(0.115470053837925,-0.2,0.));
#34050=CARTESIAN_POINT('',(0.115470053837925,0.,0.));
#34051=CARTESIAN_POINT('Origin',(-0.0577350269189626,0.,-0.1));
#34052=CARTESIAN_POINT('',(-0.0577350269189626,0.,-0.1));
#34053=CARTESIAN_POINT('',(0.0561324865405187,0.,-0.1));
#34054=CARTESIAN_POINT('',(-0.0577350269189626,-0.2,-0.1));
#34055=CARTESIAN_POINT('',(-0.0577350269189626,0.,-0.1));
#34056=CARTESIAN_POINT('',(0.0577350269189626,-0.2,-0.1));
#34057=CARTESIAN_POINT('Origin',(-0.115470053837925,0.,-1.38777878078145E-17));
#34058=CARTESIAN_POINT('',(-0.115470053837925,0.,-1.41410031829988E-17));
#34059=CARTESIAN_POINT('',(-0.0797862971081845,0.,-0.0618060796608387));
#34060=CARTESIAN_POINT('',(-0.115470053837925,-0.2,-1.38777878078145E-17));
#34061=CARTESIAN_POINT('',(-0.115470053837925,0.,-1.41410031829988E-17));
#34062=CARTESIAN_POINT('',(-0.0577350269189626,-0.2,-0.1));
#34063=CARTESIAN_POINT('Origin',(-0.0577350269189626,0.,0.1));
#34064=CARTESIAN_POINT('',(-0.0577350269189626,0.,0.1));
#34065=CARTESIAN_POINT('',(-0.0509187836487033,0.,0.111806079660839));
#34066=CARTESIAN_POINT('',(-0.0577350269189626,-0.2,0.1));
#34067=CARTESIAN_POINT('',(-0.0577350269189626,0.,0.1));
#34068=CARTESIAN_POINT('',(-0.115470053837925,-0.2,-1.41410031829988E-17));
#34069=CARTESIAN_POINT('Origin',(0.0577350269189626,0.,0.1));
#34070=CARTESIAN_POINT('',(0.0577350269189626,0.,0.1));
#34071=CARTESIAN_POINT('',(0.113867513459481,0.,0.1));
#34072=CARTESIAN_POINT('',(0.0577350269189626,-0.2,0.1));
#34073=CARTESIAN_POINT('',(0.0577350269189626,0.,0.1));
#34074=CARTESIAN_POINT('',(-0.0577350269189626,-0.2,0.1));
#34075=CARTESIAN_POINT('Origin',(0.115470053837925,0.,0.));
#34076=CARTESIAN_POINT('',(0.122286297108185,0.,-0.0118060796608386));
#34077=CARTESIAN_POINT('',(0.0577350269189626,-0.2,0.1));
#34078=CARTESIAN_POINT('Origin',(0.,-0.2,0.));
#34079=CARTESIAN_POINT('Origin',(0.17,0.,0.));
#34080=CARTESIAN_POINT('',(-0.17,-8.67361737988404E-18,-2.0818995585505E-17));
#34081=CARTESIAN_POINT('Origin',(0.,0.,0.));
#34082=CARTESIAN_POINT('Origin',(0.,-0.015,0.));
#34083=CARTESIAN_POINT('',(-0.1954,-0.0254,-2.39295984553393E-17));
#34084=CARTESIAN_POINT('Origin',(0.,-0.0254,0.));
#34085=CARTESIAN_POINT('',(-0.185,-0.015,-2.2655965784226E-17));
#34086=CARTESIAN_POINT('Origin',(0.,-0.2775,0.));
#34087=CARTESIAN_POINT('',(-0.1954,-0.2775,-2.39295984553393E-17));
#34088=CARTESIAN_POINT('',(0.,0.,0.));
#34089=CARTESIAN_POINT('Origin',(0.299075200119938,0.,-0.0235377287183535));
#34090=CARTESIAN_POINT('',(0.198647557588297,2.2,-1.29959191589676));
#34091=CARTESIAN_POINT('',(0.224229992997422,2.2,-0.974536253938444));
#34092=CARTESIAN_POINT('',(0.299075200119938,2.2,-0.0235377287183535));
#34093=CARTESIAN_POINT('',(0.198647557588297,-1.,-1.29959191589676));
#34094=CARTESIAN_POINT('',(0.198647557588297,0.,-1.29959191589676));
#34095=CARTESIAN_POINT('',(0.224229992997422,-1.,-0.974536253938444));
#34096=CARTESIAN_POINT('',(0.299075200119938,-1.,-0.0235377287183535));
#34097=CARTESIAN_POINT('',(0.224229992997422,0.,-0.974536253938444));
#34098=CARTESIAN_POINT('Origin',(0.198647557588297,0.,-1.29959191589676));
#34099=CARTESIAN_POINT('',(-0.39950284265158,2.2,-1.25251645846005));
#34100=CARTESIAN_POINT('',(0.0491099575283277,2.2,-1.28782305153758));
#34101=CARTESIAN_POINT('',(-0.39950284265158,-1.,-1.25251645846005));
#34102=CARTESIAN_POINT('',(-0.39950284265158,0.,-1.25251645846005));
#34103=CARTESIAN_POINT('',(0.0491099575283277,-1.,-1.28782305153758));
#34104=CARTESIAN_POINT('Origin',(-0.39950284265158,0.,-1.25251645846005));
#34105=CARTESIAN_POINT('',(-0.373920407242454,2.2,-0.927460796501737));
#34106=CARTESIAN_POINT('',(-0.349289021385759,2.2,-0.614489364870848));
#34107=CARTESIAN_POINT('',(-0.373920407242454,-1.,-0.927460796501737));
#34108=CARTESIAN_POINT('',(-0.373920407242454,0.,-0.927460796501737));
#34109=CARTESIAN_POINT('',(-0.349289021385759,-1.,-0.614489364870848));
#34110=CARTESIAN_POINT('Origin',(0.,-1.,0.));
#34111=CARTESIAN_POINT('',(3.71701050416825,-1.,0.496319364827592));
#34112=CARTESIAN_POINT('',(3.68845817949618,-1.,0.676591647973661));
#34113=CARTESIAN_POINT('Origin',(0.,-1.,0.));
#34114=CARTESIAN_POINT('',(4.10104028313088,-1.,0.906349047628867));
#34115=CARTESIAN_POINT('Ctrl Pts',(3.68845817949618,-1.,0.676591647973661));
#34116=CARTESIAN_POINT('Ctrl Pts',(3.68850172300543,-1.,0.67656928609342));
#34117=CARTESIAN_POINT('Ctrl Pts',(3.68869596426099,-1.,0.676535079520366));
#34118=CARTESIAN_POINT('Ctrl Pts',(3.68934997767391,-1.,0.676580391119535));
#34119=CARTESIAN_POINT('Ctrl Pts',(3.6910107117555,-1.,0.676867042599712));
#34120=CARTESIAN_POINT('Ctrl Pts',(3.69443683573443,-1.,0.677621861865197));
#34121=CARTESIAN_POINT('Ctrl Pts',(3.69959004073192,-1.,0.67887882222639));
#34122=CARTESIAN_POINT('Ctrl Pts',(3.70595722032165,-1.,0.680526909711618));
#34123=CARTESIAN_POINT('Ctrl Pts',(3.71319182790334,-1.,0.68249234510969));
#34124=CARTESIAN_POINT('Ctrl Pts',(3.7209063713952,-1.,0.684691698168356));
#34125=CARTESIAN_POINT('Ctrl Pts',(3.72872973554125,-1.,0.687043475232499));
#34126=CARTESIAN_POINT('Ctrl Pts',(3.73636374474993,-1.,0.689479637354652));
#34127=CARTESIAN_POINT('Ctrl Pts',(3.74365508986548,-1.,0.691960080400503));
#34128=CARTESIAN_POINT('Ctrl Pts',(3.7506028824329,-1.,0.694474562581174));
#34129=CARTESIAN_POINT('Ctrl Pts',(3.75729775766913,-1.,0.69703124565953));
#34130=CARTESIAN_POINT('Ctrl Pts',(3.76387780603725,-1.,0.699648552230851));
#34131=CARTESIAN_POINT('Ctrl Pts',(3.77048141872904,-1.,0.702346356621614));
#34132=CARTESIAN_POINT('Ctrl Pts',(3.77719254217197,-1.,0.70513584799995));
#34133=CARTESIAN_POINT('Ctrl Pts',(3.78402183336678,-1.,0.7080158793756));
#34134=CARTESIAN_POINT('Ctrl Pts',(3.79093694007146,-1.,0.710978231689118));
#34135=CARTESIAN_POINT('Ctrl Pts',(3.79788100314994,-1.,0.714010733006678));
#34136=CARTESIAN_POINT('Ctrl Pts',(3.80479445759296,-1.,0.717100993669091));
#34137=CARTESIAN_POINT('Ctrl Pts',(3.81163885127309,-1.,0.720240466589173));
#34138=CARTESIAN_POINT('Ctrl Pts',(3.81840802610795,-1.,0.72342634601935));
#34139=CARTESIAN_POINT('Ctrl Pts',(3.82511495756682,-1.,0.726659281876608));
#34140=CARTESIAN_POINT('Ctrl Pts',(3.8317839240337,-1.,0.729942010490146));
#34141=CARTESIAN_POINT('Ctrl Pts',(3.83844103658016,-1.,0.733277703756091));
#34142=CARTESIAN_POINT('Ctrl Pts',(3.84510432881231,-1.,0.736668240497151));
#34143=CARTESIAN_POINT('Ctrl Pts',(3.85177770351237,-1.,0.740113146827177));
#34144=CARTESIAN_POINT('Ctrl Pts',(3.85845645217611,-1.,0.743610542737042));
#34145=CARTESIAN_POINT('Ctrl Pts',(3.86513062969896,-1.,0.747157716488884));
#34146=CARTESIAN_POINT('Ctrl Pts',(3.87178914078372,-1.,0.750751822383024));
#34147=CARTESIAN_POINT('Ctrl Pts',(3.87842382520058,-1.,0.754390577396847));
#34148=CARTESIAN_POINT('Ctrl Pts',(3.88503262662684,-1.,0.758072800564799));
#34149=CARTESIAN_POINT('Ctrl Pts',(3.89161738162245,-1.,0.761798028793978));
#34150=CARTESIAN_POINT('Ctrl Pts',(3.89818233104381,-1.,0.765566256401307));
#34151=CARTESIAN_POINT('Ctrl Pts',(3.90473237182634,-1.,0.769377629847877));
#34152=CARTESIAN_POINT('Ctrl Pts',(3.91127138115238,-1.,0.773232154506306));
#34153=CARTESIAN_POINT('Ctrl Pts',(3.91780062334464,-1.,0.777129415664915));
#34154=CARTESIAN_POINT('Ctrl Pts',(3.92431956510418,-1.,0.781068718228395));
#34155=CARTESIAN_POINT('Ctrl Pts',(3.93082655631768,-1.,0.785049202786459));
#34156=CARTESIAN_POINT('Ctrl Pts',(3.93731956885671,-1.,0.789069971469324));
#34157=CARTESIAN_POINT('Ctrl Pts',(3.94379688971307,-1.,0.793130205641017));
#34158=CARTESIAN_POINT('Ctrl Pts',(3.95025788827189,-1.,0.797229296085439));
#34159=CARTESIAN_POINT('Ctrl Pts',(3.95670276375176,-1.,0.801366797727206));
#34160=CARTESIAN_POINT('Ctrl Pts',(3.96313222295874,-1.,0.805542372178496));
#34161=CARTESIAN_POINT('Ctrl Pts',(3.96954717513251,-1.,0.809755732818134));
#34162=CARTESIAN_POINT('Ctrl Pts',(3.97594844078763,-1.,0.814006592328738));
#34163=CARTESIAN_POINT('Ctrl Pts',(3.98233640155287,-1.,0.818294599022034));
#34164=CARTESIAN_POINT('Ctrl Pts',(3.98871104646328,-1.,0.82261934602177));
#34165=CARTESIAN_POINT('Ctrl Pts',(3.99507212784289,-1.,0.826980400320474));
#34166=CARTESIAN_POINT('Ctrl Pts',(4.00141928477447,-1.,0.831377325741487));
#34167=CARTESIAN_POINT('Ctrl Pts',(4.00775216907934,-1.,0.835809705809822));
#34168=CARTESIAN_POINT('Ctrl Pts',(4.01407059766338,-1.,0.840277171976381));
#34169=CARTESIAN_POINT('Ctrl Pts',(4.02037456798787,-1.,0.844779403288517));
#34170=CARTESIAN_POINT('Ctrl Pts',(4.02666418343508,-1.,0.849316107475013));
#34171=CARTESIAN_POINT('Ctrl Pts',(4.03293960436945,-1.,0.853887006632179));
#34172=CARTESIAN_POINT('Ctrl Pts',(4.03920099284658,-1.,0.858491822322572));
#34173=CARTESIAN_POINT('Ctrl Pts',(4.04544845048097,-1.,0.863130256642174));
#34174=CARTESIAN_POINT('Ctrl Pts',(4.05168199437128,-1.,0.867801988858176));
#34175=CARTESIAN_POINT('Ctrl Pts',(4.05790159030495,-1.,0.872506694780564));
#34176=CARTESIAN_POINT('Ctrl Pts',(4.06410717232347,-1.,0.877244060484596));
#34177=CARTESIAN_POINT('Ctrl Pts',(4.07029866694292,-1.,0.882013797525917));
#34178=CARTESIAN_POINT('Ctrl Pts',(4.07647601774639,-1.,0.886815658360739));
#34179=CARTESIAN_POINT('Ctrl Pts',(4.08263920306651,-1.,0.891649447920402));
#34180=CARTESIAN_POINT('Ctrl Pts',(4.08878822249095,-1.,0.896515019236369));
#34181=CARTESIAN_POINT('Ctrl Pts',(4.09369611524319,-1.,0.900432820945976));
#34182=CARTESIAN_POINT('Ctrl Pts',(4.09737067247114,-1.,0.903385402444213));
#34183=CARTESIAN_POINT('Ctrl Pts',(4.09981755067956,-1.,0.905360112216302));
#34184=CARTESIAN_POINT('Ctrl Pts',(4.10104028313088,-1.,0.906349047628867));
#34185=CARTESIAN_POINT('',(4.06552750530042,-1.,1.05427041296137));
#34186=CARTESIAN_POINT('',(4.10104028313088,-1.,0.906349047628867));
#34187=CARTESIAN_POINT('',(3.59360648251073,-1.,1.07167739962028));
#34188=CARTESIAN_POINT('Ctrl Pts',(4.06552750530042,-1.,1.05427041296137));
#34189=CARTESIAN_POINT('Ctrl Pts',(4.06398907542249,-1.,1.05459645194823));
#34190=CARTESIAN_POINT('Ctrl Pts',(4.06091239149123,-1.,1.055245071776));
#34191=CARTESIAN_POINT('Ctrl Pts',(4.05629789307025,-1.,1.05620762707996));
#34192=CARTESIAN_POINT('Ctrl Pts',(4.05014628384869,-1.,1.05747027727959));
#34193=CARTESIAN_POINT('Ctrl Pts',(4.04245854427496,-1.,1.05901393666567));
#34194=CARTESIAN_POINT('Ctrl Pts',(4.03477261141553,-1.,1.06052284711857));
#34195=CARTESIAN_POINT('Ctrl Pts',(4.02708855235633,-1.,1.06199687787462));
#34196=CARTESIAN_POINT('Ctrl Pts',(4.01940647495943,-1.,1.06343586496236));
#34197=CARTESIAN_POINT('Ctrl Pts',(4.01172654187398,-1.,1.0648396134311));
#34198=CARTESIAN_POINT('Ctrl Pts',(4.00404894952579,-1.,1.06620789963606));
#34199=CARTESIAN_POINT('Ctrl Pts',(3.99637389920441,-1.,1.06754047381312));
#34200=CARTESIAN_POINT('Ctrl Pts',(3.98870156857412,-1.,1.06883706263942));
#34201=CARTESIAN_POINT('Ctrl Pts',(3.98103208801101,-1.,1.07009737257767));
#34202=CARTESIAN_POINT('Ctrl Pts',(3.9733655022223,-1.,1.07132109206164));
#34203=CARTESIAN_POINT('Ctrl Pts',(3.96570179322338,-1.,1.07250789943007));
#34204=CARTESIAN_POINT('Ctrl Pts',(3.95804094429373,-1.,1.07365747426491));
#34205=CARTESIAN_POINT('Ctrl Pts',(3.95038299600676,-1.,1.07476950921587));
#34206=CARTESIAN_POINT('Ctrl Pts',(3.94272809633331,-1.,1.07584371946443));
#34207=CARTESIAN_POINT('Ctrl Pts',(3.93507657572883,-1.,1.07687985975384));
#34208=CARTESIAN_POINT('Ctrl Pts',(3.9274289334984,-1.,1.07787771707195));
#34209=CARTESIAN_POINT('Ctrl Pts',(3.91978568924178,-1.,1.07883706663554));
#34210=CARTESIAN_POINT('Ctrl Pts',(3.91214726022143,-1.,1.07975763507473));
#34211=CARTESIAN_POINT('Ctrl Pts',(3.90451384092545,-1.,1.08063906483818));
#34212=CARTESIAN_POINT('Ctrl Pts',(3.8968852509835,-1.,1.08148086931358));
#34213=CARTESIAN_POINT('Ctrl Pts',(3.88926088975114,-1.,1.08228241999346));
#34214=CARTESIAN_POINT('Ctrl Pts',(3.88164007721312,-1.,1.08304304871029));
#34215=CARTESIAN_POINT('Ctrl Pts',(3.8740223372254,-1.,1.08376213307504));
#34216=CARTESIAN_POINT('Ctrl Pts',(3.86640769434274,-1.,1.08443918607927));
#34217=CARTESIAN_POINT('Ctrl Pts',(3.85879698702532,-1.,1.08507395120059));
#34218=CARTESIAN_POINT('Ctrl Pts',(3.85119211322755,-1.,1.08566647671844));
#34219=CARTESIAN_POINT('Ctrl Pts',(3.8435952876495,-1.,1.08621688337604));
#34220=CARTESIAN_POINT('Ctrl Pts',(3.83600837071708,-1.,1.08672515456902));
#34221=CARTESIAN_POINT('Ctrl Pts',(3.82843215316984,-1.,1.08719091307558));
#34222=CARTESIAN_POINT('Ctrl Pts',(3.82086569676319,-1.,1.08761321539442));
#34223=CARTESIAN_POINT('Ctrl Pts',(3.81330554446323,-1.,1.08799030610862));
#34224=CARTESIAN_POINT('Ctrl Pts',(3.8057472665766,-1.,1.0883200925538));
#34225=CARTESIAN_POINT('Ctrl Pts',(3.79818708705259,-1.,1.08860064435778));
#34226=CARTESIAN_POINT('Ctrl Pts',(3.79062357974404,-1.,1.08883071512098));
#34227=CARTESIAN_POINT('Ctrl Pts',(3.78305911299504,-1.,1.08901018614636));
#34228=CARTESIAN_POINT('Ctrl Pts',(3.77550199409424,-1.,1.0891407279127));
#34229=CARTESIAN_POINT('Ctrl Pts',(3.76796340094448,-1.,1.08922484204256));
#34230=CARTESIAN_POINT('Ctrl Pts',(3.76045342580208,-1.,1.08926462734282));
#34231=CARTESIAN_POINT('Ctrl Pts',(3.75297711748132,-1.,1.08926054632925));
#34232=CARTESIAN_POINT('Ctrl Pts',(3.74553121371757,-1.,1.08921040494017));
#34233=CARTESIAN_POINT('Ctrl Pts',(3.73809879348239,-1.,1.08910769013298));
#34234=CARTESIAN_POINT('Ctrl Pts',(3.73065515162988,-1.,1.08894337390937));
#34235=CARTESIAN_POINT('Ctrl Pts',(3.72317741369398,-1.,1.08870887220082));
#34236=CARTESIAN_POINT('Ctrl Pts',(3.71565372339075,-1.,1.0883988733478));
#34237=CARTESIAN_POINT('Ctrl Pts',(3.70809084139457,-1.,1.08801367312185));
#34238=CARTESIAN_POINT('Ctrl Pts',(3.70052690909833,-1.,1.08756311291309));
#34239=CARTESIAN_POINT('Ctrl Pts',(3.69302062410157,-1.,1.08706319540271));
#34240=CARTESIAN_POINT('Ctrl Pts',(3.68562817420797,-1.,1.0865288888259));
#34241=CARTESIAN_POINT('Ctrl Pts',(3.67838211685117,-1.,1.0859675575576));
#34242=CARTESIAN_POINT('Ctrl Pts',(3.67127347729666,-1.,1.0853733414449));
#34243=CARTESIAN_POINT('Ctrl Pts',(3.66422237895365,-1.,1.08471809922901));
#34244=CARTESIAN_POINT('Ctrl Pts',(3.65709649161166,-1.,1.08395671077807));
#34245=CARTESIAN_POINT('Ctrl Pts',(3.64976441208358,-1.,1.08304289898623));
#34246=CARTESIAN_POINT('Ctrl Pts',(3.64214167843677,-1.,1.08194278850996));
#34247=CARTESIAN_POINT('Ctrl Pts',(3.63423373196529,-1.,1.08064765719867));
#34248=CARTESIAN_POINT('Ctrl Pts',(3.62619537902361,-1.,1.07919137290742));
#34249=CARTESIAN_POINT('Ctrl Pts',(3.61832318504574,-1.,1.07764868137619));
#34250=CARTESIAN_POINT('Ctrl Pts',(3.61098481349204,-1.,1.07611545402734));
#34251=CARTESIAN_POINT('Ctrl Pts',(3.60456339887778,-1.,1.07469327168578));
#34252=CARTESIAN_POINT('Ctrl Pts',(3.59940121154535,-1.,1.07347372545714));
#34253=CARTESIAN_POINT('Ctrl Pts',(3.59600583194946,-1.,1.07259084660936));
#34254=CARTESIAN_POINT('Ctrl Pts',(3.59439596999862,-1.,1.07209229745229));
#34255=CARTESIAN_POINT('Ctrl Pts',(3.59379266874567,-1.,1.07183575450617));
#34256=CARTESIAN_POINT('Ctrl Pts',(3.5936351279798,-1.,1.07171709254135));
#34257=CARTESIAN_POINT('Ctrl Pts',(3.59360648251073,-1.,1.07167739962028));
#34258=CARTESIAN_POINT('',(3.5372048861597,-1.,1.24526366418038));
#34259=CARTESIAN_POINT('Origin',(0.,-1.,0.));
#34260=CARTESIAN_POINT('',(3.90876544355381,-1.,1.53673442965256));
#34261=CARTESIAN_POINT('Ctrl Pts',(3.5372048861597,-1.,1.24526366418038));
#34262=CARTESIAN_POINT('Ctrl Pts',(3.53725139174486,-1.,1.24524838931757));
#34263=CARTESIAN_POINT('Ctrl Pts',(3.5374485926552,-1.,1.2452449899111));
#34264=CARTESIAN_POINT('Ctrl Pts',(3.53808746578196,-1.,1.24539205388767));
#34265=CARTESIAN_POINT('Ctrl Pts',(3.53968291130022,-1.,1.24593497226008));
#34266=CARTESIAN_POINT('Ctrl Pts',(3.54294877425964,-1.,1.24721646231966));
#34267=CARTESIAN_POINT('Ctrl Pts',(3.54784190283068,-1.,1.24926408628003));
#34268=CARTESIAN_POINT('Ctrl Pts',(3.55387287418985,-1.,1.2518879294064));
#34269=CARTESIAN_POINT('Ctrl Pts',(3.56071094991199,-1.,1.25496090900009));
#34270=CARTESIAN_POINT('Ctrl Pts',(3.56798645995275,-1.,1.25834000485716));
#34271=CARTESIAN_POINT('Ctrl Pts',(3.5753456065171,-1.,1.2618866714281));
#34272=CARTESIAN_POINT('Ctrl Pts',(3.58250452868618,-1.,1.26548706249862));
#34273=CARTESIAN_POINT('Ctrl Pts',(3.58931807846313,-1.,1.26907758484709));
#34274=CARTESIAN_POINT('Ctrl Pts',(3.59578698050006,-1.,1.27264798379307));
#34275=CARTESIAN_POINT('Ctrl Pts',(3.60199947736298,-1.,1.27622049908625));
#34276=CARTESIAN_POINT('Ctrl Pts',(3.60808907746339,-1.,1.27983492861691));
#34277=CARTESIAN_POINT('Ctrl Pts',(3.61418935913823,-1.,1.28353255117765));
#34278=CARTESIAN_POINT('Ctrl Pts',(3.6203814849236,-1.,1.28733755029384));
#34279=CARTESIAN_POINT('Ctrl Pts',(3.62667616004369,-1.,1.29125046021878));
#34280=CARTESIAN_POINT('Ctrl Pts',(3.63304271631046,-1.,1.29525810207762));
#34281=CARTESIAN_POINT('Ctrl Pts',(3.63942689872808,-1.,1.2993395590647));
#34282=CARTESIAN_POINT('Ctrl Pts',(3.64577181380113,-1.,1.30347327603774));
#34283=CARTESIAN_POINT('Ctrl Pts',(3.65204081987068,-1.,1.30764479590039));
#34284=CARTESIAN_POINT('Ctrl Pts',(3.65822827358617,-1.,1.31185038411218));
#34285=CARTESIAN_POINT('Ctrl Pts',(3.66434688899793,-1.,1.31609271239911));
#34286=CARTESIAN_POINT('Ctrl Pts',(3.67042021752656,-1.,1.32037828137766));
#34287=CARTESIAN_POINT('Ctrl Pts',(3.67647355257912,-1.,1.32471430856415));
#34288=CARTESIAN_POINT('Ctrl Pts',(3.68252441182551,-1.,1.3291054707274));
#34289=CARTESIAN_POINT('Ctrl Pts',(3.68857672413033,-1.,1.33355191034523));
#34290=CARTESIAN_POINT('Ctrl Pts',(3.69462613305708,-1.,1.3380510339822));
#34291=CARTESIAN_POINT('Ctrl Pts',(3.70066324015119,-1.,1.34259860752933));
#34292=CARTESIAN_POINT('Ctrl Pts',(3.70667753188248,-1.,1.34719008463534));
#34293=CARTESIAN_POINT('Ctrl Pts',(3.71266130563054,-1.,1.35182193384424));
#34294=CARTESIAN_POINT('Ctrl Pts',(3.71861271513313,-1.,1.35649266705037));
#34295=CARTESIAN_POINT('Ctrl Pts',(3.72453364678279,-1.,1.36120211416354));
#34296=CARTESIAN_POINT('Ctrl Pts',(3.73042829011295,-1.,1.36595093298676));
#34297=CARTESIAN_POINT('Ctrl Pts',(3.7363014588581,-1.,1.37074003422739));
#34298=CARTESIAN_POINT('Ctrl Pts',(3.74215698162555,-1.,1.37557002971687));
#34299=CARTESIAN_POINT('Ctrl Pts',(3.74799617204729,-1.,1.38044070763295));
#34300=CARTESIAN_POINT('Ctrl Pts',(3.75381861212707,-1.,1.38535129801176));
#34301=CARTESIAN_POINT('Ctrl Pts',(3.75962280650855,-1.,1.39030069388918));
#34302=CARTESIAN_POINT('Ctrl Pts',(3.76540689249074,-1.,1.39528769118052));
#34303=CARTESIAN_POINT('Ctrl Pts',(3.77116930621827,-1.,1.40031121335505));
#34304=CARTESIAN_POINT('Ctrl Pts',(3.77690952014259,-1.,1.40537056004722));
#34305=CARTESIAN_POINT('Ctrl Pts',(3.78262780065471,-1.,1.41046532282593));
#34306=CARTESIAN_POINT('Ctrl Pts',(3.78832489879426,-1.,1.4155952780383));
#34307=CARTESIAN_POINT('Ctrl Pts',(3.79400175744408,-1.,1.42076028482836));
#34308=CARTESIAN_POINT('Ctrl Pts',(3.7996592319632,-1.,1.42596018777283));
#34309=CARTESIAN_POINT('Ctrl Pts',(3.80529775429805,-1.,1.4311946992132));
#34310=CARTESIAN_POINT('Ctrl Pts',(3.81091737726815,-1.,1.43646341556724));
#34311=CARTESIAN_POINT('Ctrl Pts',(3.81651792398414,-1.,1.44176587041347));
#34312=CARTESIAN_POINT('Ctrl Pts',(3.82209910620533,-1.,1.44710157648539));
#34313=CARTESIAN_POINT('Ctrl Pts',(3.82766064519074,-1.,1.45247006796836));
#34314=CARTESIAN_POINT('Ctrl Pts',(3.83320241775423,-1.,1.45787095220852));
#34315=CARTESIAN_POINT('Ctrl Pts',(3.83872447159639,-1.,1.46330391180752));
#34316=CARTESIAN_POINT('Ctrl Pts',(3.84422695454796,-1.,1.46876867426504));
#34317=CARTESIAN_POINT('Ctrl Pts',(3.84971006847277,-1.,1.47426499018538));
#34318=CARTESIAN_POINT('Ctrl Pts',(3.85517401698843,-1.,1.4797926099102));
#34319=CARTESIAN_POINT('Ctrl Pts',(3.86061894706087,-1.,1.48535125509919));
#34320=CARTESIAN_POINT('Ctrl Pts',(3.86604492575189,-1.,1.4909406116431));
#34321=CARTESIAN_POINT('Ctrl Pts',(3.87145196998465,-1.,1.49656035399122));
#34322=CARTESIAN_POINT('Ctrl Pts',(3.87684006372134,-1.,1.50221016176556));
#34323=CARTESIAN_POINT('Ctrl Pts',(3.88220917950538,-1.,1.50788973857757));
#34324=CARTESIAN_POINT('Ctrl Pts',(3.88755930033884,-1.,1.51359883110559));
#34325=CARTESIAN_POINT('Ctrl Pts',(3.89289043533657,-1.,1.51933724329306));
#34326=CARTESIAN_POINT('Ctrl Pts',(3.89820260708225,-1.,1.52510482991635));
#34327=CARTESIAN_POINT('Ctrl Pts',(3.90243719631596,-1.,1.52974216056287));
#34328=CARTESIAN_POINT('Ctrl Pts',(3.90560462813969,-1.,1.53323321827755));
#34329=CARTESIAN_POINT('Ctrl Pts',(3.90771246855019,-1.,1.53556639217905));
#34330=CARTESIAN_POINT('Ctrl Pts',(3.90876544355381,-1.,1.53673442965256));
#34331=CARTESIAN_POINT('',(3.85054988729471,-1.,1.67727921511438));
#34332=CARTESIAN_POINT('',(3.90876544355381,-1.,1.53673442965256));
#34333=CARTESIAN_POINT('',(3.38171594275765,-1.,1.62064718014094));
#34334=CARTESIAN_POINT('Ctrl Pts',(3.85054988729471,-1.,1.67727921511438));
#34335=CARTESIAN_POINT('Ctrl Pts',(3.84897939430696,-1.,1.67736057656533));
#34336=CARTESIAN_POINT('Ctrl Pts',(3.84583912296459,-1.,1.6775199114018));
#34337=CARTESIAN_POINT('Ctrl Pts',(3.84113085985244,-1.,1.67774874946079));
#34338=CARTESIAN_POINT('Ctrl Pts',(3.83485746513989,-1.,1.67803353064351));
#34339=CARTESIAN_POINT('Ctrl Pts',(3.82702289286713,-1.,1.6783555575934));
#34340=CARTESIAN_POINT('Ctrl Pts',(3.81919554099578,-1.,1.67864354605954));
#34341=CARTESIAN_POINT('Ctrl Pts',(3.81137549624178,-1.,1.6788973773827));
#34342=CARTESIAN_POINT('Ctrl Pts',(3.80356289079005,-1.,1.67911690648355));
#34343=CARTESIAN_POINT('Ctrl Pts',(3.79575791578424,-1.,1.67930196625548));
#34344=CARTESIAN_POINT('Ctrl Pts',(3.7879608002176,-1.,1.67945236653493));
#34345=CARTESIAN_POINT('Ctrl Pts',(3.78017178197317,-1.,1.67956789212141));
#34346=CARTESIAN_POINT('Ctrl Pts',(3.77239107928502,-1.,1.67964830084993));
#34347=CARTESIAN_POINT('Ctrl Pts',(3.76461886684344,-1.,1.67969332319245));
#34348=CARTESIAN_POINT('Ctrl Pts',(3.75685523754493,-1.,1.67970265841239));
#34349=CARTESIAN_POINT('Ctrl Pts',(3.7491002239452,-1.,1.67967598599525));
#34350=CARTESIAN_POINT('Ctrl Pts',(3.74135385965401,-1.,1.6796129868522));
#34351=CARTESIAN_POINT('Ctrl Pts',(3.73361623282543,-1.,1.67951336376402));
#34352=CARTESIAN_POINT('Ctrl Pts',(3.72588753416396,-1.,1.67937685856652));
#34353=CARTESIAN_POINT('Ctrl Pts',(3.71816812842322,-1.,1.67920328071708));
#34354=CARTESIAN_POINT('Ctrl Pts',(3.71045854208343,-1.,1.67899249793462));
#34355=CARTESIAN_POINT('Ctrl Pts',(3.70275932351108,-1.,1.67874436948667));
#34356=CARTESIAN_POINT('Ctrl Pts',(3.6950709275959,-1.,1.67845869064323));
#34357=CARTESIAN_POINT('Ctrl Pts',(3.68739360236487,-1.,1.67813513867965));
#34358=CARTESIAN_POINT('Ctrl Pts',(3.67972724579124,-1.,1.67777320475848));
#34359=CARTESIAN_POINT('Ctrl Pts',(3.67207136294575,-1.,1.67737217414874));
#34360=CARTESIAN_POINT('Ctrl Pts',(3.66442538670968,-1.,1.67693128053132));
#34361=CARTESIAN_POINT('Ctrl Pts',(3.6567889441642,-1.,1.6764498346945));
#34362=CARTESIAN_POINT('Ctrl Pts',(3.64916213574667,-1.,1.67592735946692));
#34363=CARTESIAN_POINT('Ctrl Pts',(3.6415458297234,-1.,1.67536373264848));
#34364=CARTESIAN_POINT('Ctrl Pts',(3.63394189312924,-1.,1.67475929882971));
#34365=CARTESIAN_POINT('Ctrl Pts',(3.62635249450923,-1.,1.67411452372271));
#34366=CARTESIAN_POINT('Ctrl Pts',(3.61877947398184,-1.,1.67342968196224));
#34367=CARTESIAN_POINT('Ctrl Pts',(3.61122367156181,-1.,1.67270452466968));
#34368=CARTESIAN_POINT('Ctrl Pts',(3.603684308152,-1.,1.67193797318597));
#34369=CARTESIAN_POINT('Ctrl Pts',(3.59615824388807,-1.,1.67112775290707));
#34370=CARTESIAN_POINT('Ctrl Pts',(3.58864143097834,-1.,1.67027110397604));
#34371=CARTESIAN_POINT('Ctrl Pts',(3.58113044183829,-1.,1.66936552908232));
#34372=CARTESIAN_POINT('Ctrl Pts',(3.57362406285887,-1.,1.668409574073));
#34373=CARTESIAN_POINT('Ctrl Pts',(3.56612465179422,-1.,1.66740349220305));
#34374=CARTESIAN_POINT('Ctrl Pts',(3.55864015233602,-1.,1.66635023293114));
#34375=CARTESIAN_POINT('Ctrl Pts',(3.55118121342861,-1.,1.66525401568994));
#34376=CARTESIAN_POINT('Ctrl Pts',(3.54375747475014,-1.,1.66411849222326));
#34377=CARTESIAN_POINT('Ctrl Pts',(3.5363738506022,-1.,1.66294490916111));
#34378=CARTESIAN_POINT('Ctrl Pts',(3.52902746211093,-1.,1.66173058912371));
#34379=CARTESIAN_POINT('Ctrl Pts',(3.52170261543815,-1.,1.66046645222279));
#34380=CARTESIAN_POINT('Ctrl Pts',(3.5143763218894,-1.,1.65913971687342));
#34381=CARTESIAN_POINT('Ctrl Pts',(3.50702733146542,-1.,1.65773832633632));
#34382=CARTESIAN_POINT('Ctrl Pts',(3.4996447647794,-1.,1.65625517961588));
#34383=CARTESIAN_POINT('Ctrl Pts',(3.49223525300176,-1.,1.65469162644468));
#34384=CARTESIAN_POINT('Ctrl Pts',(3.48483492840894,-1.,1.65306335367739));
#34385=CARTESIAN_POINT('Ctrl Pts',(3.47749926256476,-1.,1.65139534930322));
#34386=CARTESIAN_POINT('Ctrl Pts',(3.47028140995992,-1.,1.64971118698256));
#34387=CARTESIAN_POINT('Ctrl Pts',(3.46321237515,-1.,1.64802323352738));
#34388=CARTESIAN_POINT('Ctrl Pts',(3.45628421062422,-1.,1.64632429697521));
#34389=CARTESIAN_POINT('Ctrl Pts',(3.44942242546795,-1.,1.64457408708107));
#34390=CARTESIAN_POINT('Ctrl Pts',(3.44250337701888,-1.,1.64270733821113));
#34391=CARTESIAN_POINT('Ctrl Pts',(3.43540451921548,-1.,1.64065778702023));
#34392=CARTESIAN_POINT('Ctrl Pts',(3.42804772926291,-1.,1.63837876246926));
#34393=CARTESIAN_POINT('Ctrl Pts',(3.42043974590882,-1.,1.63586250099773));
#34394=CARTESIAN_POINT('Ctrl Pts',(3.41272817148478,-1.,1.63316667054044));
#34395=CARTESIAN_POINT('Ctrl Pts',(3.40519422740235,-1.,1.63041148964828));
#34396=CARTESIAN_POINT('Ctrl Pts',(3.39818605297991,-1.,1.62774916464408));
#34397=CARTESIAN_POINT('Ctrl Pts',(3.39206617496906,-1.,1.62533996116713));
#34398=CARTESIAN_POINT('Ctrl Pts',(3.38715832179072,-1.,1.6233278855625));
#34399=CARTESIAN_POINT('Ctrl Pts',(3.38394285763222,-1.,1.62192472202769));
#34400=CARTESIAN_POINT('Ctrl Pts',(3.38243080602408,-1.,1.62118047294498));
#34401=CARTESIAN_POINT('Ctrl Pts',(3.38187506456922,-1.,1.62083271135947));
#34402=CARTESIAN_POINT('Ctrl Pts',(3.38173802621259,-1.,1.62069086551492));
#34403=CARTESIAN_POINT('Ctrl Pts',(3.38171594275764,-1.,1.62064718014094));
#34404=CARTESIAN_POINT('',(3.29885386921599,-1.,1.78327315618183));
#34405=CARTESIAN_POINT('Origin',(0.,-1.,0.));
#34406=CARTESIAN_POINT('',(3.62024382630768,-1.,2.12928030988903));
#34407=CARTESIAN_POINT('Ctrl Pts',(3.29885386921599,-1.,1.78327315618183));
#34408=CARTESIAN_POINT('Ctrl Pts',(3.29890219175522,-1.,1.78326534445426));
#34409=CARTESIAN_POINT('Ctrl Pts',(3.29909749657945,-1.,1.78329283591903));
#34410=CARTESIAN_POINT('Ctrl Pts',(3.29970549824336,-1.,1.78353803106983));
#34411=CARTESIAN_POINT('Ctrl Pts',(3.30119637003466,-1.,1.7843238478823));
#34412=CARTESIAN_POINT('Ctrl Pts',(3.30422155558973,-1.,1.78610045419769));
#34413=CARTESIAN_POINT('Ctrl Pts',(3.30873412266954,-1.,1.78888832245965));
#34414=CARTESIAN_POINT('Ctrl Pts',(3.31428038326763,-1.,1.79242331350137));
#34415=CARTESIAN_POINT('Ctrl Pts',(3.32055355101168,-1.,1.79652817033444));
#34416=CARTESIAN_POINT('Ctrl Pts',(3.3272108803981,-1.,1.80100380443535));
#34417=CARTESIAN_POINT('Ctrl Pts',(3.33392460276874,-1.,1.80565802981139));
#34418=CARTESIAN_POINT('Ctrl Pts',(3.34043216147532,-1.,1.81033399625311));
#34419=CARTESIAN_POINT('Ctrl Pts',(3.34660014370527,-1.,1.81494618732772));
#34420=CARTESIAN_POINT('Ctrl Pts',(3.35243086937451,-1.,1.81948458796748));
#34421=CARTESIAN_POINT('Ctrl Pts',(3.35800801557326,-1.,1.82398496829247));
#34422=CARTESIAN_POINT('Ctrl Pts',(3.36345722124127,-1.,1.82850752153182));
#34423=CARTESIAN_POINT('Ctrl Pts',(3.36890396271864,-1.,1.83311391452338));
#34424=CARTESIAN_POINT('Ctrl Pts',(3.37442462015914,-1.,1.83784072967111));
#34425=CARTESIAN_POINT('Ctrl Pts',(3.38002968341222,-1.,1.84269016931679));
#34426=CARTESIAN_POINT('Ctrl Pts',(3.38569092349639,-1.,1.84764441927778));
#34427=CARTESIAN_POINT('Ctrl Pts',(3.39135802549415,-1.,1.85267433291778));
#34428=CARTESIAN_POINT('Ctrl Pts',(3.39697816833056,-1.,1.85774972037055));
#34429=CARTESIAN_POINT('Ctrl Pts',(3.40251742305445,-1.,1.86285057051228));
#34430=CARTESIAN_POINT('Ctrl Pts',(3.40797080000513,-1.,1.86797231196635));
#34431=CARTESIAN_POINT('Ctrl Pts',(3.41335043875182,-1.,1.87311957248106));
#34432=CARTESIAN_POINT('Ctrl Pts',(3.4186785838376,-1.,1.87830245689338));
#34433=CARTESIAN_POINT('Ctrl Pts',(3.42397908819741,-1.,1.88353205062063));
#34434=CARTESIAN_POINT('Ctrl Pts',(3.42926852222174,-1.,1.88881571322018));
#34435=CARTESIAN_POINT('Ctrl Pts',(3.43455074411591,-1.,1.89415420002553));
#34436=CARTESIAN_POINT('Ctrl Pts',(3.43982185678105,-1.,1.89954426803392));
#34437=CARTESIAN_POINT('Ctrl Pts',(3.44507323983374,-1.,1.90498026502308));
#34438=CARTESIAN_POINT('Ctrl Pts',(3.45029522038885,-1.,1.91045605593638));
#34439=CARTESIAN_POINT('Ctrl Pts',(3.45548074309943,-1.,1.9159669478406));
#34440=CARTESIAN_POINT('Ctrl Pts',(3.4606282172248,-1.,1.9215111821321));
#34441=CARTESIAN_POINT('Ctrl Pts',(3.46573953254084,-1.,1.92708888591159));
#34442=CARTESIAN_POINT('Ctrl Pts',(3.47081872409783,-1.,1.93270136427083));
#34443=CARTESIAN_POINT('Ctrl Pts',(3.47587040389916,-1.,1.93835026973888));
#34444=CARTESIAN_POINT('Ctrl Pts',(3.48089825770411,-1.,1.94403680554062));
#34445=CARTESIAN_POINT('Ctrl Pts',(3.485903616108,-1.,1.94976096795902));
#34446=CARTESIAN_POINT('Ctrl Pts',(3.49088618670967,-1.,1.95552193112071));
#34447=CARTESIAN_POINT('Ctrl Pts',(3.49584466573045,-1.,1.96131836776489));
#34448=CARTESIAN_POINT('Ctrl Pts',(3.50077740176262,-1.,1.9671487972405));
#34449=CARTESIAN_POINT('Ctrl Pts',(3.505683018611,-1.,1.9730119116298));
#34450=CARTESIAN_POINT('Ctrl Pts',(3.51056110478334,-1.,1.97890693666316));
#34451=CARTESIAN_POINT('Ctrl Pts',(3.51541198728362,-1.,1.98483351061066));
#34452=CARTESIAN_POINT('Ctrl Pts',(3.52023644289195,-1.,1.99079153006143));
#34453=CARTESIAN_POINT('Ctrl Pts',(3.52503542491745,-1.,1.99678100339306));
#34454=CARTESIAN_POINT('Ctrl Pts',(3.52980980250181,-1.,2.00280191090341));
#34455=CARTESIAN_POINT('Ctrl Pts',(3.53456004727321,-1.,2.00885403604685));
#34456=CARTESIAN_POINT('Ctrl Pts',(3.53928627453503,-1.,2.0149369884727));
#34457=CARTESIAN_POINT('Ctrl Pts',(3.54398838254011,-1.,2.0210502798303));
#34458=CARTESIAN_POINT('Ctrl Pts',(3.54866616282173,-1.,2.02719338376144));
#34459=CARTESIAN_POINT('Ctrl Pts',(3.55331941294018,-1.,2.03336579658174));
#34460=CARTESIAN_POINT('Ctrl Pts',(3.55794807265052,-1.,2.03956711120099));
#34461=CARTESIAN_POINT('Ctrl Pts',(3.5625522387181,-1.,2.04579702159056));
#34462=CARTESIAN_POINT('Ctrl Pts',(3.56713209978207,-1.,2.05205528173091));
#34463=CARTESIAN_POINT('Ctrl Pts',(3.57168789423507,-1.,2.05834167687524));
#34464=CARTESIAN_POINT('Ctrl Pts',(3.576219862243,-1.,2.06465599229174));
#34465=CARTESIAN_POINT('Ctrl Pts',(3.58072819250442,-1.,2.07099797605747));
#34466=CARTESIAN_POINT('Ctrl Pts',(3.58521300039299,-1.,2.07736732842117));
#34467=CARTESIAN_POINT('Ctrl Pts',(3.58967435355088,-1.,2.08376373048756));
#34468=CARTESIAN_POINT('Ctrl Pts',(3.59411228625588,-1.,2.09018686331416));
#34469=CARTESIAN_POINT('Ctrl Pts',(3.59852681775485,-1.,2.09663642986631));
#34470=CARTESIAN_POINT('Ctrl Pts',(3.60291797088734,-1.,2.1031121772821));
#34471=CARTESIAN_POINT('Ctrl Pts',(3.60728578532601,-1.,2.10961391334462));
#34472=CARTESIAN_POINT('Ctrl Pts',(3.61163030609447,-1.,2.11614149815106));
#34473=CARTESIAN_POINT('Ctrl Pts',(3.61508732216891,-1.,2.12138417126355));
#34474=CARTESIAN_POINT('Ctrl Pts',(3.61766963590482,-1.,2.12532774376758));
#34475=CARTESIAN_POINT('Ctrl Pts',(3.61938653649098,-1.,2.12796193131368));
#34476=CARTESIAN_POINT('Ctrl Pts',(3.62024382630768,-1.,2.12928030988903));
#34477=CARTESIAN_POINT('',(3.54075895182139,-1.,2.25898783642071));
#34478=CARTESIAN_POINT('',(3.62024382630768,-1.,2.12928030988903));
#34479=CARTESIAN_POINT('',(3.08655633322211,-1.,2.1297112484669));
#34480=CARTESIAN_POINT('Ctrl Pts',(3.54075895182139,-1.,2.25898783642071));
#34481=CARTESIAN_POINT('Ctrl Pts',(3.53919506647335,-1.,2.2588225169468));
#34482=CARTESIAN_POINT('Ctrl Pts',(3.53606853162228,-1.,2.25848864343951));
#34483=CARTESIAN_POINT('Ctrl Pts',(3.53138243688262,-1.,2.25797812950104));
#34484=CARTESIAN_POINT('Ctrl Pts',(3.52514172847711,-1.,2.25727802940898));
#34485=CARTESIAN_POINT('Ctrl Pts',(3.51735323667612,-1.,2.25637049455044));
#34486=CARTESIAN_POINT('Ctrl Pts',(3.50957720117341,-1.,2.255430469798));
#34487=CARTESIAN_POINT('Ctrl Pts',(3.50181372617971,-1.,2.25445785151868));
#34488=CARTESIAN_POINT('Ctrl Pts',(3.49406296494791,-1.,2.2534525170976));
#34489=CARTESIAN_POINT('Ctrl Pts',(3.48632513240961,-1.,2.25241433138695));
#34490=CARTESIAN_POINT('Ctrl Pts',(3.47860048448691,-1.,2.25134314238687));
#34491=CARTESIAN_POINT('Ctrl Pts',(3.47088928979888,-1.,2.25023877475942));
#34492=CARTESIAN_POINT('Ctrl Pts',(3.46319180177573,-1.,2.2491010234604));
#34493=CARTESIAN_POINT('Ctrl Pts',(3.45550823512049,-1.,2.2479296496077));
#34494=CARTESIAN_POINT('Ctrl Pts',(3.44783872863151,-1.,2.2467243706995));
#34495=CARTESIAN_POINT('Ctrl Pts',(3.4401833646032,-1.,2.24548487526022));
#34496=CARTESIAN_POINT('Ctrl Pts',(3.43254222614803,-1.,2.24421085338727));
#34497=CARTESIAN_POINT('Ctrl Pts',(3.42491544683008,-1.,2.24290202531101));
#34498=CARTESIAN_POINT('Ctrl Pts',(3.41730325539172,-1.,2.24155816587844));
#34499=CARTESIAN_POINT('Ctrl Pts',(3.40970604190328,-1.,2.24017914395289));
#34500=CARTESIAN_POINT('Ctrl Pts',(3.40212434705647,-1.,2.23876491124151));
#34501=CARTESIAN_POINT('Ctrl Pts',(3.39455873448189,-1.,2.23731541452791));
#34502=CARTESIAN_POINT('Ctrl Pts',(3.38700968549563,-1.,2.23583052276308));
#34503=CARTESIAN_POINT('Ctrl Pts',(3.37947749555632,-1.,2.23430995599561));
#34504=CARTESIAN_POINT('Ctrl Pts',(3.37196214349304,-1.,2.23275319569221));
#34505=CARTESIAN_POINT('Ctrl Pts',(3.36446325227848,-1.,2.23115945849739));
#34506=CARTESIAN_POINT('Ctrl Pts',(3.35698038165483,-1.,2.22952789880983));
#34507=CARTESIAN_POINT('Ctrl Pts',(3.34951327111096,-1.,2.22785777756576));
#34508=CARTESIAN_POINT('Ctrl Pts',(3.34206209449375,-1.,2.22614863918047));
#34509=CARTESIAN_POINT('Ctrl Pts',(3.33462772849598,-1.,2.22440049878511));
#34510=CARTESIAN_POINT('Ctrl Pts',(3.3272119632604,-1.,2.22261398879635));
#34511=CARTESIAN_POINT('Ctrl Pts',(3.31981686778022,-1.,2.22078990842776));
#34512=CARTESIAN_POINT('Ctrl Pts',(3.31244421655666,-1.,2.21892881679086));
#34513=CARTESIAN_POINT('Ctrl Pts',(3.30509487819569,-1.,2.21703059947836));
#34514=CARTESIAN_POINT('Ctrl Pts',(3.29776825193159,-1.,2.21509406923369));
#34515=CARTESIAN_POINT('Ctrl Pts',(3.29046159238343,-1.,2.21311648827391));
#34516=CARTESIAN_POINT('Ctrl Pts',(3.28317133333131,-1.,2.21109449750641));
#34517=CARTESIAN_POINT('Ctrl Pts',(3.2758944800554,-1.,2.2090250941743));
#34518=CARTESIAN_POINT('Ctrl Pts',(3.26863006136782,-1.,2.20690665217743));
#34519=CARTESIAN_POINT('Ctrl Pts',(3.26138036637705,-1.,2.20473979048678));
#34520=CARTESIAN_POINT('Ctrl Pts',(3.25415277957775,-1.,2.20252866491545));
#34521=CARTESIAN_POINT('Ctrl Pts',(3.24695715874338,-1.,2.20027910880981));
#34522=CARTESIAN_POINT('Ctrl Pts',(3.23980245361308,-1.,2.19799623693253));
#34523=CARTESIAN_POINT('Ctrl Pts',(3.23269332296933,-1.,2.19568204933168));
#34524=CARTESIAN_POINT('Ctrl Pts',(3.22562734221646,-1.,2.19333345123538));
#34525=CARTESIAN_POINT('Ctrl Pts',(3.21859043114095,-1.,2.19093901948667));
#34526=CARTESIAN_POINT('Ctrl Pts',(3.21156188355769,-1.,2.18848253363901));
#34527=CARTESIAN_POINT('Ctrl Pts',(3.20452259717976,-1.,2.18594876115934));
#34528=CARTESIAN_POINT('Ctrl Pts',(3.19746293740411,-1.,2.18332898656602));
#34529=CARTESIAN_POINT('Ctrl Pts',(3.19038924261573,-1.,2.18062558031778));
#34530=CARTESIAN_POINT('Ctrl Pts',(3.18333474627807,-1.,2.17785968847142));
#34531=CARTESIAN_POINT('Ctrl Pts',(3.17635032802523,-1.,2.17506466903694));
#34532=CARTESIAN_POINT('Ctrl Pts',(3.16948480019497,-1.,2.17227212063817));
#34533=CARTESIAN_POINT('Ctrl Pts',(3.16276685102972,-1.,2.16949910801219));
#34534=CARTESIAN_POINT('Ctrl Pts',(3.15618975593656,-1.,2.1667372844769));
#34535=CARTESIAN_POINT('Ctrl Pts',(3.14968624389054,-1.,2.16393520288072));
#34536=CARTESIAN_POINT('Ctrl Pts',(3.14314440427022,-1.,2.16100905914435));
#34537=CARTESIAN_POINT('Ctrl Pts',(3.13645356563038,-1.,2.15787423530676));
#34538=CARTESIAN_POINT('Ctrl Pts',(3.12954386795646,-1.,2.1544724138292));
#34539=CARTESIAN_POINT('Ctrl Pts',(3.12242318151938,-1.,2.15079698090585));
#34540=CARTESIAN_POINT('Ctrl Pts',(3.11522827016855,-1.,2.14692798457532));
#34541=CARTESIAN_POINT('Ctrl Pts',(3.10821808668859,-1.,2.14302815601973));
#34542=CARTESIAN_POINT('Ctrl Pts',(3.10171267391049,-1.,2.13930228863751));
#34543=CARTESIAN_POINT('Ctrl Pts',(3.0960450242104,-1.,2.13596538661048));
#34544=CARTESIAN_POINT('Ctrl Pts',(3.09151235281963,-1.,2.13321032560894));
#34545=CARTESIAN_POINT('Ctrl Pts',(3.08855597949761,-1.,2.13132142793017));
#34546=CARTESIAN_POINT('Ctrl Pts',(3.08717896996098,-1.,2.13034980480424));
#34547=CARTESIAN_POINT('Ctrl Pts',(3.08668447250322,-1.,2.12991938762374));
#34548=CARTESIAN_POINT('Ctrl Pts',(3.08657131089497,-1.,2.1297578506149));
#34549=CARTESIAN_POINT('Ctrl Pts',(3.08655633322211,-1.,2.1297112484669));
#34550=CARTESIAN_POINT('',(2.97927412174388,-1.,2.27737254473378));
#34551=CARTESIAN_POINT('Origin',(0.,-1.,0.));
#34552=CARTESIAN_POINT('',(3.24257979115744,-1.,2.66939624221984));
#34553=CARTESIAN_POINT('Ctrl Pts',(2.97927412174388,-1.,2.27737254473378));
#34554=CARTESIAN_POINT('Ctrl Pts',(2.97932307137589,-1.,2.27737238849212));
#34555=CARTESIAN_POINT('Ctrl Pts',(2.97951167106106,-1.,2.27743009389704));
#34556=CARTESIAN_POINT('Ctrl Pts',(2.98007383024333,-1.,2.27776738270369));
#34557=CARTESIAN_POINT('Ctrl Pts',(2.98142341809623,-1.,2.27877674853833));
#34558=CARTESIAN_POINT('Ctrl Pts',(2.98413343613858,-1.,2.28100472516582));
#34559=CARTESIAN_POINT('Ctrl Pts',(2.98815432734929,-1.,2.28446419116036));
#34560=CARTESIAN_POINT('Ctrl Pts',(2.9930793098434,-1.,2.28882328690601));
#34561=CARTESIAN_POINT('Ctrl Pts',(2.99863310340004,-1.,2.29385894577999));
#34562=CARTESIAN_POINT('Ctrl Pts',(3.00450832658822,-1.,2.29932091315939));
#34563=CARTESIAN_POINT('Ctrl Pts',(3.01041131063882,-1.,2.30496809486529));
#34564=CARTESIAN_POINT('Ctrl Pts',(3.01610726819019,-1.,2.31060449886577));
#34565=CARTESIAN_POINT('Ctrl Pts',(3.02147780668029,-1.,2.31612479121528));
#34566=CARTESIAN_POINT('Ctrl Pts',(3.02652678416478,-1.,2.32151944306299));
#34567=CARTESIAN_POINT('Ctrl Pts',(3.03133125185047,-1.,2.32683687412027));
#34568=CARTESIAN_POINT('Ctrl Pts',(3.03600588555765,-1.,2.33215619079807));
#34569=CARTESIAN_POINT('Ctrl Pts',(3.04066496998569,-1.,2.33755792953726));
#34570=CARTESIAN_POINT('Ctrl Pts',(3.04537822217311,-1.,2.3430901708402));
#34571=CARTESIAN_POINT('Ctrl Pts',(3.05015565829976,-1.,2.34875673090816));
#34572=CARTESIAN_POINT('Ctrl Pts',(3.05497218368188,-1.,2.35453559889506));
#34573=CARTESIAN_POINT('Ctrl Pts',(3.05978266240056,-1.,2.36039011602084));
#34574=CARTESIAN_POINT('Ctrl Pts',(3.06453964643152,-1.,2.36628220107001));
#34575=CARTESIAN_POINT('Ctrl Pts',(3.06921275497472,-1.,2.37218678163157));
#34576=CARTESIAN_POINT('Ctrl Pts',(3.07379777492133,-1.,2.37809856205524));
#34577=CARTESIAN_POINT('Ctrl Pts',(3.07830597244301,-1.,2.38402401216107));
#34578=CARTESIAN_POINT('Ctrl Pts',(3.08275773747083,-1.,2.38997659219192));
#34579=CARTESIAN_POINT('Ctrl Pts',(3.08717489512919,-1.,2.39597098250635));
#34580=CARTESIAN_POINT('Ctrl Pts',(3.09157266051115,-1.,2.40201704423352));
#34581=CARTESIAN_POINT('Ctrl Pts',(3.09595472616093,-1.,2.40811612696382));
#34582=CARTESIAN_POINT('Ctrl Pts',(3.10031775027683,-1.,2.41426441798067));
#34583=CARTESIAN_POINT('Ctrl Pts',(3.10465410280902,-1.,2.42045498612494));
#34584=CARTESIAN_POINT('Ctrl Pts',(3.10895518969592,-1.,2.42668025870013));
#34585=CARTESIAN_POINT('Ctrl Pts',(3.11321477659012,-1.,2.4329344968514));
#34586=CARTESIAN_POINT('Ctrl Pts',(3.11743156744182,-1.,2.43921571477975));
#34587=CARTESIAN_POINT('Ctrl Pts',(3.12160740887768,-1.,2.44552433364716));
#34588=CARTESIAN_POINT('Ctrl Pts',(3.12574608210849,-1.,2.45186227369848));
#34589=CARTESIAN_POINT('Ctrl Pts',(3.12985188384372,-1.,2.45823188859367));
#34590=CARTESIAN_POINT('Ctrl Pts',(3.13392826623902,-1.,2.4646349433237));
#34591=CARTESIAN_POINT('Ctrl Pts',(3.13797654408931,-1.,2.47107164236827));
#34592=CARTESIAN_POINT('Ctrl Pts',(3.14199655778845,-1.,2.47754112428028));
#34593=CARTESIAN_POINT('Ctrl Pts',(3.14598722723879,-1.,2.48404187418376));
#34594=CARTESIAN_POINT('Ctrl Pts',(3.14994715298903,-1.,2.49057217131985));
#34595=CARTESIAN_POINT('Ctrl Pts',(3.15387518039064,-1.,2.49713050858911));
#34596=CARTESIAN_POINT('Ctrl Pts',(3.15777102413998,-1.,2.50371605688287));
#34597=CARTESIAN_POINT('Ctrl Pts',(3.16163506380211,-1.,2.51032851007939));
#34598=CARTESIAN_POINT('Ctrl Pts',(3.16546808277069,-1.,2.51696788755616));
#34599=CARTESIAN_POINT('Ctrl Pts',(3.1692710213075,-1.,2.523634346718));
#34600=CARTESIAN_POINT('Ctrl Pts',(3.17304474093574,-1.,2.5303280040691));
#34601=CARTESIAN_POINT('Ctrl Pts',(3.17678974135225,-1.,2.53704871950871));
#34602=CARTESIAN_POINT('Ctrl Pts',(3.18050619750515,-1.,2.54379612552948));
#34603=CARTESIAN_POINT('Ctrl Pts',(3.18419408529482,-1.,2.55056972387638));
#34604=CARTESIAN_POINT('Ctrl Pts',(3.1878532811617,-1.,2.55736896206016));
#34605=CARTESIAN_POINT('Ctrl Pts',(3.19148366395201,-1.,2.56419331092909));
#34606=CARTESIAN_POINT('Ctrl Pts',(3.19508523784548,-1.,2.57104235898053));
#34607=CARTESIAN_POINT('Ctrl Pts',(3.19865814628955,-1.,2.577915819091));
#34608=CARTESIAN_POINT('Ctrl Pts',(3.20220261408685,-1.,2.58481347777953));
#34609=CARTESIAN_POINT('Ctrl Pts',(3.20571891028879,-1.,2.59173516023605));
#34610=CARTESIAN_POINT('Ctrl Pts',(3.2092073056959,-1.,2.59868069194267));
#34611=CARTESIAN_POINT('Ctrl Pts',(3.21266802609297,-1.,2.60564985359699));
#34612=CARTESIAN_POINT('Ctrl Pts',(3.21610123232465,-1.,2.61264236718662));
#34613=CARTESIAN_POINT('Ctrl Pts',(3.21950704108654,-1.,2.61965792832396));
#34614=CARTESIAN_POINT('Ctrl Pts',(3.222885536128,-1.,2.62669622735548));
#34615=CARTESIAN_POINT('Ctrl Pts',(3.22623678292539,-1.,2.63375697391438));
#34616=CARTESIAN_POINT('Ctrl Pts',(3.2295608435934,-1.,2.64083992182478));
#34617=CARTESIAN_POINT('Ctrl Pts',(3.23285778738558,-1.,2.64794488744246));
#34618=CARTESIAN_POINT('Ctrl Pts',(3.23612768065687,-1.,2.6550717396303));
#34619=CARTESIAN_POINT('Ctrl Pts',(3.23872200036311,-1.,2.6607906631973));
#34620=CARTESIAN_POINT('Ctrl Pts',(3.24065561087681,-1.,2.66508964664767));
#34621=CARTESIAN_POINT('Ctrl Pts',(3.24193929584813,-1.,2.66795998539861));
#34622=CARTESIAN_POINT('Ctrl Pts',(3.24257979115744,-1.,2.66939624221984));
#34623=CARTESIAN_POINT('',(3.14378277984898,-1.,2.78507268004356));
#34624=CARTESIAN_POINT('',(3.24257979115744,-1.,2.66939624221984));
#34625=CARTESIAN_POINT('',(2.71539546306948,-1.,2.58633475774921));
#34626=CARTESIAN_POINT('Ctrl Pts',(3.14378277984898,-1.,2.78507268004356));
#34627=CARTESIAN_POINT('Ctrl Pts',(3.14226401018816,-1.,2.7846647503589));
#34628=CARTESIAN_POINT('Ctrl Pts',(3.13922819749279,-1.,2.78384588958166));
#34629=CARTESIAN_POINT('Ctrl Pts',(3.13467965833037,-1.,2.78260859419319));
#34630=CARTESIAN_POINT('Ctrl Pts',(3.12862530318457,-1.,2.78094085161413));
#34631=CARTESIAN_POINT('Ctrl Pts',(3.12107467037201,-1.,2.77882610146731));
#34632=CARTESIAN_POINT('Ctrl Pts',(3.11354142303921,-1.,2.77668121002545));
#34633=CARTESIAN_POINT('Ctrl Pts',(3.10602568032564,-1.,2.77450609123362));
#34634=CARTESIAN_POINT('Ctrl Pts',(3.0985276127786,-1.,2.77230064796057));
#34635=CARTESIAN_POINT('Ctrl Pts',(3.0910474538253,-1.,2.7700647803451));
#34636=CARTESIAN_POINT('Ctrl Pts',(3.08358548001503,-1.,2.76779837829373));
#34637=CARTESIAN_POINT('Ctrl Pts',(3.07614198408862,-1.,2.76550131064852));
#34638=CARTESIAN_POINT('Ctrl Pts',(3.0687172484321,-1.,2.76317341453493));
#34639=CARTESIAN_POINT('Ctrl Pts',(3.06131152247454,-1.,2.76081448759882));
#34640=CARTESIAN_POINT('Ctrl Pts',(3.05392498749847,-1.,2.75842427252931));
#34641=CARTESIAN_POINT('Ctrl Pts',(3.04655777351067,-1.,2.75600247455925));
#34642=CARTESIAN_POINT('Ctrl Pts',(3.03921001107977,-1.,2.75354880060314));
#34643=CARTESIAN_POINT('Ctrl Pts',(3.03188187589107,-1.,2.75106299522979));
#34644=CARTESIAN_POINT('Ctrl Pts',(3.02457362909245,-1.,2.7485448718414));
#34645=CARTESIAN_POINT('Ctrl Pts',(3.01728567646611,-1.,2.74599436193625));
#34646=CARTESIAN_POINT('Ctrl Pts',(3.01001855960162,-1.,2.74341150239887));
#34647=CARTESIAN_POINT('Ctrl Pts',(3.00277284351521,-1.,2.74079632883931));
#34648=CARTESIAN_POINT('Ctrl Pts',(2.99554902409778,-1.,2.73814878711641));
#34649=CARTESIAN_POINT('Ctrl Pts',(2.9883474369644,-1.,2.73546864694536));
#34650=CARTESIAN_POINT('Ctrl Pts',(2.98116814232129,-1.,2.73275539286497));
#34651=CARTESIAN_POINT('Ctrl Pts',(2.97401089032676,-1.,2.73000819218414));
#34652=CARTESIAN_POINT('Ctrl Pts',(2.96687537842451,-1.,2.72722614084076));
#34653=CARTESIAN_POINT('Ctrl Pts',(2.95976146492576,-1.,2.72440846811729));
#34654=CARTESIAN_POINT('Ctrl Pts',(2.95266939280621,-1.,2.72155475123364));
#34655=CARTESIAN_POINT('Ctrl Pts',(2.94560002559805,-1.,2.71866514227965));
#34656=CARTESIAN_POINT('Ctrl Pts',(2.93855503247266,-1.,2.71574054592591));
#34657=CARTESIAN_POINT('Ctrl Pts',(2.93153633192595,-1.,2.71278207520817));
#34658=CARTESIAN_POINT('Ctrl Pts',(2.92454558914778,-1.,2.70979055994754));
#34659=CARTESIAN_POINT('Ctrl Pts',(2.91758367994737,-1.,2.70676602302518));
#34660=CARTESIAN_POINT('Ctrl Pts',(2.91065019668329,-1.,2.70370719782113));
#34661=CARTESIAN_POINT('Ctrl Pts',(2.90374285605838,-1.,2.70061095078692));
#34662=CARTESIAN_POINT('Ctrl Pts',(2.89685866123671,-1.,2.69747340630625));
#34663=CARTESIAN_POINT('Ctrl Pts',(2.88999512410309,-1.,2.69429113011374));
#34664=CARTESIAN_POINT('Ctrl Pts',(2.88315153980466,-1.,2.69106236420198));
#34665=CARTESIAN_POINT('Ctrl Pts',(2.8763300724388,-1.,2.68778807801686));
#34666=CARTESIAN_POINT('Ctrl Pts',(2.86953736547238,-1.,2.68447353139599));
#34667=CARTESIAN_POINT('Ctrl Pts',(2.86278224277689,-1.,2.68112602796308));
#34668=CARTESIAN_POINT('Ctrl Pts',(2.85607274378017,-1.,2.67775201955724));
#34669=CARTESIAN_POINT('Ctrl Pts',(2.84941315703092,-1.,2.67435421039677));
#34670=CARTESIAN_POINT('Ctrl Pts',(2.84280157191323,-1.,2.67092916452125));
#34671=CARTESIAN_POINT('Ctrl Pts',(2.83622586853982,-1.,2.66746339678107));
#34672=CARTESIAN_POINT('Ctrl Pts',(2.82966813308998,-1.,2.6639376472693));
#34673=CARTESIAN_POINT('Ctrl Pts',(2.82311188135078,-1.,2.66033388273461));
#34674=CARTESIAN_POINT('Ctrl Pts',(2.81654896073883,-1.,2.65664198781344));
#34675=CARTESIAN_POINT('Ctrl Pts',(2.80998526078165,-1.,2.65286529532208));
#34676=CARTESIAN_POINT('Ctrl Pts',(2.80345029781152,-1.,2.64902988983337));
#34677=CARTESIAN_POINT('Ctrl Pts',(2.79698910670736,-1.,2.6451766779932));
#34678=CARTESIAN_POINT('Ctrl Pts',(2.79064495573224,-1.,2.64134450532584));
#34679=CARTESIAN_POINT('Ctrl Pts',(2.78444351041571,-1.,2.637554714303));
#34680=CARTESIAN_POINT('Ctrl Pts',(2.77837943466449,-1.,2.63379800904599));
#34681=CARTESIAN_POINT('Ctrl Pts',(2.77239433377921,-1.,2.63001305229625));
#34682=CARTESIAN_POINT('Ctrl Pts',(2.7663907847902,-1.,2.62609956506355));
#34683=CARTESIAN_POINT('Ctrl Pts',(2.76027271596686,-1.,2.62195665834605));
#34684=CARTESIAN_POINT('Ctrl Pts',(2.7539802502603,-1.,2.61751580407667));
#34685=CARTESIAN_POINT('Ctrl Pts',(2.74752219567252,-1.,2.61277170105813));
#34686=CARTESIAN_POINT('Ctrl Pts',(2.7410211099909,-1.,2.60782480638448));
#34687=CARTESIAN_POINT('Ctrl Pts',(2.73470730109615,-1.,2.60287635688728));
#34688=CARTESIAN_POINT('Ctrl Pts',(2.7288648348152,-1.,2.59817869034746));
#34689=CARTESIAN_POINT('Ctrl Pts',(2.72378896977134,-1.,2.59399625537278));
#34690=CARTESIAN_POINT('Ctrl Pts',(2.71974308958086,-1.,2.59056604771971));
#34691=CARTESIAN_POINT('Ctrl Pts',(2.71711860281815,-1.,2.58823792682672));
#34692=CARTESIAN_POINT('Ctrl Pts',(2.71591054189786,-1.,2.58706285424358));
#34693=CARTESIAN_POINT('Ctrl Pts',(2.71548946460575,-1.,2.58656037976753));
#34694=CARTESIAN_POINT('Ctrl Pts',(2.71540296616024,-1.,2.58638312917167));
#34695=CARTESIAN_POINT('Ctrl Pts',(2.71539546306948,-1.,2.58633475774921));
#34696=CARTESIAN_POINT('',(2.58633475775051,-1.,2.71539546306824));
#34697=CARTESIAN_POINT('Origin',(0.,-1.,0.));
#34698=CARTESIAN_POINT('',(2.78507268004355,-1.,3.14378277984898));
#34699=CARTESIAN_POINT('Ctrl Pts',(2.58633475775051,-1.,2.71539546306824));
#34700=CARTESIAN_POINT('Ctrl Pts',(2.58638312917291,-1.,2.71540296615967));
#34701=CARTESIAN_POINT('Ctrl Pts',(2.58656037976884,-1.,2.71548946460616));
#34702=CARTESIAN_POINT('Ctrl Pts',(2.58706285424469,-1.,2.71591054189884));
#34703=CARTESIAN_POINT('Ctrl Pts',(2.58823792682724,-1.,2.7171186028189));
#34704=CARTESIAN_POINT('Ctrl Pts',(2.59056604771863,-1.,2.7197430895797));
#34705=CARTESIAN_POINT('Ctrl Pts',(2.59399625537407,-1.,2.72378896977273));
#34706=CARTESIAN_POINT('Ctrl Pts',(2.5981786903501,-1.,2.72886483481804));
#34707=CARTESIAN_POINT('Ctrl Pts',(2.60287635689,-1.,2.73470730109906));
#34708=CARTESIAN_POINT('Ctrl Pts',(2.60782480638629,-1.,2.74102110999284));
#34709=CARTESIAN_POINT('Ctrl Pts',(2.61277170105864,-1.,2.74752219567307));
#34710=CARTESIAN_POINT('Ctrl Pts',(2.61751580407608,-1.,2.75398025025967));
#34711=CARTESIAN_POINT('Ctrl Pts',(2.62195665834491,-1.,2.76027271596564));
#34712=CARTESIAN_POINT('Ctrl Pts',(2.6260995650624,-1.,2.76639078478898));
#34713=CARTESIAN_POINT('Ctrl Pts',(2.63001305229548,-1.,2.77239433377839));
#34714=CARTESIAN_POINT('Ctrl Pts',(2.63379800904575,-1.,2.77837943466423));
#34715=CARTESIAN_POINT('Ctrl Pts',(2.63755471430322,-1.,2.78444351041594));
#34716=CARTESIAN_POINT('Ctrl Pts',(2.64134450532632,-1.,2.79064495573275));
#34717=CARTESIAN_POINT('Ctrl Pts',(2.6451766779937,-1.,2.7969891067079));
#34718=CARTESIAN_POINT('Ctrl Pts',(2.64902988983373,-1.,2.80345029781191));
#34719=CARTESIAN_POINT('Ctrl Pts',(2.65286529532221,-1.,2.80998526078179));
#34720=CARTESIAN_POINT('Ctrl Pts',(2.65664198781335,-1.,2.81654896073874));
#34721=CARTESIAN_POINT('Ctrl Pts',(2.66033388273437,-1.,2.82311188135053));
#34722=CARTESIAN_POINT('Ctrl Pts',(2.66393764726902,-1.,2.82966813308969));
#34723=CARTESIAN_POINT('Ctrl Pts',(2.66746339678085,-1.,2.8362258685396));
#34724=CARTESIAN_POINT('Ctrl Pts',(2.67092916452116,-1.,2.84280157191314));
#34725=CARTESIAN_POINT('Ctrl Pts',(2.67435421039682,-1.,2.84941315703096));
#34726=CARTESIAN_POINT('Ctrl Pts',(2.67775201955736,-1.,2.85607274378031));
#34727=CARTESIAN_POINT('Ctrl Pts',(2.68112602796323,-1.,2.86278224277705));
#34728=CARTESIAN_POINT('Ctrl Pts',(2.6844735313961,-1.,2.8695373654725));
#34729=CARTESIAN_POINT('Ctrl Pts',(2.68778807801691,-1.,2.87633007243885));
#34730=CARTESIAN_POINT('Ctrl Pts',(2.69106236420196,-1.,2.88315153980464));
#34731=CARTESIAN_POINT('Ctrl Pts',(2.69429113011369,-1.,2.88999512410304));
#34732=CARTESIAN_POINT('Ctrl Pts',(2.69747340630621,-1.,2.89685866123668));
#34733=CARTESIAN_POINT('Ctrl Pts',(2.70061095078692,-1.,2.90374285605839));
#34734=CARTESIAN_POINT('Ctrl Pts',(2.70370719782114,-1.,2.91065019668331));
#34735=CARTESIAN_POINT('Ctrl Pts',(2.70676602302518,-1.,2.91758367994738));
#34736=CARTESIAN_POINT('Ctrl Pts',(2.70979055994751,-1.,2.92454558914774));
#34737=CARTESIAN_POINT('Ctrl Pts',(2.71278207520807,-1.,2.93153633192583));
#34738=CARTESIAN_POINT('Ctrl Pts',(2.71574054592575,-1.,2.93855503247248));
#34739=CARTESIAN_POINT('Ctrl Pts',(2.71866514227951,-1.,2.94560002559789));
#34740=CARTESIAN_POINT('Ctrl Pts',(2.72155475123361,-1.,2.95266939280617));
#34741=CARTESIAN_POINT('Ctrl Pts',(2.72440846811745,-1.,2.95976146492595));
#34742=CARTESIAN_POINT('Ctrl Pts',(2.72722614084112,-1.,2.96687537842492));
#34743=CARTESIAN_POINT('Ctrl Pts',(2.7300081921846,-1.,2.97401089032729));
#34744=CARTESIAN_POINT('Ctrl Pts',(2.73275539286537,-1.,2.98116814232175));
#34745=CARTESIAN_POINT('Ctrl Pts',(2.73546864694548,-1.,2.98834743696455));
#34746=CARTESIAN_POINT('Ctrl Pts',(2.73814878711609,-1.,2.99554902409741));
#34747=CARTESIAN_POINT('Ctrl Pts',(2.74079632883852,-1.,3.00277284351431));
#34748=CARTESIAN_POINT('Ctrl Pts',(2.7434115023978,-1.,3.01001855960041));
#34749=CARTESIAN_POINT('Ctrl Pts',(2.74599436193528,-1.,3.01728567646502));
#34750=CARTESIAN_POINT('Ctrl Pts',(2.74854487184099,-1.,3.02457362909199));
#34751=CARTESIAN_POINT('Ctrl Pts',(2.75106299523032,-1.,3.03188187589168));
#34752=CARTESIAN_POINT('Ctrl Pts',(2.75354880060473,-1.,3.03921001108158));
#34753=CARTESIAN_POINT('Ctrl Pts',(2.7560024745616,-1.,3.04655777351333));
#34754=CARTESIAN_POINT('Ctrl Pts',(2.75842427253164,-1.,3.05392498750112));
#34755=CARTESIAN_POINT('Ctrl Pts',(2.76081448760011,-1.,3.06131152247599));
#34756=CARTESIAN_POINT('Ctrl Pts',(2.76317341453415,-1.,3.06871724843121));
#34757=CARTESIAN_POINT('Ctrl Pts',(2.76550131064522,-1.,3.07614198408488));
#34758=CARTESIAN_POINT('Ctrl Pts',(2.76779837828843,-1.,3.08358548000904));
#34759=CARTESIAN_POINT('Ctrl Pts',(2.77006478033937,-1.,3.09104745381882));
#34760=CARTESIAN_POINT('Ctrl Pts',(2.77230064795679,-1.,3.09852761277432));
#34761=CARTESIAN_POINT('Ctrl Pts',(2.7745060912343,-1.,3.10602568032641));
#34762=CARTESIAN_POINT('Ctrl Pts',(2.77668121003225,-1.,3.11354142304692));
#34763=CARTESIAN_POINT('Ctrl Pts',(2.77882610147986,-1.,3.12107467038623));
#34764=CARTESIAN_POINT('Ctrl Pts',(2.78094085162947,-1.,3.12862530320194));
#34765=CARTESIAN_POINT('Ctrl Pts',(2.78260859420629,-1.,3.1346796583452));
#34766=CARTESIAN_POINT('Ctrl Pts',(2.78384588958965,-1.,3.13922819750185));
#34767=CARTESIAN_POINT('Ctrl Pts',(2.78466475036183,-1.,3.14226401019149));
#34768=CARTESIAN_POINT('Ctrl Pts',(2.78507268004355,-1.,3.14378277984898));
#34769=CARTESIAN_POINT('',(2.66939624221984,-1.,3.24257979115744));
#34770=CARTESIAN_POINT('',(2.78507268004355,-1.,3.14378277984898));
#34771=CARTESIAN_POINT('',(2.27737254473521,-1.,2.97927412174279));
#34772=CARTESIAN_POINT('Ctrl Pts',(2.66939624221984,-1.,3.24257979115744));
#34773=CARTESIAN_POINT('Ctrl Pts',(2.66795998539579,-1.,3.24193929584471));
#34774=CARTESIAN_POINT('Ctrl Pts',(2.66508964663997,-1.,3.24065561086749));
#34775=CARTESIAN_POINT('Ctrl Pts',(2.6607906631847,-1.,3.23872200034785));
#34776=CARTESIAN_POINT('Ctrl Pts',(2.65507173961555,-1.,3.236127680639));
#34777=CARTESIAN_POINT('Ctrl Pts',(2.64794488743038,-1.,3.23285778737096));
#34778=CARTESIAN_POINT('Ctrl Pts',(2.64083992181823,-1.,3.22956084358547));
#34779=CARTESIAN_POINT('Ctrl Pts',(2.63375697391372,-1.,3.2262367829246));
#34780=CARTESIAN_POINT('Ctrl Pts',(2.62669622735912,-1.,3.2228855361324));
#34781=CARTESIAN_POINT('Ctrl Pts',(2.61965792832947,-1.,3.21950704109321));
#34782=CARTESIAN_POINT('Ctrl Pts',(2.61264236719171,-1.,3.21610123233082));
#34783=CARTESIAN_POINT('Ctrl Pts',(2.60564985360017,-1.,3.21266802609682));
#34784=CARTESIAN_POINT('Ctrl Pts',(2.59868069194341,-1.,3.20920730569681));
#34785=CARTESIAN_POINT('Ctrl Pts',(2.59173516023481,-1.,3.2057189102873));
#34786=CARTESIAN_POINT('Ctrl Pts',(2.58481347777728,-1.,3.20220261408414));
#34787=CARTESIAN_POINT('Ctrl Pts',(2.57791581908874,-1.,3.19865814628682));
#34788=CARTESIAN_POINT('Ctrl Pts',(2.57104235897899,-1.,3.19508523784363));
#34789=CARTESIAN_POINT('Ctrl Pts',(2.56419331092858,-1.,3.19148366395139));
#34790=CARTESIAN_POINT('Ctrl Pts',(2.55736896206056,-1.,3.18785328116218));
#34791=CARTESIAN_POINT('Ctrl Pts',(2.5505697238773,-1.,3.18419408529594));
#34792=CARTESIAN_POINT('Ctrl Pts',(2.5437961255305,-1.,3.1805061975064));
#34793=CARTESIAN_POINT('Ctrl Pts',(2.53704871950948,-1.,3.17678974135318));
#34794=CARTESIAN_POINT('Ctrl Pts',(2.53032800406941,-1.,3.17304474093612));
#34795=CARTESIAN_POINT('Ctrl Pts',(2.52363434671788,-1.,3.16927102130736));
#34796=CARTESIAN_POINT('Ctrl Pts',(2.51696788755577,-1.,3.16546808277023));
#34797=CARTESIAN_POINT('Ctrl Pts',(2.51032851007894,-1.,3.16163506380157));
#34798=CARTESIAN_POINT('Ctrl Pts',(2.50371605688252,-1.,3.15777102413957));
#34799=CARTESIAN_POINT('Ctrl Pts',(2.49713050858896,-1.,3.15387518039046));
#34800=CARTESIAN_POINT('Ctrl Pts',(2.49057217131988,-1.,3.14994715298907));
#34801=CARTESIAN_POINT('Ctrl Pts',(2.4840418741839,-1.,3.14598722723896));
#34802=CARTESIAN_POINT('Ctrl Pts',(2.47754112428043,-1.,3.14199655778863));
#34803=CARTESIAN_POINT('Ctrl Pts',(2.47107164236838,-1.,3.13797654408943));
#34804=CARTESIAN_POINT('Ctrl Pts',(2.46463494332374,-1.,3.13392826623906));
#34805=CARTESIAN_POINT('Ctrl Pts',(2.45823188859366,-1.,3.12985188384371));
#34806=CARTESIAN_POINT('Ctrl Pts',(2.45186227369846,-1.,3.12574608210847));
#34807=CARTESIAN_POINT('Ctrl Pts',(2.44552433364715,-1.,3.12160740887768));
#34808=CARTESIAN_POINT('Ctrl Pts',(2.43921571477977,-1.,3.11743156744186));
#34809=CARTESIAN_POINT('Ctrl Pts',(2.43293449685144,-1.,3.11321477659018));
#34810=CARTESIAN_POINT('Ctrl Pts',(2.42668025870015,-1.,3.10895518969595));
#34811=CARTESIAN_POINT('Ctrl Pts',(2.42045498612489,-1.,3.10465410280896));
#34812=CARTESIAN_POINT('Ctrl Pts',(2.41426441798057,-1.,3.1003177502767));
#34813=CARTESIAN_POINT('Ctrl Pts',(2.40811612696369,-1.,3.09595472616076));
#34814=CARTESIAN_POINT('Ctrl Pts',(2.40201704423341,-1.,3.091572660511));
#34815=CARTESIAN_POINT('Ctrl Pts',(2.39597098250631,-1.,3.08717489512914));
#34816=CARTESIAN_POINT('Ctrl Pts',(2.38997659219199,-1.,3.08275773747093));
#34817=CARTESIAN_POINT('Ctrl Pts',(2.38402401216126,-1.,3.07830597244326));
#34818=CARTESIAN_POINT('Ctrl Pts',(2.37809856205548,-1.,3.07379777492165));
#34819=CARTESIAN_POINT('Ctrl Pts',(2.37218678163178,-1.,3.069212754975));
#34820=CARTESIAN_POINT('Ctrl Pts',(2.36628220107009,-1.,3.06453964643162));
#34821=CARTESIAN_POINT('Ctrl Pts',(2.36039011602072,-1.,3.0597826624004));
#34822=CARTESIAN_POINT('Ctrl Pts',(2.35453559889474,-1.,3.05497218368146));
#34823=CARTESIAN_POINT('Ctrl Pts',(2.3487567309077,-1.,3.05015565829918));
#34824=CARTESIAN_POINT('Ctrl Pts',(2.34309017083976,-1.,3.04537822217256));
#34825=CARTESIAN_POINT('Ctrl Pts',(2.33755792953706,-1.,3.04066496998544));
#34826=CARTESIAN_POINT('Ctrl Pts',(2.33215619079829,-1.,3.03600588555793));
#34827=CARTESIAN_POINT('Ctrl Pts',(2.32683687412096,-1.,3.03133125185136));
#34828=CARTESIAN_POINT('Ctrl Pts',(2.32151944306402,-1.,3.02652678416611));
#34829=CARTESIAN_POINT('Ctrl Pts',(2.31612479121631,-1.,3.02147780668161));
#34830=CARTESIAN_POINT('Ctrl Pts',(2.31060449886629,-1.,3.01610726819086));
#34831=CARTESIAN_POINT('Ctrl Pts',(2.30496809486482,-1.,3.01041131063823));
#34832=CARTESIAN_POINT('Ctrl Pts',(2.29932091315775,-1.,3.00450832658613));
#34833=CARTESIAN_POINT('Ctrl Pts',(2.29385894577754,-1.,2.99863310339691));
#34834=CARTESIAN_POINT('Ctrl Pts',(2.28882328690362,-1.,2.99307930984034));
#34835=CARTESIAN_POINT('Ctrl Pts',(2.28446419115919,-1.,2.9881543273478));
#34836=CARTESIAN_POINT('Ctrl Pts',(2.28100472516679,-1.,2.98413343613983));
#34837=CARTESIAN_POINT('Ctrl Pts',(2.27877674853766,-1.,2.9814234180956));
#34838=CARTESIAN_POINT('Ctrl Pts',(2.27776738270289,-1.,2.98007383024207));
#34839=CARTESIAN_POINT('Ctrl Pts',(2.27743009389684,-1.,2.9795116710597));
#34840=CARTESIAN_POINT('Ctrl Pts',(2.27737238849287,-1.,2.97932307137476));
#34841=CARTESIAN_POINT('Ctrl Pts',(2.27737254473521,-1.,2.97927412174279));
#34842=CARTESIAN_POINT('',(2.12971124846838,-1.,3.08655633322109));
#34843=CARTESIAN_POINT('Origin',(0.,-1.,0.));
#34844=CARTESIAN_POINT('',(2.25898783642071,-1.,3.54075895182139));
#34845=CARTESIAN_POINT('Ctrl Pts',(2.12971124846838,-1.,3.08655633322109));
#34846=CARTESIAN_POINT('Ctrl Pts',(2.1297578506162,-1.,3.0865713108946));
#34847=CARTESIAN_POINT('Ctrl Pts',(2.12991938762497,-1.,3.08668447250383));
#34848=CARTESIAN_POINT('Ctrl Pts',(2.13034980480519,-1.,3.08717896996213));
#34849=CARTESIAN_POINT('Ctrl Pts',(2.13132142793056,-1.,3.08855597949844));
#34850=CARTESIAN_POINT('Ctrl Pts',(2.13321032560805,-1.,3.09151235281832));
#34851=CARTESIAN_POINT('Ctrl Pts',(2.13596538661154,-1.,3.09604502421197));
#34852=CARTESIAN_POINT('Ctrl Pts',(2.13930228863968,-1.,3.1017126739137));
#34853=CARTESIAN_POINT('Ctrl Pts',(2.14302815602195,-1.,3.10821808669189));
#34854=CARTESIAN_POINT('Ctrl Pts',(2.1469279845768,-1.,3.11522827017075));
#34855=CARTESIAN_POINT('Ctrl Pts',(2.15079698090627,-1.,3.12242318152001));
#34856=CARTESIAN_POINT('Ctrl Pts',(2.15447241382872,-1.,3.12954386795575));
#34857=CARTESIAN_POINT('Ctrl Pts',(2.15787423530583,-1.,3.136453565629));
#34858=CARTESIAN_POINT('Ctrl Pts',(2.16100905914341,-1.,3.14314440426882));
#34859=CARTESIAN_POINT('Ctrl Pts',(2.16393520288009,-1.,3.14968624388961));
#34860=CARTESIAN_POINT('Ctrl Pts',(2.1667372844767,-1.,3.15618975593627));
#34861=CARTESIAN_POINT('Ctrl Pts',(2.16949910801237,-1.,3.16276685102999));
#34862=CARTESIAN_POINT('Ctrl Pts',(2.17227212063857,-1.,3.16948480019555));
#34863=CARTESIAN_POINT('Ctrl Pts',(2.17506466903736,-1.,3.17635032802584));
#34864=CARTESIAN_POINT('Ctrl Pts',(2.17785968847172,-1.,3.18333474627851));
#34865=CARTESIAN_POINT('Ctrl Pts',(2.18062558031789,-1.,3.19038924261589));
#34866=CARTESIAN_POINT('Ctrl Pts',(2.18332898656595,-1.,3.197462937404));
#34867=CARTESIAN_POINT('Ctrl Pts',(2.18594876115914,-1.,3.20452259717947));
#34868=CARTESIAN_POINT('Ctrl Pts',(2.18848253363878,-1.,3.21156188355736));
#34869=CARTESIAN_POINT('Ctrl Pts',(2.1909390194865,-1.,3.21859043114069));
#34870=CARTESIAN_POINT('Ctrl Pts',(2.19333345123531,-1.,3.22562734221636));
#34871=CARTESIAN_POINT('Ctrl Pts',(2.19568204933172,-1.,3.23269332296938));
#34872=CARTESIAN_POINT('Ctrl Pts',(2.19799623693263,-1.,3.23980245361323));
#34873=CARTESIAN_POINT('Ctrl Pts',(2.20027910880993,-1.,3.24695715874356));
#34874=CARTESIAN_POINT('Ctrl Pts',(2.20252866491554,-1.,3.25415277957789));
#34875=CARTESIAN_POINT('Ctrl Pts',(2.20473979048682,-1.,3.26138036637711));
#34876=CARTESIAN_POINT('Ctrl Pts',(2.20690665217741,-1.,3.2686300613678));
#34877=CARTESIAN_POINT('Ctrl Pts',(2.20902509417425,-1.,3.27589448005534));
#34878=CARTESIAN_POINT('Ctrl Pts',(2.21109449750638,-1.,3.28317133333127));
#34879=CARTESIAN_POINT('Ctrl Pts',(2.2131164882739,-1.,3.29046159238344));
#34880=CARTESIAN_POINT('Ctrl Pts',(2.21509406923369,-1.,3.29776825193162));
#34881=CARTESIAN_POINT('Ctrl Pts',(2.21703059947837,-1.,3.3050948781957));
#34882=CARTESIAN_POINT('Ctrl Pts',(2.21892881679083,-1.,3.31244421655662));
#34883=CARTESIAN_POINT('Ctrl Pts',(2.22078990842768,-1.,3.31981686778008));
#34884=CARTESIAN_POINT('Ctrl Pts',(2.22261398879623,-1.,3.32721196326019));
#34885=CARTESIAN_POINT('Ctrl Pts',(2.224400498785,-1.,3.3346277284958));
#34886=CARTESIAN_POINT('Ctrl Pts',(2.22614863918044,-1.,3.34206209449371));
#34887=CARTESIAN_POINT('Ctrl Pts',(2.22785777756588,-1.,3.34951327111117));
#34888=CARTESIAN_POINT('Ctrl Pts',(2.22952789881011,-1.,3.35698038165529));
#34889=CARTESIAN_POINT('Ctrl Pts',(2.23115945849777,-1.,3.36446325227908));
#34890=CARTESIAN_POINT('Ctrl Pts',(2.23275319569253,-1.,3.37196214349356));
#34891=CARTESIAN_POINT('Ctrl Pts',(2.23430995599572,-1.,3.37947749555649));
#34892=CARTESIAN_POINT('Ctrl Pts',(2.23583052276281,-1.,3.38700968549522));
#34893=CARTESIAN_POINT('Ctrl Pts',(2.23731541452726,-1.,3.39455873448088));
#34894=CARTESIAN_POINT('Ctrl Pts',(2.23876491124064,-1.,3.40212434705511));
#34895=CARTESIAN_POINT('Ctrl Pts',(2.24017914395211,-1.,3.40970604190205));
#34896=CARTESIAN_POINT('Ctrl Pts',(2.24155816587811,-1.,3.41730325539119));
#34897=CARTESIAN_POINT('Ctrl Pts',(2.24290202531144,-1.,3.42491544683075));
#34898=CARTESIAN_POINT('Ctrl Pts',(2.24421085338856,-1.,3.43254222615007));
#34899=CARTESIAN_POINT('Ctrl Pts',(2.24548487526212,-1.,3.44018336460619));
#34900=CARTESIAN_POINT('Ctrl Pts',(2.24672437070139,-1.,3.44783872863448));
#34901=CARTESIAN_POINT('Ctrl Pts',(2.24792964960874,-1.,3.45550823512213));
#34902=CARTESIAN_POINT('Ctrl Pts',(2.24910102345977,-1.,3.46319180177474));
#34903=CARTESIAN_POINT('Ctrl Pts',(2.25023877475674,-1.,3.47088928979467));
#34904=CARTESIAN_POINT('Ctrl Pts',(2.25134314238258,-1.,3.47860048448015));
#34905=CARTESIAN_POINT('Ctrl Pts',(2.25241433138231,-1.,3.48632513240231));
#34906=CARTESIAN_POINT('Ctrl Pts',(2.25345251709453,-1.,3.49406296494309));
#34907=CARTESIAN_POINT('Ctrl Pts',(2.25445785151923,-1.,3.50181372618058));
#34908=CARTESIAN_POINT('Ctrl Pts',(2.25543046980351,-1.,3.50957720118209));
#34909=CARTESIAN_POINT('Ctrl Pts',(2.25637049456061,-1.,3.51735323669213));
#34910=CARTESIAN_POINT('Ctrl Pts',(2.25727802942141,-1.,3.52514172849666));
#34911=CARTESIAN_POINT('Ctrl Pts',(2.25797812951166,-1.,3.53138243689932));
#34912=CARTESIAN_POINT('Ctrl Pts',(2.25848864344599,-1.,3.53606853163247));
#34913=CARTESIAN_POINT('Ctrl Pts',(2.25882251694918,-1.,3.5391950664771));
#34914=CARTESIAN_POINT('Ctrl Pts',(2.25898783642071,-1.,3.54075895182139));
#34915=CARTESIAN_POINT('',(2.12928030988903,-1.,3.62024382630768));
#34916=CARTESIAN_POINT('',(2.25898783642071,-1.,3.54075895182139));
#34917=CARTESIAN_POINT('',(1.78327315618341,-1.,3.29885386921513));
#34918=CARTESIAN_POINT('Ctrl Pts',(2.12928030988903,-1.,3.62024382630768));
#34919=CARTESIAN_POINT('Ctrl Pts',(2.12796193131142,-1.,3.61938653648716));
#34920=CARTESIAN_POINT('Ctrl Pts',(2.12532774376144,-1.,3.61766963589442));
#34921=CARTESIAN_POINT('Ctrl Pts',(2.12138417125349,-1.,3.61508732215187));
#34922=CARTESIAN_POINT('Ctrl Pts',(2.11614149813928,-1.,3.61163030607452));
#34923=CARTESIAN_POINT('Ctrl Pts',(2.10961391333497,-1.,3.60728578530968));
#34924=CARTESIAN_POINT('Ctrl Pts',(2.10311217727687,-1.,3.60291797087849));
#34925=CARTESIAN_POINT('Ctrl Pts',(2.09663642986579,-1.,3.59852681775396));
#34926=CARTESIAN_POINT('Ctrl Pts',(2.09018686331706,-1.,3.5941122862608));
#34927=CARTESIAN_POINT('Ctrl Pts',(2.08376373049196,-1.,3.58967435355834));
#34928=CARTESIAN_POINT('Ctrl Pts',(2.07736732842524,-1.,3.58521300039988));
#34929=CARTESIAN_POINT('Ctrl Pts',(2.07099797606,-1.,3.58072819250872));
#34930=CARTESIAN_POINT('Ctrl Pts',(2.06465599229234,-1.,3.57621986224402));
#34931=CARTESIAN_POINT('Ctrl Pts',(2.05834167687425,-1.,3.5716878942334));
#34932=CARTESIAN_POINT('Ctrl Pts',(2.05205528172911,-1.,3.56713209977904));
#34933=CARTESIAN_POINT('Ctrl Pts',(2.04579702158876,-1.,3.56255223871505));
#34934=CARTESIAN_POINT('Ctrl Pts',(2.03956711119976,-1.,3.55794807264844));
#34935=CARTESIAN_POINT('Ctrl Pts',(2.03336579658133,-1.,3.55331941293949));
#34936=CARTESIAN_POINT('Ctrl Pts',(2.02719338376175,-1.,3.54866616282227));
#34937=CARTESIAN_POINT('Ctrl Pts',(2.02105027983104,-1.,3.54398838254136));
#34938=CARTESIAN_POINT('Ctrl Pts',(2.01493698847351,-1.,3.53928627453642));
#34939=CARTESIAN_POINT('Ctrl Pts',(2.00885403604746,-1.,3.53456004727424));
#34940=CARTESIAN_POINT('Ctrl Pts',(2.00280191090366,-1.,3.52980980250224));
#34941=CARTESIAN_POINT('Ctrl Pts',(1.99678100339295,-1.,3.52503542491728));
#34942=CARTESIAN_POINT('Ctrl Pts',(1.99079153006112,-1.,3.52023644289142));
#34943=CARTESIAN_POINT('Ctrl Pts',(1.9848335106103,-1.,3.51541198728301));
#34944=CARTESIAN_POINT('Ctrl Pts',(1.97890693666288,-1.,3.51056110478287));
#34945=CARTESIAN_POINT('Ctrl Pts',(1.97301191162968,-1.,3.5056830186108));
#34946=CARTESIAN_POINT('Ctrl Pts',(1.96714879724052,-1.,3.50077740176267));
#34947=CARTESIAN_POINT('Ctrl Pts',(1.961318367765,-1.,3.49584466573064));
#34948=CARTESIAN_POINT('Ctrl Pts',(1.95552193112084,-1.,3.49088618670987));
#34949=CARTESIAN_POINT('Ctrl Pts',(1.94976096795911,-1.,3.48590361610814));
#34950=CARTESIAN_POINT('Ctrl Pts',(1.94403680554065,-1.,3.48089825770416));
#34951=CARTESIAN_POINT('Ctrl Pts',(1.93835026973887,-1.,3.47587040389915));
#34952=CARTESIAN_POINT('Ctrl Pts',(1.93270136427081,-1.,3.47081872409781));
#34953=CARTESIAN_POINT('Ctrl Pts',(1.92708888591158,-1.,3.46573953254084));
#34954=CARTESIAN_POINT('Ctrl Pts',(1.92151118213212,-1.,3.46062821722485));
#34955=CARTESIAN_POINT('Ctrl Pts',(1.91596694784063,-1.,3.4554807430995));
#34956=CARTESIAN_POINT('Ctrl Pts',(1.91045605593639,-1.,3.45029522038888));
#34957=CARTESIAN_POINT('Ctrl Pts',(1.90498026502304,-1.,3.44507323983368));
#34958=CARTESIAN_POINT('Ctrl Pts',(1.89954426803384,-1.,3.4398218567809));
#34959=CARTESIAN_POINT('Ctrl Pts',(1.89415420002542,-1.,3.43455074411571));
#34960=CARTESIAN_POINT('Ctrl Pts',(1.88881571322009,-1.,3.42926852222158));
#34961=CARTESIAN_POINT('Ctrl Pts',(1.8835320506206,-1.,3.42397908819736));
#34962=CARTESIAN_POINT('Ctrl Pts',(1.87830245689344,-1.,3.41867858383771));
#34963=CARTESIAN_POINT('Ctrl Pts',(1.87311957248121,-1.,3.41335043875209));
#34964=CARTESIAN_POINT('Ctrl Pts',(1.86797231196654,-1.,3.40797080000549));
#34965=CARTESIAN_POINT('Ctrl Pts',(1.86285057051245,-1.,3.40251742305476));
#34966=CARTESIAN_POINT('Ctrl Pts',(1.85774972037062,-1.,3.39697816833067));
#34967=CARTESIAN_POINT('Ctrl Pts',(1.85267433291769,-1.,3.39135802549398));
#34968=CARTESIAN_POINT('Ctrl Pts',(1.84764441927753,-1.,3.38569092349592));
#34969=CARTESIAN_POINT('Ctrl Pts',(1.84269016931643,-1.,3.38002968341157));
#34970=CARTESIAN_POINT('Ctrl Pts',(1.83784072967077,-1.,3.37442462015853));
#34971=CARTESIAN_POINT('Ctrl Pts',(1.83311391452322,-1.,3.36890396271836));
#34972=CARTESIAN_POINT('Ctrl Pts',(1.82850752153199,-1.,3.36345722124158));
#34973=CARTESIAN_POINT('Ctrl Pts',(1.82398496829301,-1.,3.35800801557424));
#34974=CARTESIAN_POINT('Ctrl Pts',(1.81948458796829,-1.,3.35243086937598));
#34975=CARTESIAN_POINT('Ctrl Pts',(1.81494618732853,-1.,3.34660014370673));
#34976=CARTESIAN_POINT('Ctrl Pts',(1.81033399625352,-1.,3.34043216147606));
#34977=CARTESIAN_POINT('Ctrl Pts',(1.80565802981102,-1.,3.33392460276808));
#34978=CARTESIAN_POINT('Ctrl Pts',(1.80100380443406,-1.,3.32721088039578));
#34979=CARTESIAN_POINT('Ctrl Pts',(1.79652817033251,-1.,3.3205535510082));
#34980=CARTESIAN_POINT('Ctrl Pts',(1.79242331349949,-1.,3.31428038326424));
#34981=CARTESIAN_POINT('Ctrl Pts',(1.78888832245873,-1.,3.30873412266788));
#34982=CARTESIAN_POINT('Ctrl Pts',(1.78610045419846,-1.,3.30422155559112));
#34983=CARTESIAN_POINT('Ctrl Pts',(1.78432384788174,-1.,3.30119637003393));
#34984=CARTESIAN_POINT('Ctrl Pts',(1.78353803106924,-1.,3.299705498242));
#34985=CARTESIAN_POINT('Ctrl Pts',(1.78329283591905,-1.,3.29909749657808));
#34986=CARTESIAN_POINT('Ctrl Pts',(1.78326534445518,-1.,3.29890219175423));
#34987=CARTESIAN_POINT('Ctrl Pts',(1.78327315618341,-1.,3.29885386921513));
#34988=CARTESIAN_POINT('',(1.62064718014256,-1.,3.38171594275687));
#34989=CARTESIAN_POINT('Origin',(0.,-1.,0.));
#34990=CARTESIAN_POINT('',(1.67727921511438,-1.,3.85054988729471));
#34991=CARTESIAN_POINT('Ctrl Pts',(1.62064718014256,-1.,3.38171594275687));
#34992=CARTESIAN_POINT('Ctrl Pts',(1.62069086551626,-1.,3.38173802621243));
#34993=CARTESIAN_POINT('Ctrl Pts',(1.62083271136059,-1.,3.38187506457001));
#34994=CARTESIAN_POINT('Ctrl Pts',(1.62118047294574,-1.,3.38243080602536));
#34995=CARTESIAN_POINT('Ctrl Pts',(1.62192472202795,-1.,3.3839428576331));
#34996=CARTESIAN_POINT('Ctrl Pts',(1.62332788556183,-1.,3.38715832178929));
#34997=CARTESIAN_POINT('Ctrl Pts',(1.62533996116793,-1.,3.39206617497078));
#34998=CARTESIAN_POINT('Ctrl Pts',(1.62774916464571,-1.,3.39818605298342));
#34999=CARTESIAN_POINT('Ctrl Pts',(1.63041148964996,-1.,3.40519422740596));
#35000=CARTESIAN_POINT('Ctrl Pts',(1.63316667054156,-1.,3.41272817148719));
#35001=CARTESIAN_POINT('Ctrl Pts',(1.63586250099804,-1.,3.4204397459095));
#35002=CARTESIAN_POINT('Ctrl Pts',(1.6383787624689,-1.,3.42804772926214));
#35003=CARTESIAN_POINT('Ctrl Pts',(1.64065778701952,-1.,3.43540451921397));
#35004=CARTESIAN_POINT('Ctrl Pts',(1.64270733821042,-1.,3.44250337701736));
#35005=CARTESIAN_POINT('Ctrl Pts',(1.64457408708059,-1.,3.44942242546693));
#35006=CARTESIAN_POINT('Ctrl Pts',(1.64632429697506,-1.,3.4562842106239));
#35007=CARTESIAN_POINT('Ctrl Pts',(1.64802323352752,-1.,3.46321237515029));
#35008=CARTESIAN_POINT('Ctrl Pts',(1.64971118698285,-1.,3.47028140996055));
#35009=CARTESIAN_POINT('Ctrl Pts',(1.65139534930353,-1.,3.47749926256543));
#35010=CARTESIAN_POINT('Ctrl Pts',(1.65306335367762,-1.,3.48483492840942));
#35011=CARTESIAN_POINT('Ctrl Pts',(1.65469162644476,-1.,3.49223525300194));
#35012=CARTESIAN_POINT('Ctrl Pts',(1.65625517961583,-1.,3.49964476477929));
#35013=CARTESIAN_POINT('Ctrl Pts',(1.65773832633617,-1.,3.5070273314651));
#35014=CARTESIAN_POINT('Ctrl Pts',(1.65913971687324,-1.,3.51437632188903));
#35015=CARTESIAN_POINT('Ctrl Pts',(1.66046645222266,-1.,3.52170261543787));
#35016=CARTESIAN_POINT('Ctrl Pts',(1.66173058912365,-1.,3.52902746211082));
#35017=CARTESIAN_POINT('Ctrl Pts',(1.66294490916113,-1.,3.53637385060225));
#35018=CARTESIAN_POINT('Ctrl Pts',(1.66411849222334,-1.,3.5437574747503));
#35019=CARTESIAN_POINT('Ctrl Pts',(1.66525401569004,-1.,3.5511812134288));
#35020=CARTESIAN_POINT('Ctrl Pts',(1.66635023293121,-1.,3.55864015233617));
#35021=CARTESIAN_POINT('Ctrl Pts',(1.66740349220308,-1.,3.56612465179429));
#35022=CARTESIAN_POINT('Ctrl Pts',(1.66840957407299,-1.,3.57362406285884));
#35023=CARTESIAN_POINT('Ctrl Pts',(1.66936552908228,-1.,3.58113044183823));
#35024=CARTESIAN_POINT('Ctrl Pts',(1.67027110397601,-1.,3.5886414309783));
#35025=CARTESIAN_POINT('Ctrl Pts',(1.67112775290706,-1.,3.59615824388808));
#35026=CARTESIAN_POINT('Ctrl Pts',(1.67193797318598,-1.,3.60368430815203));
#35027=CARTESIAN_POINT('Ctrl Pts',(1.67270452466968,-1.,3.61122367156182));
#35028=CARTESIAN_POINT('Ctrl Pts',(1.67342968196223,-1.,3.61877947398179));
#35029=CARTESIAN_POINT('Ctrl Pts',(1.67411452372265,-1.,3.62635249450908));
#35030=CARTESIAN_POINT('Ctrl Pts',(1.67475929882962,-1.,3.63394189312902));
#35031=CARTESIAN_POINT('Ctrl Pts',(1.67536373264839,-1.,3.6415458297232));
#35032=CARTESIAN_POINT('Ctrl Pts',(1.6759273594669,-1.,3.64916213574663));
#35033=CARTESIAN_POINT('Ctrl Pts',(1.67644983469459,-1.,3.65678894416442));
#35034=CARTESIAN_POINT('Ctrl Pts',(1.67693128053153,-1.,3.66442538671018));
#35035=CARTESIAN_POINT('Ctrl Pts',(1.67737217414901,-1.,3.67207136294639));
#35036=CARTESIAN_POINT('Ctrl Pts',(1.67777320475872,-1.,3.6797272457918));
#35037=CARTESIAN_POINT('Ctrl Pts',(1.67813513867973,-1.,3.68739360236505));
#35038=CARTESIAN_POINT('Ctrl Pts',(1.67845869064304,-1.,3.69507092759545));
#35039=CARTESIAN_POINT('Ctrl Pts',(1.6787443694862,-1.,3.70275932350998));
#35040=CARTESIAN_POINT('Ctrl Pts',(1.67899249793398,-1.,3.71045854208195));
#35041=CARTESIAN_POINT('Ctrl Pts',(1.6792032807165,-1.,3.71816812842188));
#35042=CARTESIAN_POINT('Ctrl Pts',(1.67937685856627,-1.,3.72588753416339));
#35043=CARTESIAN_POINT('Ctrl Pts',(1.67951336376434,-1.,3.73361623282617));
#35044=CARTESIAN_POINT('Ctrl Pts',(1.67961298685316,-1.,3.74135385965622));
#35045=CARTESIAN_POINT('Ctrl Pts',(1.67967598599665,-1.,3.74910022394845));
#35046=CARTESIAN_POINT('Ctrl Pts',(1.67970265841379,-1.,3.75685523754816));
#35047=CARTESIAN_POINT('Ctrl Pts',(1.67969332319322,-1.,3.76461886684523));
#35048=CARTESIAN_POINT('Ctrl Pts',(1.67964830084946,-1.,3.77239107928394));
#35049=CARTESIAN_POINT('Ctrl Pts',(1.67956789211943,-1.,3.78017178196859));
#35050=CARTESIAN_POINT('Ctrl Pts',(1.67945236653175,-1.,3.78796080021026));
#35051=CARTESIAN_POINT('Ctrl Pts',(1.67930196625203,-1.,3.7957579157763));
#35052=CARTESIAN_POINT('Ctrl Pts',(1.67911690648128,-1.,3.80356289078481));
#35053=CARTESIAN_POINT('Ctrl Pts',(1.67889737738311,-1.,3.81137549624273));
#35054=CARTESIAN_POINT('Ctrl Pts',(1.67864354606363,-1.,3.81919554100522));
#35055=CARTESIAN_POINT('Ctrl Pts',(1.67835555760094,-1.,3.82702289288453));
#35056=CARTESIAN_POINT('Ctrl Pts',(1.67803353065273,-1.,3.83485746516115));
#35057=CARTESIAN_POINT('Ctrl Pts',(1.67774874946867,-1.,3.8411308598706));
#35058=CARTESIAN_POINT('Ctrl Pts',(1.67751991140661,-1.,3.84583912297567));
#35059=CARTESIAN_POINT('Ctrl Pts',(1.6773605765671,-1.,3.84897939431104));
#35060=CARTESIAN_POINT('Ctrl Pts',(1.67727921511438,-1.,3.85054988729471));
#35061=CARTESIAN_POINT('',(1.53673442965255,-1.,3.90876544355381));
#35062=CARTESIAN_POINT('',(1.67727921511438,-1.,3.85054988729471));
#35063=CARTESIAN_POINT('',(1.24526366418208,-1.,3.5372048861591));
#35064=CARTESIAN_POINT('Ctrl Pts',(1.53673442965255,-1.,3.90876544355381));
#35065=CARTESIAN_POINT('Ctrl Pts',(1.53556639217742,-1.,3.90771246854607));
#35066=CARTESIAN_POINT('Ctrl Pts',(1.53323321827311,-1.,3.90560462812846));
#35067=CARTESIAN_POINT('Ctrl Pts',(1.5297421605556,-1.,3.90243719629755));
#35068=CARTESIAN_POINT('Ctrl Pts',(1.52510482990784,-1.,3.8982026070607));
#35069=CARTESIAN_POINT('Ctrl Pts',(1.51933724328609,-1.,3.89289043531893));
#35070=CARTESIAN_POINT('Ctrl Pts',(1.51359883110181,-1.,3.88755930032927));
#35071=CARTESIAN_POINT('Ctrl Pts',(1.50788973857719,-1.,3.88220917950443));
#35072=CARTESIAN_POINT('Ctrl Pts',(1.50221016176766,-1.,3.87684006372665));
#35073=CARTESIAN_POINT('Ctrl Pts',(1.4965603539944,-1.,3.8714519699927));
#35074=CARTESIAN_POINT('Ctrl Pts',(1.49094061164604,-1.,3.86604492575933));
#35075=CARTESIAN_POINT('Ctrl Pts',(1.48535125510102,-1.,3.86061894706551));
#35076=CARTESIAN_POINT('Ctrl Pts',(1.47979260991063,-1.,3.85517401698952));
#35077=CARTESIAN_POINT('Ctrl Pts',(1.47426499018467,-1.,3.84971006847096));
#35078=CARTESIAN_POINT('Ctrl Pts',(1.46876867426374,-1.,3.84422695454469));
#35079=CARTESIAN_POINT('Ctrl Pts',(1.46330391180621,-1.,3.83872447159309));
#35080=CARTESIAN_POINT('Ctrl Pts',(1.45787095220763,-1.,3.83320241775199));
#35081=CARTESIAN_POINT('Ctrl Pts',(1.45247006796807,-1.,3.82766064519));
#35082=CARTESIAN_POINT('Ctrl Pts',(1.44710157648562,-1.,3.82209910620591));
#35083=CARTESIAN_POINT('Ctrl Pts',(1.441765870414,-1.,3.8165179239855));
#35084=CARTESIAN_POINT('Ctrl Pts',(1.43646341556783,-1.,3.81091737726965));
#35085=CARTESIAN_POINT('Ctrl Pts',(1.43119469921364,-1.,3.80529775429916));
#35086=CARTESIAN_POINT('Ctrl Pts',(1.42596018777301,-1.,3.79965923196365));
#35087=CARTESIAN_POINT('Ctrl Pts',(1.42076028482828,-1.,3.7940017574439));
#35088=CARTESIAN_POINT('Ctrl Pts',(1.41559527803808,-1.,3.78832489879369));
#35089=CARTESIAN_POINT('Ctrl Pts',(1.41046532282567,-1.,3.78262780065406));
#35090=CARTESIAN_POINT('Ctrl Pts',(1.40537056004702,-1.,3.77690952014209));
#35091=CARTESIAN_POINT('Ctrl Pts',(1.40031121335495,-1.,3.77116930621804));
#35092=CARTESIAN_POINT('Ctrl Pts',(1.39528769118054,-1.,3.76540689249078));
#35093=CARTESIAN_POINT('Ctrl Pts',(1.39030069388926,-1.,3.75962280650875));
#35094=CARTESIAN_POINT('Ctrl Pts',(1.38535129801185,-1.,3.75381861212728));
#35095=CARTESIAN_POINT('Ctrl Pts',(1.38044070763302,-1.,3.74799617204744));
#35096=CARTESIAN_POINT('Ctrl Pts',(1.3755700297169,-1.,3.7421569816256));
#35097=CARTESIAN_POINT('Ctrl Pts',(1.37074003422739,-1.,3.73630145885809));
#35098=CARTESIAN_POINT('Ctrl Pts',(1.36595093298674,-1.,3.73042829011293));
#35099=CARTESIAN_POINT('Ctrl Pts',(1.36120211416353,-1.,3.72453364678279));
#35100=CARTESIAN_POINT('Ctrl Pts',(1.35649266705038,-1.,3.71861271513318));
#35101=CARTESIAN_POINT('Ctrl Pts',(1.35182193384426,-1.,3.71266130563061));
#35102=CARTESIAN_POINT('Ctrl Pts',(1.34719008463535,-1.,3.7066775318825));
#35103=CARTESIAN_POINT('Ctrl Pts',(1.3425986075293,-1.,3.70066324015112));
#35104=CARTESIAN_POINT('Ctrl Pts',(1.33805103398214,-1.,3.69462613305692));
#35105=CARTESIAN_POINT('Ctrl Pts',(1.33355191034515,-1.,3.68857672413013));
#35106=CARTESIAN_POINT('Ctrl Pts',(1.32910547072734,-1.,3.68252441182534));
#35107=CARTESIAN_POINT('Ctrl Pts',(1.32471430856413,-1.,3.67647355257906));
#35108=CARTESIAN_POINT('Ctrl Pts',(1.3203782813777,-1.,3.67042021752668));
#35109=CARTESIAN_POINT('Ctrl Pts',(1.31609271239922,-1.,3.66434688899822));
#35110=CARTESIAN_POINT('Ctrl Pts',(1.31185038411231,-1.,3.65822827358655));
#35111=CARTESIAN_POINT('Ctrl Pts',(1.30764479590051,-1.,3.65204081987101));
#35112=CARTESIAN_POINT('Ctrl Pts',(1.30347327603778,-1.,3.64577181380125));
#35113=CARTESIAN_POINT('Ctrl Pts',(1.29933955906463,-1.,3.6394268987279));
#35114=CARTESIAN_POINT('Ctrl Pts',(1.29525810207744,-1.,3.63304271630995));
#35115=CARTESIAN_POINT('Ctrl Pts',(1.29125046021853,-1.,3.62667616004299));
#35116=CARTESIAN_POINT('Ctrl Pts',(1.2873375502936,-1.,3.62038148492295));
#35117=CARTESIAN_POINT('Ctrl Pts',(1.28353255117754,-1.,3.61418935913793));
#35118=CARTESIAN_POINT('Ctrl Pts',(1.27983492861703,-1.,3.60808907746372));
#35119=CARTESIAN_POINT('Ctrl Pts',(1.27622049908664,-1.,3.60199947736404));
#35120=CARTESIAN_POINT('Ctrl Pts',(1.27264798379365,-1.,3.59578698050164));
#35121=CARTESIAN_POINT('Ctrl Pts',(1.26907758484766,-1.,3.5893180784647));
#35122=CARTESIAN_POINT('Ctrl Pts',(1.26548706249891,-1.,3.58250452868699));
#35123=CARTESIAN_POINT('Ctrl Pts',(1.26188667142784,-1.,3.5753456065164));
#35124=CARTESIAN_POINT('Ctrl Pts',(1.25834000485626,-1.,3.56798645995025));
#35125=CARTESIAN_POINT('Ctrl Pts',(1.25496090899873,-1.,3.56071094990825));
#35126=CARTESIAN_POINT('Ctrl Pts',(1.25188792940508,-1.,3.5538728741862));
#35127=CARTESIAN_POINT('Ctrl Pts',(1.24926408627938,-1.,3.54784190282889));
#35128=CARTESIAN_POINT('Ctrl Pts',(1.2472164623202,-1.,3.54294877426113));
#35129=CARTESIAN_POINT('Ctrl Pts',(1.24593497225964,-1.,3.53968291129942));
#35130=CARTESIAN_POINT('Ctrl Pts',(1.2453920538873,-1.,3.53808746578052));
#35131=CARTESIAN_POINT('Ctrl Pts',(1.24524498991133,-1.,3.53744859265385));
#35132=CARTESIAN_POINT('Ctrl Pts',(1.24524838931864,-1.,3.53725139174402));
#35133=CARTESIAN_POINT('Ctrl Pts',(1.24526366418208,-1.,3.5372048861591));
#35134=CARTESIAN_POINT('',(1.071677399622,-1.,3.59360648251021));
#35135=CARTESIAN_POINT('Origin',(0.,-1.,0.));
#35136=CARTESIAN_POINT('',(1.05427041296137,-1.,4.06552750530042));
#35137=CARTESIAN_POINT('Ctrl Pts',(1.071677399622,-1.,3.59360648251021));
#35138=CARTESIAN_POINT('Ctrl Pts',(1.07171709254271,-1.,3.59363512797985));
#35139=CARTESIAN_POINT('Ctrl Pts',(1.07183575450716,-1.,3.59379266874663));
#35140=CARTESIAN_POINT('Ctrl Pts',(1.07209229745284,-1.,3.59439597));
#35141=CARTESIAN_POINT('Ctrl Pts',(1.07259084660947,-1.,3.59600583195037));
#35142=CARTESIAN_POINT('Ctrl Pts',(1.0734737254567,-1.,3.59940121154383));
#35143=CARTESIAN_POINT('Ctrl Pts',(1.0746932716863,-1.,3.6045633988796));
#35144=CARTESIAN_POINT('Ctrl Pts',(1.07611545402841,-1.,3.61098481349577));
#35145=CARTESIAN_POINT('Ctrl Pts',(1.07764868137729,-1.,3.61832318504957));
#35146=CARTESIAN_POINT('Ctrl Pts',(1.07919137290815,-1.,3.62619537902616));
#35147=CARTESIAN_POINT('Ctrl Pts',(1.08064765719887,-1.,3.63423373196602));
#35148=CARTESIAN_POINT('Ctrl Pts',(1.08194278850972,-1.,3.64214167843595));
#35149=CARTESIAN_POINT('Ctrl Pts',(1.08304289898577,-1.,3.64976441208197));
#35150=CARTESIAN_POINT('Ctrl Pts',(1.08395671077761,-1.,3.65709649161004));
#35151=CARTESIAN_POINT('Ctrl Pts',(1.0847180992287,-1.,3.66422237895256));
#35152=CARTESIAN_POINT('Ctrl Pts',(1.0853733414448,-1.,3.67127347729632));
#35153=CARTESIAN_POINT('Ctrl Pts',(1.08596755755768,-1.,3.67838211685148));
#35154=CARTESIAN_POINT('Ctrl Pts',(1.08652888882609,-1.,3.68562817420864));
#35155=CARTESIAN_POINT('Ctrl Pts',(1.08706319540291,-1.,3.69302062410229));
#35156=CARTESIAN_POINT('Ctrl Pts',(1.08756311291324,-1.,3.70052690909884));
#35157=CARTESIAN_POINT('Ctrl Pts',(1.0880136731219,-1.,3.70809084139476));
#35158=CARTESIAN_POINT('Ctrl Pts',(1.08839887334776,-1.,3.71565372339063));
#35159=CARTESIAN_POINT('Ctrl Pts',(1.08870887220072,-1.,3.72317741369364));
#35160=CARTESIAN_POINT('Ctrl Pts',(1.08894337390925,-1.,3.73065515162949));
#35161=CARTESIAN_POINT('Ctrl Pts',(1.08910769013288,-1.,3.73809879348209));
#35162=CARTESIAN_POINT('Ctrl Pts',(1.08921040494013,-1.,3.74553121371745));
#35163=CARTESIAN_POINT('Ctrl Pts',(1.08926054632927,-1.,3.75297711748138));
#35164=CARTESIAN_POINT('Ctrl Pts',(1.08926462734287,-1.,3.76045342580226));
#35165=CARTESIAN_POINT('Ctrl Pts',(1.08922484204263,-1.,3.76796340094469));
#35166=CARTESIAN_POINT('Ctrl Pts',(1.08914072791275,-1.,3.7755019940944));
#35167=CARTESIAN_POINT('Ctrl Pts',(1.08901018614638,-1.,3.78305911299511));
#35168=CARTESIAN_POINT('Ctrl Pts',(1.08883071512097,-1.,3.79062357974401));
#35169=CARTESIAN_POINT('Ctrl Pts',(1.08860064435775,-1.,3.79818708705252));
#35170=CARTESIAN_POINT('Ctrl Pts',(1.08832009255378,-1.,3.80574726657656));
#35171=CARTESIAN_POINT('Ctrl Pts',(1.08799030610861,-1.,3.81330554446324));
#35172=CARTESIAN_POINT('Ctrl Pts',(1.08761321539442,-1.,3.82086569676321));
#35173=CARTESIAN_POINT('Ctrl Pts',(1.08719091307558,-1.,3.82843215316985));
#35174=CARTESIAN_POINT('Ctrl Pts',(1.08672515456901,-1.,3.83600837071702));
#35175=CARTESIAN_POINT('Ctrl Pts',(1.08621688337601,-1.,3.84359528764934));
#35176=CARTESIAN_POINT('Ctrl Pts',(1.08566647671838,-1.,3.85119211322732));
#35177=CARTESIAN_POINT('Ctrl Pts',(1.08507395120054,-1.,3.85879698702511));
#35178=CARTESIAN_POINT('Ctrl Pts',(1.08443918607926,-1.,3.86640769434269));
#35179=CARTESIAN_POINT('Ctrl Pts',(1.0837621330751,-1.,3.87402233722563));
#35180=CARTESIAN_POINT('Ctrl Pts',(1.08304304871042,-1.,3.88164007721365));
#35181=CARTESIAN_POINT('Ctrl Pts',(1.08228241999363,-1.,3.88926088975182));
#35182=CARTESIAN_POINT('Ctrl Pts',(1.08148086931373,-1.,3.89688525098408));
#35183=CARTESIAN_POINT('Ctrl Pts',(1.08063906483822,-1.,3.90451384092564));
#35184=CARTESIAN_POINT('Ctrl Pts',(1.0797576350746,-1.,3.91214726022096));
#35185=CARTESIAN_POINT('Ctrl Pts',(1.07883706663524,-1.,3.91978568924062));
#35186=CARTESIAN_POINT('Ctrl Pts',(1.07787771707155,-1.,3.92742893349684));
#35187=CARTESIAN_POINT('Ctrl Pts',(1.07687985975348,-1.,3.93507657572743));
#35188=CARTESIAN_POINT('Ctrl Pts',(1.07584371946428,-1.,3.94272809633271));
#35189=CARTESIAN_POINT('Ctrl Pts',(1.07476950921607,-1.,3.95038299600754));
#35190=CARTESIAN_POINT('Ctrl Pts',(1.07365747426551,-1.,3.95804094429606));
#35191=CARTESIAN_POINT('Ctrl Pts',(1.07250789943095,-1.,3.96570179322681));
#35192=CARTESIAN_POINT('Ctrl Pts',(1.07132109206252,-1.,3.97336550222571));
#35193=CARTESIAN_POINT('Ctrl Pts',(1.07009737257815,-1.,3.98103208801289));
#35194=CARTESIAN_POINT('Ctrl Pts',(1.06883706263912,-1.,3.98870156857298));
#35195=CARTESIAN_POINT('Ctrl Pts',(1.06754047381188,-1.,3.99637389919958));
#35196=CARTESIAN_POINT('Ctrl Pts',(1.06620789963406,-1.,4.00404894951804));
#35197=CARTESIAN_POINT('Ctrl Pts',(1.06483961342894,-1.,4.0117265418656));
#35198=CARTESIAN_POINT('Ctrl Pts',(1.06343586496094,-1.,4.0194064749539));
#35199=CARTESIAN_POINT('Ctrl Pts',(1.06199687787488,-1.,4.02708855235732));
#35200=CARTESIAN_POINT('Ctrl Pts',(1.06052284712114,-1.,4.03477261142549));
#35201=CARTESIAN_POINT('Ctrl Pts',(1.05901393667039,-1.,4.04245854429333));
#35202=CARTESIAN_POINT('Ctrl Pts',(1.05747027728537,-1.,4.05014628387112));
#35203=CARTESIAN_POINT('Ctrl Pts',(1.0562076270849,-1.,4.05629789308941));
#35204=CARTESIAN_POINT('Ctrl Pts',(1.05524507177901,-1.,4.06091239150293));
#35205=CARTESIAN_POINT('Ctrl Pts',(1.05459645194934,-1.,4.06398907542679));
#35206=CARTESIAN_POINT('Ctrl Pts',(1.05427041296137,-1.,4.06552750530042));
#35207=CARTESIAN_POINT('',(0.906349047628865,-1.,4.10104028313088));
#35208=CARTESIAN_POINT('',(1.05427041296137,-1.,4.06552750530042));
#35209=CARTESIAN_POINT('',(0.676591647975428,-1.,3.68845817949586));
#35210=CARTESIAN_POINT('Ctrl Pts',(0.906349047628865,-1.,4.10104028313088));
#35211=CARTESIAN_POINT('Ctrl Pts',(0.905360112215337,-1.,4.09981755067523));
#35212=CARTESIAN_POINT('Ctrl Pts',(0.903385402441587,-1.,4.09737067245935));
#35213=CARTESIAN_POINT('Ctrl Pts',(0.900432820941674,-1.,4.09369611522387));
#35214=CARTESIAN_POINT('Ctrl Pts',(0.896515019231333,-1.,4.08878822246833));
#35215=CARTESIAN_POINT('Ctrl Pts',(0.891649447916277,-1.,4.08263920304799));
#35216=CARTESIAN_POINT('Ctrl Pts',(0.886815658358501,-1.,4.07647601773635));
#35217=CARTESIAN_POINT('Ctrl Pts',(0.882013797525691,-1.,4.07029866694192));
#35218=CARTESIAN_POINT('Ctrl Pts',(0.877244060485837,-1.,4.06410717232905));
#35219=CARTESIAN_POINT('Ctrl Pts',(0.872506694782446,-1.,4.0579015903134));
#35220=CARTESIAN_POINT('Ctrl Pts',(0.867801988859917,-1.,4.05168199437909));
#35221=CARTESIAN_POINT('Ctrl Pts',(0.863130256643258,-1.,4.04544845048584));
#35222=CARTESIAN_POINT('Ctrl Pts',(0.858491822322827,-1.,4.03920099284773));
#35223=CARTESIAN_POINT('Ctrl Pts',(0.853887006631755,-1.,4.03293960436756));
#35224=CARTESIAN_POINT('Ctrl Pts',(0.849316107474244,-1.,4.02666418343164));
#35225=CARTESIAN_POINT('Ctrl Pts',(0.844779403287745,-1.,4.02037456798441));
#35226=CARTESIAN_POINT('Ctrl Pts',(0.840277171975854,-1.,4.01407059766103));
#35227=CARTESIAN_POINT('Ctrl Pts',(0.835809705809645,-1.,4.00775216907856));
#35228=CARTESIAN_POINT('Ctrl Pts',(0.831377325741622,-1.,4.00141928477507));
#35229=CARTESIAN_POINT('Ctrl Pts',(0.826980400320789,-1.,3.99507212784431));
#35230=CARTESIAN_POINT('Ctrl Pts',(0.822619346022118,-1.,3.98871104646485));
#35231=CARTESIAN_POINT('Ctrl Pts',(0.818294599022293,-1.,3.98233640155404));
#35232=CARTESIAN_POINT('Ctrl Pts',(0.814006592328843,-1.,3.97594844078811));
#35233=CARTESIAN_POINT('Ctrl Pts',(0.80975573281809,-1.,3.96954717513232));
#35234=CARTESIAN_POINT('Ctrl Pts',(0.805542372178361,-1.,3.96313222295815));
#35235=CARTESIAN_POINT('Ctrl Pts',(0.801366797727049,-1.,3.95670276375108));
#35236=CARTESIAN_POINT('Ctrl Pts',(0.797229296085315,-1.,3.95025788827136));
#35237=CARTESIAN_POINT('Ctrl Pts',(0.79313020564096,-1.,3.94379688971283));
#35238=CARTESIAN_POINT('Ctrl Pts',(0.789069971469332,-1.,3.93731956885676));
#35239=CARTESIAN_POINT('Ctrl Pts',(0.785049202786507,-1.,3.93082655631789));
#35240=CARTESIAN_POINT('Ctrl Pts',(0.781068718228451,-1.,3.92431956510441));
#35241=CARTESIAN_POINT('Ctrl Pts',(0.777129415664956,-1.,3.9178006233448));
#35242=CARTESIAN_POINT('Ctrl Pts',(0.77323215450632,-1.,3.91127138115243));
#35243=CARTESIAN_POINT('Ctrl Pts',(0.769377629847873,-1.,3.90473237182633));
#35244=CARTESIAN_POINT('Ctrl Pts',(0.765566256401295,-1.,3.89818233104378));
#35245=CARTESIAN_POINT('Ctrl Pts',(0.761798028793969,-1.,3.89161738162245));
#35246=CARTESIAN_POINT('Ctrl Pts',(0.758072800564801,-1.,3.88503262662689));
#35247=CARTESIAN_POINT('Ctrl Pts',(0.754390577396856,-1.,3.87842382520065));
#35248=CARTESIAN_POINT('Ctrl Pts',(0.750751822383027,-1.,3.87178914078374));
#35249=CARTESIAN_POINT('Ctrl Pts',(0.747157716488871,-1.,3.86513062969889));
#35250=CARTESIAN_POINT('Ctrl Pts',(0.743610542737012,-1.,3.85845645217594));
#35251=CARTESIAN_POINT('Ctrl Pts',(0.740113146827137,-1.,3.85177770351216));
#35252=CARTESIAN_POINT('Ctrl Pts',(0.736668240497117,-1.,3.84510432881213));
#35253=CARTESIAN_POINT('Ctrl Pts',(0.733277703756078,-1.,3.83844103658009));
#35254=CARTESIAN_POINT('Ctrl Pts',(0.729942010490167,-1.,3.83178392403383));
#35255=CARTESIAN_POINT('Ctrl Pts',(0.726659281876663,-1.,3.82511495756713));
#35256=CARTESIAN_POINT('Ctrl Pts',(0.723426346019422,-1.,3.81840802610835));
#35257=CARTESIAN_POINT('Ctrl Pts',(0.720240466589236,-1.,3.81163885127344));
#35258=CARTESIAN_POINT('Ctrl Pts',(0.717100993669114,-1.,3.80479445759309));
#35259=CARTESIAN_POINT('Ctrl Pts',(0.71401073300664,-1.,3.79788100314975));
#35260=CARTESIAN_POINT('Ctrl Pts',(0.710978231689016,-1.,3.79093694007094));
#35261=CARTESIAN_POINT('Ctrl Pts',(0.708015879375459,-1.,3.78402183336605));
#35262=CARTESIAN_POINT('Ctrl Pts',(0.705135847999816,-1.,3.77719254217129));
#35263=CARTESIAN_POINT('Ctrl Pts',(0.702346356621551,-1.,3.77048141872872));
#35264=CARTESIAN_POINT('Ctrl Pts',(0.699648552230917,-1.,3.76387780603759));
#35265=CARTESIAN_POINT('Ctrl Pts',(0.697031245659743,-1.,3.75729775767023));
#35266=CARTESIAN_POINT('Ctrl Pts',(0.694474562581492,-1.,3.75060288243455));
#35267=CARTESIAN_POINT('Ctrl Pts',(0.69196008040082,-1.,3.74365508986712));
#35268=CARTESIAN_POINT('Ctrl Pts',(0.689479637354813,-1.,3.73636374475077));
#35269=CARTESIAN_POINT('Ctrl Pts',(0.687043475232354,-1.,3.72872973554051));
#35270=CARTESIAN_POINT('Ctrl Pts',(0.684691698167848,-1.,3.7209063713926));
#35271=CARTESIAN_POINT('Ctrl Pts',(0.682492345108929,-1.,3.71319182789943));
#35272=CARTESIAN_POINT('Ctrl Pts',(0.680526909710876,-1.,3.70595722031785));
#35273=CARTESIAN_POINT('Ctrl Pts',(0.678878822226026,-1.,3.69959004073005));
#35274=CARTESIAN_POINT('Ctrl Pts',(0.677621861865497,-1.,3.69443683573598));
#35275=CARTESIAN_POINT('Ctrl Pts',(0.676867042599401,-1.,3.69101071175464));
#35276=CARTESIAN_POINT('Ctrl Pts',(0.676580391119396,-1.,3.68934997767243));
#35277=CARTESIAN_POINT('Ctrl Pts',(0.676535079520806,-1.,3.68869596425969));
#35278=CARTESIAN_POINT('Ctrl Pts',(0.676569286094606,-1.,3.68850172300477));
#35279=CARTESIAN_POINT('Ctrl Pts',(0.676591647975428,-1.,3.68845817949586));
#35280=CARTESIAN_POINT('',(0.496319364829373,-1.,3.71701050416802));
#35281=CARTESIAN_POINT('Origin',(0.,-1.,0.));
#35282=CARTESIAN_POINT('',(0.405301974318349,-1.,4.18039834341342));
#35283=CARTESIAN_POINT('Ctrl Pts',(0.496319364829373,-1.,3.71701050416802));
#35284=CARTESIAN_POINT('Ctrl Pts',(0.496354087925645,-1.,3.71704500630521));
#35285=CARTESIAN_POINT('Ctrl Pts',(0.496446644158827,-1.,3.71721917030465));
#35286=CARTESIAN_POINT('Ctrl Pts',(0.496605651526313,-1.,3.71785517607694));
#35287=CARTESIAN_POINT('Ctrl Pts',(0.496846224822534,-1.,3.7195232082259));
#35288=CARTESIAN_POINT('Ctrl Pts',(0.497187079575794,-1.,3.72301489774241));
#35289=CARTESIAN_POINT('Ctrl Pts',(0.497584067153279,-1.,3.72830430904794));
#35290=CARTESIAN_POINT('Ctrl Pts',(0.497984209510495,-1.,3.73486914372834));
#35291=CARTESIAN_POINT('Ctrl Pts',(0.498350586058176,-1.,3.74235701735109));
#35292=CARTESIAN_POINT('Ctrl Pts',(0.498642802042929,-1.,3.75037362168103));
#35293=CARTESIAN_POINT('Ctrl Pts',(0.498823681615513,-1.,3.75854082221127));
#35294=CARTESIAN_POINT('Ctrl Pts',(0.498865792335185,-1.,3.76655401191144));
#35295=CARTESIAN_POINT('Ctrl Pts',(0.498759900365686,-1.,3.77425499225089));
#35296=CARTESIAN_POINT('Ctrl Pts',(0.498515471679378,-1.,3.78163975337189));
#35297=CARTESIAN_POINT('Ctrl Pts',(0.498152751800819,-1.,3.78879701661152));
#35298=CARTESIAN_POINT('Ctrl Pts',(0.49769689210058,-1.,3.79586380669959));
#35299=CARTESIAN_POINT('Ctrl Pts',(0.49717175620109,-1.,3.80297788298545));
#35300=CARTESIAN_POINT('Ctrl Pts',(0.496592643443789,-1.,3.81022254090909));
#35301=CARTESIAN_POINT('Ctrl Pts',(0.495963937875571,-1.,3.81760756144099));
#35302=CARTESIAN_POINT('Ctrl Pts',(0.495283458893903,-1.,3.82509963594156));
#35303=CARTESIAN_POINT('Ctrl Pts',(0.494545212256425,-1.,3.8326409268245));
#35304=CARTESIAN_POINT('Ctrl Pts',(0.493742574629117,-1.,3.84017095578438));
#35305=CARTESIAN_POINT('Ctrl Pts',(0.492871792414095,-1.,3.84765051147965));
#35306=CARTESIAN_POINT('Ctrl Pts',(0.49193363108376,-1.,3.85507287020223));
#35307=CARTESIAN_POINT('Ctrl Pts',(0.490931482170849,-1.,3.86245057319215));
#35308=CARTESIAN_POINT('Ctrl Pts',(0.489870245704899,-1.,3.86980755613694));
#35309=CARTESIAN_POINT('Ctrl Pts',(0.488754973798281,-1.,3.87716963231115));
#35310=CARTESIAN_POINT('Ctrl Pts',(0.487589452275179,-1.,3.88455453328156));
#35311=CARTESIAN_POINT('Ctrl Pts',(0.486375337854133,-1.,3.89196582437574));
#35312=CARTESIAN_POINT('Ctrl Pts',(0.485112963522245,-1.,3.89939844658529));
#35313=CARTESIAN_POINT('Ctrl Pts',(0.48380183508916,-1.,3.90684210358063));
#35314=CARTESIAN_POINT('Ctrl Pts',(0.482441230340708,-1.,3.91428536373749));
#35315=CARTESIAN_POINT('Ctrl Pts',(0.481030798910735,-1.,3.92171976072334));
#35316=CARTESIAN_POINT('Ctrl Pts',(0.479571028525565,-1.,3.92914297392067));
#35317=CARTESIAN_POINT('Ctrl Pts',(0.478062927140957,-1.,3.93655660689819));
#35318=CARTESIAN_POINT('Ctrl Pts',(0.476507810658534,-1.,3.94396469119385));
#35319=CARTESIAN_POINT('Ctrl Pts',(0.47490705302179,-1.,3.95137192932898));
#35320=CARTESIAN_POINT('Ctrl Pts',(0.473261847236295,-1.,3.95878201038332));
#35321=CARTESIAN_POINT('Ctrl Pts',(0.471572978413493,-1.,3.96619600864626));
#35322=CARTESIAN_POINT('Ctrl Pts',(0.469840942829878,-1.,3.97361320212413));
#35323=CARTESIAN_POINT('Ctrl Pts',(0.468066047920139,-1.,3.98103175589349));
#35324=CARTESIAN_POINT('Ctrl Pts',(0.466248520883034,-1.,3.98844946363258));
#35325=CARTESIAN_POINT('Ctrl Pts',(0.464388610938994,-1.,3.99586444320135));
#35326=CARTESIAN_POINT('Ctrl Pts',(0.462486702616251,-1.,4.00327590659129));
#35327=CARTESIAN_POINT('Ctrl Pts',(0.460543280768577,-1.,4.01068390573469));
#35328=CARTESIAN_POINT('Ctrl Pts',(0.458558885637,-1.,4.01808900827647));
#35329=CARTESIAN_POINT('Ctrl Pts',(0.456534070784968,-1.,4.02549199038414));
#35330=CARTESIAN_POINT('Ctrl Pts',(0.454469363020495,-1.,4.03289354362745));
#35331=CARTESIAN_POINT('Ctrl Pts',(0.452365214748778,-1.,4.0402939222793));
#35332=CARTESIAN_POINT('Ctrl Pts',(0.450222009543773,-1.,4.0476929901797));
#35333=CARTESIAN_POINT('Ctrl Pts',(0.448040082683976,-1.,4.05509037796815));
#35334=CARTESIAN_POINT('Ctrl Pts',(0.445819737468477,-1.,4.06248560760596));
#35335=CARTESIAN_POINT('Ctrl Pts',(0.443561262395407,-1.,4.0698782192577));
#35336=CARTESIAN_POINT('Ctrl Pts',(0.441264951396587,-1.,4.07726792490256));
#35337=CARTESIAN_POINT('Ctrl Pts',(0.438931108931613,-1.,4.08465462294625));
#35338=CARTESIAN_POINT('Ctrl Pts',(0.436560044913814,-1.,4.09203832139439));
#35339=CARTESIAN_POINT('Ctrl Pts',(0.434152073200642,-1.,4.09941908688567));
#35340=CARTESIAN_POINT('Ctrl Pts',(0.431707508679771,-1.,4.10679698750219));
#35341=CARTESIAN_POINT('Ctrl Pts',(0.429226666075372,-1.,4.1141720278277));
#35342=CARTESIAN_POINT('Ctrl Pts',(0.426709855706242,-1.,4.1215441250121));
#35343=CARTESIAN_POINT('Ctrl Pts',(0.424157375323155,-1.,4.1289131463371));
#35344=CARTESIAN_POINT('Ctrl Pts',(0.421569503103971,-1.,4.13627893206433));
#35345=CARTESIAN_POINT('Ctrl Pts',(0.418946490667799,-1.,4.14364132317223));
#35346=CARTESIAN_POINT('Ctrl Pts',(0.416288556008986,-1.,4.15100018950989));
#35347=CARTESIAN_POINT('Ctrl Pts',(0.413595877953268,-1.,4.1583554501909));
#35348=CARTESIAN_POINT('Ctrl Pts',(0.410868596148613,-1.,4.16570705940731));
#35349=CARTESIAN_POINT('Ctrl Pts',(0.408659167570152,-1.,4.17158541009947));
#35350=CARTESIAN_POINT('Ctrl Pts',(0.406986596326602,-1.,4.17599251955585));
#35351=CARTESIAN_POINT('Ctrl Pts',(0.40586466267963,-1.,4.17892985789908));
#35352=CARTESIAN_POINT('Ctrl Pts',(0.405301974318349,-1.,4.18039834341342));
#35353=CARTESIAN_POINT('',(0.253646344052521,-1.,4.1923339003649));
#35354=CARTESIAN_POINT('',(0.405301974318349,-1.,4.18039834341342));
#35355=CARTESIAN_POINT('',(0.091259699916682,-1.,3.74888939116255));
#35356=CARTESIAN_POINT('Ctrl Pts',(0.253646344052521,-1.,4.1923339003649));
#35357=CARTESIAN_POINT('Ctrl Pts',(0.252860861572565,-1.,4.19097151819241));
#35358=CARTESIAN_POINT('Ctrl Pts',(0.251293239837692,-1.,4.18824585244066));
#35359=CARTESIAN_POINT('Ctrl Pts',(0.248951836910963,-1.,4.18415464959491));
#35360=CARTESIAN_POINT('Ctrl Pts',(0.245850033418583,-1.,4.17869430192868));
#35361=CARTESIAN_POINT('Ctrl Pts',(0.242006283923911,-1.,4.17185984409533));
#35362=CARTESIAN_POINT('Ctrl Pts',(0.238196140933976,-1.,4.1650163665385));
#35363=CARTESIAN_POINT('Ctrl Pts',(0.234419749543142,-1.,4.1581638926525));
#35364=CARTESIAN_POINT('Ctrl Pts',(0.230677299028737,-1.,4.15130247435029));
#35365=CARTESIAN_POINT('Ctrl Pts',(0.226969025061243,-1.,4.14443220607733));
#35366=CARTESIAN_POINT('Ctrl Pts',(0.223295201038383,-1.,4.13755320553563));
#35367=CARTESIAN_POINT('Ctrl Pts',(0.219656126701851,-1.,4.13066558698156));
#35368=CARTESIAN_POINT('Ctrl Pts',(0.216052116898424,-1.,4.12376943492249));
#35369=CARTESIAN_POINT('Ctrl Pts',(0.212483491087067,-1.,4.11686478264545));
#35370=CARTESIAN_POINT('Ctrl Pts',(0.208950559400171,-1.,4.10995157639026));
#35371=CARTESIAN_POINT('Ctrl Pts',(0.205453622198233,-1.,4.10302969965374));
#35372=CARTESIAN_POINT('Ctrl Pts',(0.201992979049984,-1.,4.09609903751912));
#35373=CARTESIAN_POINT('Ctrl Pts',(0.19856893480081,-1.,4.08915953359753));
#35374=CARTESIAN_POINT('Ctrl Pts',(0.195181806054714,-1.,4.08221124060385));
#35375=CARTESIAN_POINT('Ctrl Pts',(0.191831928181081,-1.,4.07525439703137));
#35376=CARTESIAN_POINT('Ctrl Pts',(0.188519658060255,-1.,4.06828941192308));
#35377=CARTESIAN_POINT('Ctrl Pts',(0.185245370038947,-1.,4.06131670998589));
#35378=CARTESIAN_POINT('Ctrl Pts',(0.18200945304855,-1.,4.05433660358402));
#35379=CARTESIAN_POINT('Ctrl Pts',(0.178812307240715,-1.,4.04734916719722));
#35380=CARTESIAN_POINT('Ctrl Pts',(0.175654339673757,-1.,4.04035407891161));
#35381=CARTESIAN_POINT('Ctrl Pts',(0.172535962484466,-1.,4.03335057326093));
#35382=CARTESIAN_POINT('Ctrl Pts',(0.169457601001653,-1.,4.0263377970371));
#35383=CARTESIAN_POINT('Ctrl Pts',(0.166419700015847,-1.,4.01931510507143));
#35384=CARTESIAN_POINT('Ctrl Pts',(0.163422730287458,-1.,4.01228237022301));
#35385=CARTESIAN_POINT('Ctrl Pts',(0.160467194882218,-1.,4.00524031064509));
#35386=CARTESIAN_POINT('Ctrl Pts',(0.157553634383809,-1.,3.99819074631874));
#35387=CARTESIAN_POINT('Ctrl Pts',(0.154682618338563,-1.,3.99113582086059));
#35388=CARTESIAN_POINT('Ctrl Pts',(0.151854737441405,-1.,3.9840772985098));
#35389=CARTESIAN_POINT('Ctrl Pts',(0.149070594803543,-1.,3.97701581473643));
#35390=CARTESIAN_POINT('Ctrl Pts',(0.146330797814513,-1.,3.96995018565891));
#35391=CARTESIAN_POINT('Ctrl Pts',(0.143635947692791,-1.,3.96287658098896));
#35392=CARTESIAN_POINT('Ctrl Pts',(0.140986665829936,-1.,3.95579014116899));
#35393=CARTESIAN_POINT('Ctrl Pts',(0.138383621255159,-1.,3.94868667844355));
#35394=CARTESIAN_POINT('Ctrl Pts',(0.135827558661187,-1.,3.94156445130744));
#35395=CARTESIAN_POINT('Ctrl Pts',(0.133319322794189,-1.,3.93442567551035));
#35396=CARTESIAN_POINT('Ctrl Pts',(0.130859892027798,-1.,3.9272787679596));
#35397=CARTESIAN_POINT('Ctrl Pts',(0.128450341339527,-1.,3.92013513251642));
#35398=CARTESIAN_POINT('Ctrl Pts',(0.126091793324136,-1.,3.91300501605392));
#35399=CARTESIAN_POINT('Ctrl Pts',(0.123785368272377,-1.,3.90589336320508));
#35400=CARTESIAN_POINT('Ctrl Pts',(0.121532144765723,-1.,3.89879639336952));
#35401=CARTESIAN_POINT('Ctrl Pts',(0.119333088190417,-1.,3.89169600105201));
#35402=CARTESIAN_POINT('Ctrl Pts',(0.117189150373144,-1.,3.88456590045767));
#35403=CARTESIAN_POINT('Ctrl Pts',(0.115101426649469,-1.,3.87738168405343));
#35404=CARTESIAN_POINT('Ctrl Pts',(0.113071304914561,-1.,3.87013043445014));
#35405=CARTESIAN_POINT('Ctrl Pts',(0.11110059303626,-1.,3.86281867282965));
#35406=CARTESIAN_POINT('Ctrl Pts',(0.109191717634943,-1.,3.855485714969));
#35407=CARTESIAN_POINT('Ctrl Pts',(0.107347597812183,-1.,3.84819233070317));
#35408=CARTESIAN_POINT('Ctrl Pts',(0.105571360916569,-1.,3.84099658324803));
#35409=CARTESIAN_POINT('Ctrl Pts',(0.103866063811622,-1.,3.83393171228002));
#35410=CARTESIAN_POINT('Ctrl Pts',(0.102234506488456,-1.,3.82698737143255));
#35411=CARTESIAN_POINT('Ctrl Pts',(0.100678769650632,-1.,3.82007889742625));
#35412=CARTESIAN_POINT('Ctrl Pts',(0.0992008728096511,-1.,3.81306649386461));
#35413=CARTESIAN_POINT('Ctrl Pts',(0.097804222290664,-1.,3.80581088847809));
#35414=CARTESIAN_POINT('Ctrl Pts',(0.0964949352873128,-1.,3.79822128513845));
#35415=CARTESIAN_POINT('Ctrl Pts',(0.0952829885100798,-1.,3.79030016353111));
#35416=CARTESIAN_POINT('Ctrl Pts',(0.0941840095090811,-1.,3.782205218991));
#35417=CARTESIAN_POINT('Ctrl Pts',(0.0932185546203175,-1.,3.77424159971059));
#35418=CARTESIAN_POINT('Ctrl Pts',(0.0924090589602688,-1.,3.76678860031841));
#35419=CARTESIAN_POINT('Ctrl Pts',(0.0917773084998332,-1.,3.76024199359303));
#35420=CARTESIAN_POINT('Ctrl Pts',(0.0913419622736395,-1.,3.75495560118212));
#35421=CARTESIAN_POINT('Ctrl Pts',(0.0911323999574423,-1.,3.75145357872422));
#35422=CARTESIAN_POINT('Ctrl Pts',(0.0911090736805507,-1.,3.74976844886346));
#35423=CARTESIAN_POINT('Ctrl Pts',(0.0911666301812815,-1.,3.74911539914542));
#35424=CARTESIAN_POINT('Ctrl Pts',(0.0912308016421979,-1.,3.74892890040975));
#35425=CARTESIAN_POINT('Ctrl Pts',(0.091259699916682,-1.,3.74888939116255));
#35426=CARTESIAN_POINT('',(-0.091259699914886,-1.,3.74888939116259));
#35427=CARTESIAN_POINT('Origin',(0.,-1.,0.));
#35428=CARTESIAN_POINT('',(-0.253646344052522,-1.,4.1923339003649));
#35429=CARTESIAN_POINT('Ctrl Pts',(-0.091259699914886,-1.,3.74888939116259));
#35430=CARTESIAN_POINT('Ctrl Pts',(-0.0912308016409234,-1.,3.74892890041021));
#35431=CARTESIAN_POINT('Ctrl Pts',(-0.0911666301806427,-1.,3.74911539914664));
#35432=CARTESIAN_POINT('Ctrl Pts',(-0.0911090736804572,-1.,3.74976844886495));
#35433=CARTESIAN_POINT('Ctrl Pts',(-0.0911323999576145,-1.,3.75145357872511));
#35434=CARTESIAN_POINT('Ctrl Pts',(-0.0913419622735854,-1.,3.75495560118053));
#35435=CARTESIAN_POINT('Ctrl Pts',(-0.091777308499901,-1.,3.76024199359493));
#35436=CARTESIAN_POINT('Ctrl Pts',(-0.0924090589604057,-1.,3.76678860032228));
#35437=CARTESIAN_POINT('Ctrl Pts',(-0.0932185546204576,-1.,3.77424159971456));
#35438=CARTESIAN_POINT('Ctrl Pts',(-0.0941840095091746,-1.,3.78220521899366));
#35439=CARTESIAN_POINT('Ctrl Pts',(-0.095282988510107,-1.,3.79030016353186));
#35440=CARTESIAN_POINT('Ctrl Pts',(-0.0964949352872846,-1.,3.7982212851376));
#35441=CARTESIAN_POINT('Ctrl Pts',(-0.0978042222906077,-1.,3.80581088847642));
#35442=CARTESIAN_POINT('Ctrl Pts',(-0.0992008728095946,-1.,3.81306649386293));
#35443=CARTESIAN_POINT('Ctrl Pts',(-0.100678769650594,-1.,3.82007889742512));
#35444=CARTESIAN_POINT('Ctrl Pts',(-0.102234506488445,-1.,3.8269873714322));
#35445=CARTESIAN_POINT('Ctrl Pts',(-0.103866063811634,-1.,3.83393171228034));
#35446=CARTESIAN_POINT('Ctrl Pts',(-0.105571360916593,-1.,3.84099658324873));
#35447=CARTESIAN_POINT('Ctrl Pts',(-0.107347597812208,-1.,3.84819233070391));
#35448=CARTESIAN_POINT('Ctrl Pts',(-0.109191717634961,-1.,3.85548571496953));
#35449=CARTESIAN_POINT('Ctrl Pts',(-0.111100593036267,-1.,3.86281867282984));
#35450=CARTESIAN_POINT('Ctrl Pts',(-0.113071304914559,-1.,3.87013043445001));
#35451=CARTESIAN_POINT('Ctrl Pts',(-0.115101426649461,-1.,3.87738168405308));
#35452=CARTESIAN_POINT('Ctrl Pts',(-0.117189150373134,-1.,3.88456590045726));
#35453=CARTESIAN_POINT('Ctrl Pts',(-0.11933308819041,-1.,3.8916960010517));
#35454=CARTESIAN_POINT('Ctrl Pts',(-0.121532144765721,-1.,3.89879639336939));
#35455=CARTESIAN_POINT('Ctrl Pts',(-0.12378536827238,-1.,3.90589336320515));
#35456=CARTESIAN_POINT('Ctrl Pts',(-0.126091793324141,-1.,3.91300501605411));
#35457=CARTESIAN_POINT('Ctrl Pts',(-0.128450341339532,-1.,3.92013513251664));
#35458=CARTESIAN_POINT('Ctrl Pts',(-0.130859892027802,-1.,3.92727876795977));
#35459=CARTESIAN_POINT('Ctrl Pts',(-0.133319322794191,-1.,3.93442567551042));
#35460=CARTESIAN_POINT('Ctrl Pts',(-0.135827558661188,-1.,3.94156445130741));
#35461=CARTESIAN_POINT('Ctrl Pts',(-0.138383621255161,-1.,3.94868667844347));
#35462=CARTESIAN_POINT('Ctrl Pts',(-0.140986665829942,-1.,3.95579014116894));
#35463=CARTESIAN_POINT('Ctrl Pts',(-0.143635947692799,-1.,3.96287658098896));
#35464=CARTESIAN_POINT('Ctrl Pts',(-0.14633079781452,-1.,3.96995018565893));
#35465=CARTESIAN_POINT('Ctrl Pts',(-0.149070594803545,-1.,3.97701581473644));
#35466=CARTESIAN_POINT('Ctrl Pts',(-0.151854737441398,-1.,3.98407729850975));
#35467=CARTESIAN_POINT('Ctrl Pts',(-0.154682618338548,-1.,3.99113582086043));
#35468=CARTESIAN_POINT('Ctrl Pts',(-0.15755363438379,-1.,3.9981907463185));
#35469=CARTESIAN_POINT('Ctrl Pts',(-0.160467194882203,-1.,4.00524031064487));
#35470=CARTESIAN_POINT('Ctrl Pts',(-0.163422730287457,-1.,4.01228237022296));
#35471=CARTESIAN_POINT('Ctrl Pts',(-0.166419700015866,-1.,4.01931510507167));
#35472=CARTESIAN_POINT('Ctrl Pts',(-0.169457601001691,-1.,4.02633779703764));
#35473=CARTESIAN_POINT('Ctrl Pts',(-0.172535962484514,-1.,4.03335057326163));
#35474=CARTESIAN_POINT('Ctrl Pts',(-0.175654339673798,-1.,4.04035407891222));
#35475=CARTESIAN_POINT('Ctrl Pts',(-0.178812307240729,-1.,4.04734916719741));
#35476=CARTESIAN_POINT('Ctrl Pts',(-0.18200945304852,-1.,4.05433660358353));
#35477=CARTESIAN_POINT('Ctrl Pts',(-0.185245370038874,-1.,4.06131670998469));
#35478=CARTESIAN_POINT('Ctrl Pts',(-0.188519658060156,-1.,4.06828941192148));
#35479=CARTESIAN_POINT('Ctrl Pts',(-0.191831928180991,-1.,4.07525439702992));
#35480=CARTESIAN_POINT('Ctrl Pts',(-0.195181806054676,-1.,4.08221124060322));
#35481=CARTESIAN_POINT('Ctrl Pts',(-0.198568934800862,-1.,4.08915953359833));
#35482=CARTESIAN_POINT('Ctrl Pts',(-0.201992979050136,-1.,4.09609903752152));
#35483=CARTESIAN_POINT('Ctrl Pts',(-0.205453622198455,-1.,4.10302969965728));
#35484=CARTESIAN_POINT('Ctrl Pts',(-0.208950559400393,-1.,4.10995157639377));
#35485=CARTESIAN_POINT('Ctrl Pts',(-0.21248349108719,-1.,4.11686478264739));
#35486=CARTESIAN_POINT('Ctrl Pts',(-0.216052116898352,-1.,4.12376943492132));
#35487=CARTESIAN_POINT('Ctrl Pts',(-0.219656126701542,-1.,4.13066558697658));
#35488=CARTESIAN_POINT('Ctrl Pts',(-0.223295201037886,-1.,4.13755320552764));
#35489=CARTESIAN_POINT('Ctrl Pts',(-0.226969025060705,-1.,4.14443220606869));
#35490=CARTESIAN_POINT('Ctrl Pts',(-0.230677299028383,-1.,4.15130247434459));
#35491=CARTESIAN_POINT('Ctrl Pts',(-0.234419749543208,-1.,4.15816389265352));
#35492=CARTESIAN_POINT('Ctrl Pts',(-0.238196140934616,-1.,4.16501636654877));
#35493=CARTESIAN_POINT('Ctrl Pts',(-0.242006283925089,-1.,4.17185984411426));
#35494=CARTESIAN_POINT('Ctrl Pts',(-0.245850033420019,-1.,4.1786943019518));
#35495=CARTESIAN_POINT('Ctrl Pts',(-0.248951836912189,-1.,4.18415464961466));
#35496=CARTESIAN_POINT('Ctrl Pts',(-0.251293239838441,-1.,4.18824585245272));
#35497=CARTESIAN_POINT('Ctrl Pts',(-0.252860861572841,-1.,4.19097151819684));
#35498=CARTESIAN_POINT('Ctrl Pts',(-0.253646344052522,-1.,4.1923339003649));
#35499=CARTESIAN_POINT('',(-0.40530197431835,-1.,4.18039834341342));
#35500=CARTESIAN_POINT('',(-0.253646344052522,-1.,4.1923339003649));
#35501=CARTESIAN_POINT('',(-0.496319364827592,-1.,3.71701050416825));
#35502=CARTESIAN_POINT('Ctrl Pts',(-0.40530197431835,-1.,4.18039834341342));
#35503=CARTESIAN_POINT('Ctrl Pts',(-0.40586466267921,-1.,4.17892985789466));
#35504=CARTESIAN_POINT('Ctrl Pts',(-0.406986596325455,-1.,4.17599251954382));
#35505=CARTESIAN_POINT('Ctrl Pts',(-0.408659167568273,-1.,4.17158541007977));
#35506=CARTESIAN_POINT('Ctrl Pts',(-0.410868596146414,-1.,4.16570705938425));
#35507=CARTESIAN_POINT('Ctrl Pts',(-0.41359587795147,-1.,4.15835545017202));
#35508=CARTESIAN_POINT('Ctrl Pts',(-0.416288556008012,-1.,4.15100018949965));
#35509=CARTESIAN_POINT('Ctrl Pts',(-0.418946490667703,-1.,4.14364132317121));
#35510=CARTESIAN_POINT('Ctrl Pts',(-0.421569503104513,-1.,4.13627893207002));
#35511=CARTESIAN_POINT('Ctrl Pts',(-0.424157375323975,-1.,4.12891314634572));
#35512=CARTESIAN_POINT('Ctrl Pts',(-0.426709855707001,-1.,4.12154412502007));
#35513=CARTESIAN_POINT('Ctrl Pts',(-0.429226666075845,-1.,4.11417202783267));
#35514=CARTESIAN_POINT('Ctrl Pts',(-0.431707508679884,-1.,4.10679698750336));
#35515=CARTESIAN_POINT('Ctrl Pts',(-0.43415207320046,-1.,4.09941908688373));
#35516=CARTESIAN_POINT('Ctrl Pts',(-0.436560044913482,-1.,4.09203832139089));
#35517=CARTESIAN_POINT('Ctrl Pts',(-0.43893110893128,-1.,4.08465462294273));
#35518=CARTESIAN_POINT('Ctrl Pts',(-0.441264951396361,-1.,4.07726792490016));
#35519=CARTESIAN_POINT('Ctrl Pts',(-0.443561262395333,-1.,4.0698782192569));
#35520=CARTESIAN_POINT('Ctrl Pts',(-0.445819737468538,-1.,4.06248560760659));
#35521=CARTESIAN_POINT('Ctrl Pts',(-0.448040082684115,-1.,4.0550903779696));
#35522=CARTESIAN_POINT('Ctrl Pts',(-0.450222009543927,-1.,4.0476929901813));
#35523=CARTESIAN_POINT('Ctrl Pts',(-0.452365214748893,-1.,4.04029392228049));
#35524=CARTESIAN_POINT('Ctrl Pts',(-0.454469363020542,-1.,4.03289354362794));
#35525=CARTESIAN_POINT('Ctrl Pts',(-0.456534070784951,-1.,4.02549199038394));
#35526=CARTESIAN_POINT('Ctrl Pts',(-0.458558885636946,-1.,4.01808900827587));
#35527=CARTESIAN_POINT('Ctrl Pts',(-0.460543280768515,-1.,4.01068390573399));
#35528=CARTESIAN_POINT('Ctrl Pts',(-0.462486702616205,-1.,4.00327590659075));
#35529=CARTESIAN_POINT('Ctrl Pts',(-0.464388610938975,-1.,3.9958644432011));
#35530=CARTESIAN_POINT('Ctrl Pts',(-0.46624852088304,-1.,3.98844946363262));
#35531=CARTESIAN_POINT('Ctrl Pts',(-0.468066047920157,-1.,3.98103175589371));
#35532=CARTESIAN_POINT('Ctrl Pts',(-0.469840942829896,-1.,3.97361320212436));
#35533=CARTESIAN_POINT('Ctrl Pts',(-0.471572978413504,-1.,3.96619600864643));
#35534=CARTESIAN_POINT('Ctrl Pts',(-0.473261847236297,-1.,3.95878201038338));
#35535=CARTESIAN_POINT('Ctrl Pts',(-0.47490705302179,-1.,3.95137192932897));
#35536=CARTESIAN_POINT('Ctrl Pts',(-0.476507810658537,-1.,3.94396469119383));
#35537=CARTESIAN_POINT('Ctrl Pts',(-0.478062927140965,-1.,3.93655660689819));
#35538=CARTESIAN_POINT('Ctrl Pts',(-0.479571028525579,-1.,3.92914297392071));
#35539=CARTESIAN_POINT('Ctrl Pts',(-0.481030798910748,-1.,3.92171976072341));
#35540=CARTESIAN_POINT('Ctrl Pts',(-0.482441230340713,-1.,3.91428536373751));
#35541=CARTESIAN_POINT('Ctrl Pts',(-0.48380183508915,-1.,3.90684210358056));
#35542=CARTESIAN_POINT('Ctrl Pts',(-0.485112963522222,-1.,3.89939844658513));
#35543=CARTESIAN_POINT('Ctrl Pts',(-0.486375337854103,-1.,3.89196582437552));
#35544=CARTESIAN_POINT('Ctrl Pts',(-0.487589452275155,-1.,3.88455453328138));
#35545=CARTESIAN_POINT('Ctrl Pts',(-0.488754973798274,-1.,3.87716963231109));
#35546=CARTESIAN_POINT('Ctrl Pts',(-0.489870245704918,-1.,3.86980755613707));
#35547=CARTESIAN_POINT('Ctrl Pts',(-0.490931482170891,-1.,3.86245057319246));
#35548=CARTESIAN_POINT('Ctrl Pts',(-0.491933631083813,-1.,3.85507287020263));
#35549=CARTESIAN_POINT('Ctrl Pts',(-0.492871792414141,-1.,3.84765051147999));
#35550=CARTESIAN_POINT('Ctrl Pts',(-0.493742574629135,-1.,3.84017095578451));
#35551=CARTESIAN_POINT('Ctrl Pts',(-0.494545212256401,-1.,3.83264092682431));
#35552=CARTESIAN_POINT('Ctrl Pts',(-0.495283458893837,-1.,3.82509963594103));
#35553=CARTESIAN_POINT('Ctrl Pts',(-0.49596393787548,-1.,3.81760756144025));
#35554=CARTESIAN_POINT('Ctrl Pts',(-0.496592643443704,-1.,3.81022254090839));
#35555=CARTESIAN_POINT('Ctrl Pts',(-0.497171756201052,-1.,3.80297788298514));
#35556=CARTESIAN_POINT('Ctrl Pts',(-0.497696892100625,-1.,3.79586380669994));
#35557=CARTESIAN_POINT('Ctrl Pts',(-0.498152751800958,-1.,3.78879701661264));
#35558=CARTESIAN_POINT('Ctrl Pts',(-0.498515471679585,-1.,3.78163975337356));
#35559=CARTESIAN_POINT('Ctrl Pts',(-0.498759900365892,-1.,3.77425499225255));
#35560=CARTESIAN_POINT('Ctrl Pts',(-0.498865792335291,-1.,3.76655401191229));
#35561=CARTESIAN_POINT('Ctrl Pts',(-0.498823681615422,-1.,3.75854082221053));
#35562=CARTESIAN_POINT('Ctrl Pts',(-0.498642802042606,-1.,3.75037362167839));
#35563=CARTESIAN_POINT('Ctrl Pts',(-0.498350586057692,-1.,3.74235701734714));
#35564=CARTESIAN_POINT('Ctrl Pts',(-0.497984209510024,-1.,3.73486914372449));
#35565=CARTESIAN_POINT('Ctrl Pts',(-0.497584067153049,-1.,3.72830430904606));
#35566=CARTESIAN_POINT('Ctrl Pts',(-0.497187079575988,-1.,3.72301489774398));
#35567=CARTESIAN_POINT('Ctrl Pts',(-0.496846224822564,-1.,3.71952320822499));
#35568=CARTESIAN_POINT('Ctrl Pts',(-0.496605651525989,-1.,3.71785517607549));
#35569=CARTESIAN_POINT('Ctrl Pts',(-0.496446644158005,-1.,3.71721917030355));
#35570=CARTESIAN_POINT('Ctrl Pts',(-0.496354087924313,-1.,3.71704500630495));
#35571=CARTESIAN_POINT('Ctrl Pts',(-0.496319364827592,-1.,3.71701050416825));
#35572=CARTESIAN_POINT('',(-0.676591647973661,-1.,3.68845817949618));
#35573=CARTESIAN_POINT('Origin',(0.,-1.,0.));
#35574=CARTESIAN_POINT('',(-0.906349047628866,-1.,4.10104028313088));
#35575=CARTESIAN_POINT('Ctrl Pts',(-0.676591647973661,-1.,3.68845817949618));
#35576=CARTESIAN_POINT('Ctrl Pts',(-0.67656928609342,-1.,3.68850172300543));
#35577=CARTESIAN_POINT('Ctrl Pts',(-0.676535079520365,-1.,3.68869596426099));
#35578=CARTESIAN_POINT('Ctrl Pts',(-0.676580391119535,-1.,3.68934997767391));
#35579=CARTESIAN_POINT('Ctrl Pts',(-0.676867042599712,-1.,3.6910107117555));
#35580=CARTESIAN_POINT('Ctrl Pts',(-0.677621861865196,-1.,3.69443683573443));
#35581=CARTESIAN_POINT('Ctrl Pts',(-0.67887882222639,-1.,3.69959004073192));
#35582=CARTESIAN_POINT('Ctrl Pts',(-0.680526909711618,-1.,3.70595722032165));
#35583=CARTESIAN_POINT('Ctrl Pts',(-0.682492345109689,-1.,3.71319182790334));
#35584=CARTESIAN_POINT('Ctrl Pts',(-0.684691698168355,-1.,3.7209063713952));
#35585=CARTESIAN_POINT('Ctrl Pts',(-0.687043475232499,-1.,3.72872973554125));
#35586=CARTESIAN_POINT('Ctrl Pts',(-0.689479637354651,-1.,3.73636374474993));
#35587=CARTESIAN_POINT('Ctrl Pts',(-0.691960080400503,-1.,3.74365508986548));
#35588=CARTESIAN_POINT('Ctrl Pts',(-0.694474562581173,-1.,3.7506028824329));
#35589=CARTESIAN_POINT('Ctrl Pts',(-0.69703124565953,-1.,3.75729775766913));
#35590=CARTESIAN_POINT('Ctrl Pts',(-0.699648552230851,-1.,3.76387780603725));
#35591=CARTESIAN_POINT('Ctrl Pts',(-0.702346356621613,-1.,3.77048141872904));
#35592=CARTESIAN_POINT('Ctrl Pts',(-0.70513584799995,-1.,3.77719254217197));
#35593=CARTESIAN_POINT('Ctrl Pts',(-0.7080158793756,-1.,3.78402183336678));
#35594=CARTESIAN_POINT('Ctrl Pts',(-0.710978231689117,-1.,3.79093694007146));
#35595=CARTESIAN_POINT('Ctrl Pts',(-0.714010733006677,-1.,3.79788100314994));
#35596=CARTESIAN_POINT('Ctrl Pts',(-0.717100993669091,-1.,3.80479445759296));
#35597=CARTESIAN_POINT('Ctrl Pts',(-0.720240466589172,-1.,3.81163885127309));
#35598=CARTESIAN_POINT('Ctrl Pts',(-0.723426346019349,-1.,3.81840802610795));
#35599=CARTESIAN_POINT('Ctrl Pts',(-0.726659281876608,-1.,3.82511495756682));
#35600=CARTESIAN_POINT('Ctrl Pts',(-0.729942010490146,-1.,3.8317839240337));
#35601=CARTESIAN_POINT('Ctrl Pts',(-0.73327770375609,-1.,3.83844103658016));
#35602=CARTESIAN_POINT('Ctrl Pts',(-0.736668240497151,-1.,3.84510432881231));
#35603=CARTESIAN_POINT('Ctrl Pts',(-0.740113146827176,-1.,3.85177770351237));
#35604=CARTESIAN_POINT('Ctrl Pts',(-0.743610542737042,-1.,3.85845645217611));
#35605=CARTESIAN_POINT('Ctrl Pts',(-0.747157716488884,-1.,3.86513062969896));
#35606=CARTESIAN_POINT('Ctrl Pts',(-0.750751822383024,-1.,3.87178914078372));
#35607=CARTESIAN_POINT('Ctrl Pts',(-0.754390577396847,-1.,3.87842382520058));
#35608=CARTESIAN_POINT('Ctrl Pts',(-0.758072800564799,-1.,3.88503262662684));
#35609=CARTESIAN_POINT('Ctrl Pts',(-0.761798028793978,-1.,3.89161738162245));
#35610=CARTESIAN_POINT('Ctrl Pts',(-0.765566256401306,-1.,3.89818233104381));
#35611=CARTESIAN_POINT('Ctrl Pts',(-0.769377629847877,-1.,3.90473237182634));
#35612=CARTESIAN_POINT('Ctrl Pts',(-0.773232154506305,-1.,3.91127138115238));
#35613=CARTESIAN_POINT('Ctrl Pts',(-0.777129415664915,-1.,3.91780062334464));
#35614=CARTESIAN_POINT('Ctrl Pts',(-0.781068718228395,-1.,3.92431956510418));
#35615=CARTESIAN_POINT('Ctrl Pts',(-0.785049202786458,-1.,3.93082655631768));
#35616=CARTESIAN_POINT('Ctrl Pts',(-0.789069971469323,-1.,3.93731956885671));
#35617=CARTESIAN_POINT('Ctrl Pts',(-0.793130205641017,-1.,3.94379688971307));
#35618=CARTESIAN_POINT('Ctrl Pts',(-0.797229296085438,-1.,3.95025788827189));
#35619=CARTESIAN_POINT('Ctrl Pts',(-0.801366797727206,-1.,3.95670276375176));
#35620=CARTESIAN_POINT('Ctrl Pts',(-0.805542372178496,-1.,3.96313222295874));
#35621=CARTESIAN_POINT('Ctrl Pts',(-0.809755732818134,-1.,3.96954717513251));
#35622=CARTESIAN_POINT('Ctrl Pts',(-0.814006592328737,-1.,3.97594844078763));
#35623=CARTESIAN_POINT('Ctrl Pts',(-0.818294599022033,-1.,3.98233640155287));
#35624=CARTESIAN_POINT('Ctrl Pts',(-0.822619346021769,-1.,3.98871104646328));
#35625=CARTESIAN_POINT('Ctrl Pts',(-0.826980400320473,-1.,3.99507212784289));
#35626=CARTESIAN_POINT('Ctrl Pts',(-0.831377325741487,-1.,4.00141928477447));
#35627=CARTESIAN_POINT('Ctrl Pts',(-0.835809705809822,-1.,4.00775216907934));
#35628=CARTESIAN_POINT('Ctrl Pts',(-0.84027717197638,-1.,4.01407059766338));
#35629=CARTESIAN_POINT('Ctrl Pts',(-0.844779403288517,-1.,4.02037456798787));
#35630=CARTESIAN_POINT('Ctrl Pts',(-0.849316107475012,-1.,4.02666418343508));
#35631=CARTESIAN_POINT('Ctrl Pts',(-0.853887006632178,-1.,4.03293960436945));
#35632=CARTESIAN_POINT('Ctrl Pts',(-0.858491822322571,-1.,4.03920099284658));
#35633=CARTESIAN_POINT('Ctrl Pts',(-0.863130256642173,-1.,4.04544845048097));
#35634=CARTESIAN_POINT('Ctrl Pts',(-0.867801988858176,-1.,4.05168199437128));
#35635=CARTESIAN_POINT('Ctrl Pts',(-0.872506694780563,-1.,4.05790159030495));
#35636=CARTESIAN_POINT('Ctrl Pts',(-0.877244060484595,-1.,4.06410717232347));
#35637=CARTESIAN_POINT('Ctrl Pts',(-0.882013797525916,-1.,4.07029866694292));
#35638=CARTESIAN_POINT('Ctrl Pts',(-0.886815658360739,-1.,4.07647601774639));
#35639=CARTESIAN_POINT('Ctrl Pts',(-0.891649447920401,-1.,4.08263920306651));
#35640=CARTESIAN_POINT('Ctrl Pts',(-0.896515019236368,-1.,4.08878822249095));
#35641=CARTESIAN_POINT('Ctrl Pts',(-0.900432820945975,-1.,4.09369611524319));
#35642=CARTESIAN_POINT('Ctrl Pts',(-0.903385402444213,-1.,4.09737067247114));
#35643=CARTESIAN_POINT('Ctrl Pts',(-0.905360112216302,-1.,4.09981755067956));
#35644=CARTESIAN_POINT('Ctrl Pts',(-0.906349047628866,-1.,4.10104028313088));
#35645=CARTESIAN_POINT('',(-1.05427041296137,-1.,4.06552750530042));
#35646=CARTESIAN_POINT('',(-0.906349047628866,-1.,4.10104028313088));
#35647=CARTESIAN_POINT('',(-1.07167739962028,-1.,3.59360648251073));
#35648=CARTESIAN_POINT('Ctrl Pts',(-1.05427041296137,-1.,4.06552750530042));
#35649=CARTESIAN_POINT('Ctrl Pts',(-1.05459645194823,-1.,4.06398907542249));
#35650=CARTESIAN_POINT('Ctrl Pts',(-1.055245071776,-1.,4.06091239149123));
#35651=CARTESIAN_POINT('Ctrl Pts',(-1.05620762707996,-1.,4.05629789307025));
#35652=CARTESIAN_POINT('Ctrl Pts',(-1.05747027727959,-1.,4.05014628384869));
#35653=CARTESIAN_POINT('Ctrl Pts',(-1.05901393666566,-1.,4.04245854427496));
#35654=CARTESIAN_POINT('Ctrl Pts',(-1.06052284711857,-1.,4.03477261141553));
#35655=CARTESIAN_POINT('Ctrl Pts',(-1.06199687787462,-1.,4.02708855235633));
#35656=CARTESIAN_POINT('Ctrl Pts',(-1.06343586496236,-1.,4.01940647495943));
#35657=CARTESIAN_POINT('Ctrl Pts',(-1.06483961343109,-1.,4.01172654187398));
#35658=CARTESIAN_POINT('Ctrl Pts',(-1.06620789963606,-1.,4.00404894952579));
#35659=CARTESIAN_POINT('Ctrl Pts',(-1.06754047381312,-1.,3.99637389920441));
#35660=CARTESIAN_POINT('Ctrl Pts',(-1.06883706263942,-1.,3.98870156857412));
#35661=CARTESIAN_POINT('Ctrl Pts',(-1.07009737257767,-1.,3.98103208801101));
#35662=CARTESIAN_POINT('Ctrl Pts',(-1.07132109206164,-1.,3.9733655022223));
#35663=CARTESIAN_POINT('Ctrl Pts',(-1.07250789943007,-1.,3.96570179322338));
#35664=CARTESIAN_POINT('Ctrl Pts',(-1.07365747426491,-1.,3.95804094429373));
#35665=CARTESIAN_POINT('Ctrl Pts',(-1.07476950921587,-1.,3.95038299600676));
#35666=CARTESIAN_POINT('Ctrl Pts',(-1.07584371946443,-1.,3.94272809633331));
#35667=CARTESIAN_POINT('Ctrl Pts',(-1.07687985975384,-1.,3.93507657572883));
#35668=CARTESIAN_POINT('Ctrl Pts',(-1.07787771707195,-1.,3.9274289334984));
#35669=CARTESIAN_POINT('Ctrl Pts',(-1.07883706663554,-1.,3.91978568924178));
#35670=CARTESIAN_POINT('Ctrl Pts',(-1.07975763507473,-1.,3.91214726022143));
#35671=CARTESIAN_POINT('Ctrl Pts',(-1.08063906483818,-1.,3.90451384092545));
#35672=CARTESIAN_POINT('Ctrl Pts',(-1.08148086931358,-1.,3.8968852509835));
#35673=CARTESIAN_POINT('Ctrl Pts',(-1.08228241999346,-1.,3.88926088975114));
#35674=CARTESIAN_POINT('Ctrl Pts',(-1.08304304871028,-1.,3.88164007721312));
#35675=CARTESIAN_POINT('Ctrl Pts',(-1.08376213307504,-1.,3.8740223372254));
#35676=CARTESIAN_POINT('Ctrl Pts',(-1.08443918607927,-1.,3.86640769434274));
#35677=CARTESIAN_POINT('Ctrl Pts',(-1.08507395120059,-1.,3.85879698702532));
#35678=CARTESIAN_POINT('Ctrl Pts',(-1.08566647671844,-1.,3.85119211322755));
#35679=CARTESIAN_POINT('Ctrl Pts',(-1.08621688337604,-1.,3.8435952876495));
#35680=CARTESIAN_POINT('Ctrl Pts',(-1.08672515456902,-1.,3.83600837071708));
#35681=CARTESIAN_POINT('Ctrl Pts',(-1.08719091307558,-1.,3.82843215316984));
#35682=CARTESIAN_POINT('Ctrl Pts',(-1.08761321539442,-1.,3.82086569676319));
#35683=CARTESIAN_POINT('Ctrl Pts',(-1.08799030610862,-1.,3.81330554446323));
#35684=CARTESIAN_POINT('Ctrl Pts',(-1.0883200925538,-1.,3.8057472665766));
#35685=CARTESIAN_POINT('Ctrl Pts',(-1.08860064435778,-1.,3.79818708705259));
#35686=CARTESIAN_POINT('Ctrl Pts',(-1.08883071512098,-1.,3.79062357974404));
#35687=CARTESIAN_POINT('Ctrl Pts',(-1.08901018614636,-1.,3.78305911299504));
#35688=CARTESIAN_POINT('Ctrl Pts',(-1.0891407279127,-1.,3.77550199409424));
#35689=CARTESIAN_POINT('Ctrl Pts',(-1.08922484204256,-1.,3.76796340094448));
#35690=CARTESIAN_POINT('Ctrl Pts',(-1.08926462734282,-1.,3.76045342580208));
#35691=CARTESIAN_POINT('Ctrl Pts',(-1.08926054632925,-1.,3.75297711748132));
#35692=CARTESIAN_POINT('Ctrl Pts',(-1.08921040494017,-1.,3.74553121371757));
#35693=CARTESIAN_POINT('Ctrl Pts',(-1.08910769013297,-1.,3.73809879348239));
#35694=CARTESIAN_POINT('Ctrl Pts',(-1.08894337390937,-1.,3.73065515162988));
#35695=CARTESIAN_POINT('Ctrl Pts',(-1.08870887220082,-1.,3.72317741369398));
#35696=CARTESIAN_POINT('Ctrl Pts',(-1.0883988733478,-1.,3.71565372339075));
#35697=CARTESIAN_POINT('Ctrl Pts',(-1.08801367312185,-1.,3.70809084139457));
#35698=CARTESIAN_POINT('Ctrl Pts',(-1.08756311291309,-1.,3.70052690909833));
#35699=CARTESIAN_POINT('Ctrl Pts',(-1.08706319540271,-1.,3.69302062410157));
#35700=CARTESIAN_POINT('Ctrl Pts',(-1.0865288888259,-1.,3.68562817420797));
#35701=CARTESIAN_POINT('Ctrl Pts',(-1.0859675575576,-1.,3.67838211685117));
#35702=CARTESIAN_POINT('Ctrl Pts',(-1.0853733414449,-1.,3.67127347729666));
#35703=CARTESIAN_POINT('Ctrl Pts',(-1.08471809922901,-1.,3.66422237895365));
#35704=CARTESIAN_POINT('Ctrl Pts',(-1.08395671077807,-1.,3.65709649161166));
#35705=CARTESIAN_POINT('Ctrl Pts',(-1.08304289898623,-1.,3.64976441208358));
#35706=CARTESIAN_POINT('Ctrl Pts',(-1.08194278850996,-1.,3.64214167843677));
#35707=CARTESIAN_POINT('Ctrl Pts',(-1.08064765719867,-1.,3.63423373196529));
#35708=CARTESIAN_POINT('Ctrl Pts',(-1.07919137290742,-1.,3.62619537902361));
#35709=CARTESIAN_POINT('Ctrl Pts',(-1.07764868137619,-1.,3.61832318504574));
#35710=CARTESIAN_POINT('Ctrl Pts',(-1.07611545402734,-1.,3.61098481349204));
#35711=CARTESIAN_POINT('Ctrl Pts',(-1.07469327168578,-1.,3.60456339887778));
#35712=CARTESIAN_POINT('Ctrl Pts',(-1.07347372545714,-1.,3.59940121154535));
#35713=CARTESIAN_POINT('Ctrl Pts',(-1.07259084660936,-1.,3.59600583194946));
#35714=CARTESIAN_POINT('Ctrl Pts',(-1.07209229745229,-1.,3.59439596999862));
#35715=CARTESIAN_POINT('Ctrl Pts',(-1.07183575450617,-1.,3.59379266874567));
#35716=CARTESIAN_POINT('Ctrl Pts',(-1.07171709254135,-1.,3.5936351279798));
#35717=CARTESIAN_POINT('Ctrl Pts',(-1.07167739962028,-1.,3.59360648251073));
#35718=CARTESIAN_POINT('',(-1.24526366418038,-1.,3.5372048861597));
#35719=CARTESIAN_POINT('Origin',(0.,-1.,0.));
#35720=CARTESIAN_POINT('',(-1.53673442965256,-1.,3.90876544355381));
#35721=CARTESIAN_POINT('Ctrl Pts',(-1.24526366418038,-1.,3.5372048861597));
#35722=CARTESIAN_POINT('Ctrl Pts',(-1.24524838931757,-1.,3.53725139174486));
#35723=CARTESIAN_POINT('Ctrl Pts',(-1.2452449899111,-1.,3.5374485926552));
#35724=CARTESIAN_POINT('Ctrl Pts',(-1.24539205388767,-1.,3.53808746578196));
#35725=CARTESIAN_POINT('Ctrl Pts',(-1.24593497226008,-1.,3.53968291130022));
#35726=CARTESIAN_POINT('Ctrl Pts',(-1.24721646231966,-1.,3.54294877425964));
#35727=CARTESIAN_POINT('Ctrl Pts',(-1.24926408628003,-1.,3.54784190283068));
#35728=CARTESIAN_POINT('Ctrl Pts',(-1.2518879294064,-1.,3.55387287418985));
#35729=CARTESIAN_POINT('Ctrl Pts',(-1.25496090900009,-1.,3.56071094991199));
#35730=CARTESIAN_POINT('Ctrl Pts',(-1.25834000485716,-1.,3.56798645995275));
#35731=CARTESIAN_POINT('Ctrl Pts',(-1.2618866714281,-1.,3.5753456065171));
#35732=CARTESIAN_POINT('Ctrl Pts',(-1.26548706249862,-1.,3.58250452868618));
#35733=CARTESIAN_POINT('Ctrl Pts',(-1.26907758484709,-1.,3.58931807846313));
#35734=CARTESIAN_POINT('Ctrl Pts',(-1.27264798379307,-1.,3.59578698050006));
#35735=CARTESIAN_POINT('Ctrl Pts',(-1.27622049908625,-1.,3.60199947736298));
#35736=CARTESIAN_POINT('Ctrl Pts',(-1.27983492861691,-1.,3.60808907746339));
#35737=CARTESIAN_POINT('Ctrl Pts',(-1.28353255117765,-1.,3.61418935913823));
#35738=CARTESIAN_POINT('Ctrl Pts',(-1.28733755029384,-1.,3.6203814849236));
#35739=CARTESIAN_POINT('Ctrl Pts',(-1.29125046021878,-1.,3.62667616004369));
#35740=CARTESIAN_POINT('Ctrl Pts',(-1.29525810207762,-1.,3.63304271631046));
#35741=CARTESIAN_POINT('Ctrl Pts',(-1.2993395590647,-1.,3.63942689872808));
#35742=CARTESIAN_POINT('Ctrl Pts',(-1.30347327603774,-1.,3.64577181380113));
#35743=CARTESIAN_POINT('Ctrl Pts',(-1.30764479590039,-1.,3.65204081987068));
#35744=CARTESIAN_POINT('Ctrl Pts',(-1.31185038411218,-1.,3.65822827358617));
#35745=CARTESIAN_POINT('Ctrl Pts',(-1.31609271239911,-1.,3.66434688899793));
#35746=CARTESIAN_POINT('Ctrl Pts',(-1.32037828137766,-1.,3.67042021752656));
#35747=CARTESIAN_POINT('Ctrl Pts',(-1.32471430856415,-1.,3.67647355257912));
#35748=CARTESIAN_POINT('Ctrl Pts',(-1.3291054707274,-1.,3.68252441182551));
#35749=CARTESIAN_POINT('Ctrl Pts',(-1.33355191034523,-1.,3.68857672413033));
#35750=CARTESIAN_POINT('Ctrl Pts',(-1.3380510339822,-1.,3.69462613305708));
#35751=CARTESIAN_POINT('Ctrl Pts',(-1.34259860752933,-1.,3.70066324015119));
#35752=CARTESIAN_POINT('Ctrl Pts',(-1.34719008463534,-1.,3.70667753188248));
#35753=CARTESIAN_POINT('Ctrl Pts',(-1.35182193384424,-1.,3.71266130563054));
#35754=CARTESIAN_POINT('Ctrl Pts',(-1.35649266705037,-1.,3.71861271513313));
#35755=CARTESIAN_POINT('Ctrl Pts',(-1.36120211416354,-1.,3.72453364678279));
#35756=CARTESIAN_POINT('Ctrl Pts',(-1.36595093298676,-1.,3.73042829011295));
#35757=CARTESIAN_POINT('Ctrl Pts',(-1.37074003422739,-1.,3.7363014588581));
#35758=CARTESIAN_POINT('Ctrl Pts',(-1.37557002971687,-1.,3.74215698162555));
#35759=CARTESIAN_POINT('Ctrl Pts',(-1.38044070763295,-1.,3.74799617204729));
#35760=CARTESIAN_POINT('Ctrl Pts',(-1.38535129801176,-1.,3.75381861212707));
#35761=CARTESIAN_POINT('Ctrl Pts',(-1.39030069388918,-1.,3.75962280650855));
#35762=CARTESIAN_POINT('Ctrl Pts',(-1.39528769118052,-1.,3.76540689249074));
#35763=CARTESIAN_POINT('Ctrl Pts',(-1.40031121335505,-1.,3.77116930621827));
#35764=CARTESIAN_POINT('Ctrl Pts',(-1.40537056004722,-1.,3.77690952014259));
#35765=CARTESIAN_POINT('Ctrl Pts',(-1.41046532282593,-1.,3.78262780065471));
#35766=CARTESIAN_POINT('Ctrl Pts',(-1.4155952780383,-1.,3.78832489879426));
#35767=CARTESIAN_POINT('Ctrl Pts',(-1.42076028482836,-1.,3.79400175744408));
#35768=CARTESIAN_POINT('Ctrl Pts',(-1.42596018777283,-1.,3.7996592319632));
#35769=CARTESIAN_POINT('Ctrl Pts',(-1.4311946992132,-1.,3.80529775429805));
#35770=CARTESIAN_POINT('Ctrl Pts',(-1.43646341556724,-1.,3.81091737726815));
#35771=CARTESIAN_POINT('Ctrl Pts',(-1.44176587041347,-1.,3.81651792398414));
#35772=CARTESIAN_POINT('Ctrl Pts',(-1.44710157648539,-1.,3.82209910620533));
#35773=CARTESIAN_POINT('Ctrl Pts',(-1.45247006796836,-1.,3.82766064519074));
#35774=CARTESIAN_POINT('Ctrl Pts',(-1.45787095220852,-1.,3.83320241775423));
#35775=CARTESIAN_POINT('Ctrl Pts',(-1.46330391180752,-1.,3.83872447159639));
#35776=CARTESIAN_POINT('Ctrl Pts',(-1.46876867426504,-1.,3.84422695454796));
#35777=CARTESIAN_POINT('Ctrl Pts',(-1.47426499018538,-1.,3.84971006847277));
#35778=CARTESIAN_POINT('Ctrl Pts',(-1.4797926099102,-1.,3.85517401698843));
#35779=CARTESIAN_POINT('Ctrl Pts',(-1.48535125509919,-1.,3.86061894706087));
#35780=CARTESIAN_POINT('Ctrl Pts',(-1.4909406116431,-1.,3.86604492575189));
#35781=CARTESIAN_POINT('Ctrl Pts',(-1.49656035399122,-1.,3.87145196998465));
#35782=CARTESIAN_POINT('Ctrl Pts',(-1.50221016176556,-1.,3.87684006372134));
#35783=CARTESIAN_POINT('Ctrl Pts',(-1.50788973857757,-1.,3.88220917950538));
#35784=CARTESIAN_POINT('Ctrl Pts',(-1.51359883110559,-1.,3.88755930033884));
#35785=CARTESIAN_POINT('Ctrl Pts',(-1.51933724329306,-1.,3.89289043533657));
#35786=CARTESIAN_POINT('Ctrl Pts',(-1.52510482991635,-1.,3.89820260708225));
#35787=CARTESIAN_POINT('Ctrl Pts',(-1.52974216056287,-1.,3.90243719631596));
#35788=CARTESIAN_POINT('Ctrl Pts',(-1.53323321827755,-1.,3.90560462813969));
#35789=CARTESIAN_POINT('Ctrl Pts',(-1.53556639217905,-1.,3.90771246855019));
#35790=CARTESIAN_POINT('Ctrl Pts',(-1.53673442965256,-1.,3.90876544355381));
#35791=CARTESIAN_POINT('',(-1.67727921511438,-1.,3.85054988729471));
#35792=CARTESIAN_POINT('',(-1.53673442965256,-1.,3.90876544355381));
#35793=CARTESIAN_POINT('',(-1.62064718014094,-1.,3.38171594275765));
#35794=CARTESIAN_POINT('Ctrl Pts',(-1.67727921511438,-1.,3.85054988729471));
#35795=CARTESIAN_POINT('Ctrl Pts',(-1.67736057656533,-1.,3.84897939430696));
#35796=CARTESIAN_POINT('Ctrl Pts',(-1.6775199114018,-1.,3.84583912296459));
#35797=CARTESIAN_POINT('Ctrl Pts',(-1.67774874946079,-1.,3.84113085985244));
#35798=CARTESIAN_POINT('Ctrl Pts',(-1.67803353064351,-1.,3.83485746513989));
#35799=CARTESIAN_POINT('Ctrl Pts',(-1.6783555575934,-1.,3.82702289286713));
#35800=CARTESIAN_POINT('Ctrl Pts',(-1.67864354605954,-1.,3.81919554099578));
#35801=CARTESIAN_POINT('Ctrl Pts',(-1.6788973773827,-1.,3.81137549624178));
#35802=CARTESIAN_POINT('Ctrl Pts',(-1.67911690648355,-1.,3.80356289079005));
#35803=CARTESIAN_POINT('Ctrl Pts',(-1.67930196625548,-1.,3.79575791578424));
#35804=CARTESIAN_POINT('Ctrl Pts',(-1.67945236653493,-1.,3.7879608002176));
#35805=CARTESIAN_POINT('Ctrl Pts',(-1.67956789212141,-1.,3.78017178197317));
#35806=CARTESIAN_POINT('Ctrl Pts',(-1.67964830084993,-1.,3.77239107928502));
#35807=CARTESIAN_POINT('Ctrl Pts',(-1.67969332319245,-1.,3.76461886684344));
#35808=CARTESIAN_POINT('Ctrl Pts',(-1.67970265841239,-1.,3.75685523754493));
#35809=CARTESIAN_POINT('Ctrl Pts',(-1.67967598599525,-1.,3.7491002239452));
#35810=CARTESIAN_POINT('Ctrl Pts',(-1.6796129868522,-1.,3.74135385965401));
#35811=CARTESIAN_POINT('Ctrl Pts',(-1.67951336376402,-1.,3.73361623282543));
#35812=CARTESIAN_POINT('Ctrl Pts',(-1.67937685856652,-1.,3.72588753416396));
#35813=CARTESIAN_POINT('Ctrl Pts',(-1.67920328071708,-1.,3.71816812842322));
#35814=CARTESIAN_POINT('Ctrl Pts',(-1.67899249793462,-1.,3.71045854208343));
#35815=CARTESIAN_POINT('Ctrl Pts',(-1.67874436948667,-1.,3.70275932351108));
#35816=CARTESIAN_POINT('Ctrl Pts',(-1.67845869064323,-1.,3.6950709275959));
#35817=CARTESIAN_POINT('Ctrl Pts',(-1.67813513867965,-1.,3.68739360236487));
#35818=CARTESIAN_POINT('Ctrl Pts',(-1.67777320475848,-1.,3.67972724579124));
#35819=CARTESIAN_POINT('Ctrl Pts',(-1.67737217414874,-1.,3.67207136294575));
#35820=CARTESIAN_POINT('Ctrl Pts',(-1.67693128053132,-1.,3.66442538670968));
#35821=CARTESIAN_POINT('Ctrl Pts',(-1.6764498346945,-1.,3.6567889441642));
#35822=CARTESIAN_POINT('Ctrl Pts',(-1.67592735946692,-1.,3.64916213574667));
#35823=CARTESIAN_POINT('Ctrl Pts',(-1.67536373264848,-1.,3.6415458297234));
#35824=CARTESIAN_POINT('Ctrl Pts',(-1.67475929882971,-1.,3.63394189312924));
#35825=CARTESIAN_POINT('Ctrl Pts',(-1.67411452372271,-1.,3.62635249450923));
#35826=CARTESIAN_POINT('Ctrl Pts',(-1.67342968196224,-1.,3.61877947398184));
#35827=CARTESIAN_POINT('Ctrl Pts',(-1.67270452466968,-1.,3.61122367156181));
#35828=CARTESIAN_POINT('Ctrl Pts',(-1.67193797318597,-1.,3.603684308152));
#35829=CARTESIAN_POINT('Ctrl Pts',(-1.67112775290707,-1.,3.59615824388807));
#35830=CARTESIAN_POINT('Ctrl Pts',(-1.67027110397604,-1.,3.58864143097834));
#35831=CARTESIAN_POINT('Ctrl Pts',(-1.66936552908232,-1.,3.58113044183829));
#35832=CARTESIAN_POINT('Ctrl Pts',(-1.668409574073,-1.,3.57362406285887));
#35833=CARTESIAN_POINT('Ctrl Pts',(-1.66740349220305,-1.,3.56612465179422));
#35834=CARTESIAN_POINT('Ctrl Pts',(-1.66635023293114,-1.,3.55864015233602));
#35835=CARTESIAN_POINT('Ctrl Pts',(-1.66525401568994,-1.,3.55118121342861));
#35836=CARTESIAN_POINT('Ctrl Pts',(-1.66411849222326,-1.,3.54375747475014));
#35837=CARTESIAN_POINT('Ctrl Pts',(-1.66294490916111,-1.,3.5363738506022));
#35838=CARTESIAN_POINT('Ctrl Pts',(-1.66173058912371,-1.,3.52902746211093));
#35839=CARTESIAN_POINT('Ctrl Pts',(-1.66046645222279,-1.,3.52170261543815));
#35840=CARTESIAN_POINT('Ctrl Pts',(-1.65913971687342,-1.,3.5143763218894));
#35841=CARTESIAN_POINT('Ctrl Pts',(-1.65773832633632,-1.,3.50702733146542));
#35842=CARTESIAN_POINT('Ctrl Pts',(-1.65625517961588,-1.,3.4996447647794));
#35843=CARTESIAN_POINT('Ctrl Pts',(-1.65469162644468,-1.,3.49223525300176));
#35844=CARTESIAN_POINT('Ctrl Pts',(-1.65306335367739,-1.,3.48483492840894));
#35845=CARTESIAN_POINT('Ctrl Pts',(-1.65139534930322,-1.,3.47749926256476));
#35846=CARTESIAN_POINT('Ctrl Pts',(-1.64971118698256,-1.,3.47028140995992));
#35847=CARTESIAN_POINT('Ctrl Pts',(-1.64802323352738,-1.,3.46321237515));
#35848=CARTESIAN_POINT('Ctrl Pts',(-1.64632429697521,-1.,3.45628421062422));
#35849=CARTESIAN_POINT('Ctrl Pts',(-1.64457408708107,-1.,3.44942242546795));
#35850=CARTESIAN_POINT('Ctrl Pts',(-1.64270733821113,-1.,3.44250337701888));
#35851=CARTESIAN_POINT('Ctrl Pts',(-1.64065778702023,-1.,3.43540451921548));
#35852=CARTESIAN_POINT('Ctrl Pts',(-1.63837876246926,-1.,3.42804772926291));
#35853=CARTESIAN_POINT('Ctrl Pts',(-1.63586250099773,-1.,3.42043974590882));
#35854=CARTESIAN_POINT('Ctrl Pts',(-1.63316667054044,-1.,3.41272817148478));
#35855=CARTESIAN_POINT('Ctrl Pts',(-1.63041148964828,-1.,3.40519422740235));
#35856=CARTESIAN_POINT('Ctrl Pts',(-1.62774916464408,-1.,3.39818605297991));
#35857=CARTESIAN_POINT('Ctrl Pts',(-1.62533996116713,-1.,3.39206617496906));
#35858=CARTESIAN_POINT('Ctrl Pts',(-1.6233278855625,-1.,3.38715832179072));
#35859=CARTESIAN_POINT('Ctrl Pts',(-1.62192472202769,-1.,3.38394285763222));
#35860=CARTESIAN_POINT('Ctrl Pts',(-1.62118047294498,-1.,3.38243080602408));
#35861=CARTESIAN_POINT('Ctrl Pts',(-1.62083271135947,-1.,3.38187506456922));
#35862=CARTESIAN_POINT('Ctrl Pts',(-1.62069086551492,-1.,3.38173802621259));
#35863=CARTESIAN_POINT('Ctrl Pts',(-1.62064718014094,-1.,3.38171594275764));
#35864=CARTESIAN_POINT('',(-1.78327315618183,-1.,3.29885386921599));
#35865=CARTESIAN_POINT('Origin',(0.,-1.,0.));
#35866=CARTESIAN_POINT('',(-2.12928030988903,-1.,3.62024382630768));
#35867=CARTESIAN_POINT('Ctrl Pts',(-1.78327315618183,-1.,3.29885386921599));
#35868=CARTESIAN_POINT('Ctrl Pts',(-1.78326534445426,-1.,3.29890219175522));
#35869=CARTESIAN_POINT('Ctrl Pts',(-1.78329283591903,-1.,3.29909749657945));
#35870=CARTESIAN_POINT('Ctrl Pts',(-1.78353803106983,-1.,3.29970549824337));
#35871=CARTESIAN_POINT('Ctrl Pts',(-1.7843238478823,-1.,3.30119637003466));
#35872=CARTESIAN_POINT('Ctrl Pts',(-1.78610045419769,-1.,3.30422155558973));
#35873=CARTESIAN_POINT('Ctrl Pts',(-1.78888832245965,-1.,3.30873412266954));
#35874=CARTESIAN_POINT('Ctrl Pts',(-1.79242331350137,-1.,3.31428038326763));
#35875=CARTESIAN_POINT('Ctrl Pts',(-1.79652817033444,-1.,3.32055355101168));
#35876=CARTESIAN_POINT('Ctrl Pts',(-1.80100380443535,-1.,3.3272108803981));
#35877=CARTESIAN_POINT('Ctrl Pts',(-1.80565802981138,-1.,3.33392460276874));
#35878=CARTESIAN_POINT('Ctrl Pts',(-1.81033399625311,-1.,3.34043216147532));
#35879=CARTESIAN_POINT('Ctrl Pts',(-1.81494618732772,-1.,3.34660014370527));
#35880=CARTESIAN_POINT('Ctrl Pts',(-1.81948458796748,-1.,3.35243086937451));
#35881=CARTESIAN_POINT('Ctrl Pts',(-1.82398496829247,-1.,3.35800801557326));
#35882=CARTESIAN_POINT('Ctrl Pts',(-1.82850752153182,-1.,3.36345722124127));
#35883=CARTESIAN_POINT('Ctrl Pts',(-1.83311391452338,-1.,3.36890396271864));
#35884=CARTESIAN_POINT('Ctrl Pts',(-1.83784072967111,-1.,3.37442462015914));
#35885=CARTESIAN_POINT('Ctrl Pts',(-1.84269016931679,-1.,3.38002968341222));
#35886=CARTESIAN_POINT('Ctrl Pts',(-1.84764441927778,-1.,3.38569092349639));
#35887=CARTESIAN_POINT('Ctrl Pts',(-1.85267433291778,-1.,3.39135802549415));
#35888=CARTESIAN_POINT('Ctrl Pts',(-1.85774972037055,-1.,3.39697816833056));
#35889=CARTESIAN_POINT('Ctrl Pts',(-1.86285057051228,-1.,3.40251742305445));
#35890=CARTESIAN_POINT('Ctrl Pts',(-1.86797231196635,-1.,3.40797080000513));
#35891=CARTESIAN_POINT('Ctrl Pts',(-1.87311957248106,-1.,3.41335043875182));
#35892=CARTESIAN_POINT('Ctrl Pts',(-1.87830245689338,-1.,3.4186785838376));
#35893=CARTESIAN_POINT('Ctrl Pts',(-1.88353205062063,-1.,3.42397908819741));
#35894=CARTESIAN_POINT('Ctrl Pts',(-1.88881571322018,-1.,3.42926852222174));
#35895=CARTESIAN_POINT('Ctrl Pts',(-1.89415420002553,-1.,3.43455074411591));
#35896=CARTESIAN_POINT('Ctrl Pts',(-1.89954426803392,-1.,3.43982185678105));
#35897=CARTESIAN_POINT('Ctrl Pts',(-1.90498026502308,-1.,3.44507323983374));
#35898=CARTESIAN_POINT('Ctrl Pts',(-1.91045605593638,-1.,3.45029522038885));
#35899=CARTESIAN_POINT('Ctrl Pts',(-1.9159669478406,-1.,3.45548074309943));
#35900=CARTESIAN_POINT('Ctrl Pts',(-1.9215111821321,-1.,3.4606282172248));
#35901=CARTESIAN_POINT('Ctrl Pts',(-1.92708888591159,-1.,3.46573953254084));
#35902=CARTESIAN_POINT('Ctrl Pts',(-1.93270136427083,-1.,3.47081872409783));
#35903=CARTESIAN_POINT('Ctrl Pts',(-1.93835026973888,-1.,3.47587040389916));
#35904=CARTESIAN_POINT('Ctrl Pts',(-1.94403680554062,-1.,3.48089825770411));
#35905=CARTESIAN_POINT('Ctrl Pts',(-1.94976096795902,-1.,3.485903616108));
#35906=CARTESIAN_POINT('Ctrl Pts',(-1.95552193112071,-1.,3.49088618670967));
#35907=CARTESIAN_POINT('Ctrl Pts',(-1.96131836776489,-1.,3.49584466573045));
#35908=CARTESIAN_POINT('Ctrl Pts',(-1.9671487972405,-1.,3.50077740176262));
#35909=CARTESIAN_POINT('Ctrl Pts',(-1.9730119116298,-1.,3.505683018611));
#35910=CARTESIAN_POINT('Ctrl Pts',(-1.97890693666316,-1.,3.51056110478334));
#35911=CARTESIAN_POINT('Ctrl Pts',(-1.98483351061066,-1.,3.51541198728362));
#35912=CARTESIAN_POINT('Ctrl Pts',(-1.99079153006143,-1.,3.52023644289195));
#35913=CARTESIAN_POINT('Ctrl Pts',(-1.99678100339305,-1.,3.52503542491745));
#35914=CARTESIAN_POINT('Ctrl Pts',(-2.00280191090341,-1.,3.52980980250181));
#35915=CARTESIAN_POINT('Ctrl Pts',(-2.00885403604685,-1.,3.53456004727321));
#35916=CARTESIAN_POINT('Ctrl Pts',(-2.0149369884727,-1.,3.53928627453503));
#35917=CARTESIAN_POINT('Ctrl Pts',(-2.0210502798303,-1.,3.54398838254011));
#35918=CARTESIAN_POINT('Ctrl Pts',(-2.02719338376144,-1.,3.54866616282173));
#35919=CARTESIAN_POINT('Ctrl Pts',(-2.03336579658174,-1.,3.55331941294018));
#35920=CARTESIAN_POINT('Ctrl Pts',(-2.03956711120099,-1.,3.55794807265052));
#35921=CARTESIAN_POINT('Ctrl Pts',(-2.04579702159056,-1.,3.5625522387181));
#35922=CARTESIAN_POINT('Ctrl Pts',(-2.0520552817309,-1.,3.56713209978207));
#35923=CARTESIAN_POINT('Ctrl Pts',(-2.05834167687523,-1.,3.57168789423507));
#35924=CARTESIAN_POINT('Ctrl Pts',(-2.06465599229174,-1.,3.576219862243));
#35925=CARTESIAN_POINT('Ctrl Pts',(-2.07099797605747,-1.,3.58072819250442));
#35926=CARTESIAN_POINT('Ctrl Pts',(-2.07736732842117,-1.,3.58521300039299));
#35927=CARTESIAN_POINT('Ctrl Pts',(-2.08376373048756,-1.,3.58967435355088));
#35928=CARTESIAN_POINT('Ctrl Pts',(-2.09018686331416,-1.,3.59411228625588));
#35929=CARTESIAN_POINT('Ctrl Pts',(-2.09663642986631,-1.,3.59852681775485));
#35930=CARTESIAN_POINT('Ctrl Pts',(-2.1031121772821,-1.,3.60291797088734));
#35931=CARTESIAN_POINT('Ctrl Pts',(-2.10961391334462,-1.,3.60728578532601));
#35932=CARTESIAN_POINT('Ctrl Pts',(-2.11614149815106,-1.,3.61163030609447));
#35933=CARTESIAN_POINT('Ctrl Pts',(-2.12138417126355,-1.,3.61508732216891));
#35934=CARTESIAN_POINT('Ctrl Pts',(-2.12532774376758,-1.,3.61766963590482));
#35935=CARTESIAN_POINT('Ctrl Pts',(-2.12796193131368,-1.,3.61938653649098));
#35936=CARTESIAN_POINT('Ctrl Pts',(-2.12928030988903,-1.,3.62024382630768));
#35937=CARTESIAN_POINT('',(-2.25898783642071,-1.,3.54075895182139));
#35938=CARTESIAN_POINT('',(-2.12928030988903,-1.,3.62024382630768));
#35939=CARTESIAN_POINT('',(-2.1297112484669,-1.,3.08655633322212));
#35940=CARTESIAN_POINT('Ctrl Pts',(-2.25898783642071,-1.,3.54075895182139));
#35941=CARTESIAN_POINT('Ctrl Pts',(-2.2588225169468,-1.,3.53919506647335));
#35942=CARTESIAN_POINT('Ctrl Pts',(-2.25848864343951,-1.,3.53606853162228));
#35943=CARTESIAN_POINT('Ctrl Pts',(-2.25797812950104,-1.,3.53138243688262));
#35944=CARTESIAN_POINT('Ctrl Pts',(-2.25727802940898,-1.,3.52514172847711));
#35945=CARTESIAN_POINT('Ctrl Pts',(-2.25637049455044,-1.,3.51735323667612));
#35946=CARTESIAN_POINT('Ctrl Pts',(-2.25543046979799,-1.,3.50957720117341));
#35947=CARTESIAN_POINT('Ctrl Pts',(-2.25445785151868,-1.,3.50181372617971));
#35948=CARTESIAN_POINT('Ctrl Pts',(-2.2534525170976,-1.,3.49406296494791));
#35949=CARTESIAN_POINT('Ctrl Pts',(-2.25241433138695,-1.,3.48632513240961));
#35950=CARTESIAN_POINT('Ctrl Pts',(-2.25134314238687,-1.,3.47860048448691));
#35951=CARTESIAN_POINT('Ctrl Pts',(-2.25023877475942,-1.,3.47088928979888));
#35952=CARTESIAN_POINT('Ctrl Pts',(-2.2491010234604,-1.,3.46319180177573));
#35953=CARTESIAN_POINT('Ctrl Pts',(-2.2479296496077,-1.,3.45550823512049));
#35954=CARTESIAN_POINT('Ctrl Pts',(-2.2467243706995,-1.,3.44783872863151));
#35955=CARTESIAN_POINT('Ctrl Pts',(-2.24548487526022,-1.,3.4401833646032));
#35956=CARTESIAN_POINT('Ctrl Pts',(-2.24421085338727,-1.,3.43254222614803));
#35957=CARTESIAN_POINT('Ctrl Pts',(-2.24290202531101,-1.,3.42491544683008));
#35958=CARTESIAN_POINT('Ctrl Pts',(-2.24155816587844,-1.,3.41730325539172));
#35959=CARTESIAN_POINT('Ctrl Pts',(-2.24017914395289,-1.,3.40970604190328));
#35960=CARTESIAN_POINT('Ctrl Pts',(-2.2387649112415,-1.,3.40212434705647));
#35961=CARTESIAN_POINT('Ctrl Pts',(-2.23731541452791,-1.,3.39455873448189));
#35962=CARTESIAN_POINT('Ctrl Pts',(-2.23583052276308,-1.,3.38700968549563));
#35963=CARTESIAN_POINT('Ctrl Pts',(-2.23430995599561,-1.,3.37947749555632));
#35964=CARTESIAN_POINT('Ctrl Pts',(-2.23275319569221,-1.,3.37196214349304));
#35965=CARTESIAN_POINT('Ctrl Pts',(-2.23115945849739,-1.,3.36446325227848));
#35966=CARTESIAN_POINT('Ctrl Pts',(-2.22952789880982,-1.,3.35698038165483));
#35967=CARTESIAN_POINT('Ctrl Pts',(-2.22785777756576,-1.,3.34951327111096));
#35968=CARTESIAN_POINT('Ctrl Pts',(-2.22614863918047,-1.,3.34206209449375));
#35969=CARTESIAN_POINT('Ctrl Pts',(-2.22440049878511,-1.,3.33462772849598));
#35970=CARTESIAN_POINT('Ctrl Pts',(-2.22261398879635,-1.,3.3272119632604));
#35971=CARTESIAN_POINT('Ctrl Pts',(-2.22078990842776,-1.,3.31981686778022));
#35972=CARTESIAN_POINT('Ctrl Pts',(-2.21892881679086,-1.,3.31244421655666));
#35973=CARTESIAN_POINT('Ctrl Pts',(-2.21703059947836,-1.,3.30509487819569));
#35974=CARTESIAN_POINT('Ctrl Pts',(-2.21509406923368,-1.,3.29776825193159));
#35975=CARTESIAN_POINT('Ctrl Pts',(-2.21311648827391,-1.,3.29046159238343));
#35976=CARTESIAN_POINT('Ctrl Pts',(-2.21109449750641,-1.,3.28317133333131));
#35977=CARTESIAN_POINT('Ctrl Pts',(-2.2090250941743,-1.,3.2758944800554));
#35978=CARTESIAN_POINT('Ctrl Pts',(-2.20690665217743,-1.,3.26863006136782));
#35979=CARTESIAN_POINT('Ctrl Pts',(-2.20473979048678,-1.,3.26138036637705));
#35980=CARTESIAN_POINT('Ctrl Pts',(-2.20252866491545,-1.,3.25415277957775));
#35981=CARTESIAN_POINT('Ctrl Pts',(-2.20027910880981,-1.,3.24695715874338));
#35982=CARTESIAN_POINT('Ctrl Pts',(-2.19799623693253,-1.,3.23980245361308));
#35983=CARTESIAN_POINT('Ctrl Pts',(-2.19568204933168,-1.,3.23269332296933));
#35984=CARTESIAN_POINT('Ctrl Pts',(-2.19333345123538,-1.,3.22562734221646));
#35985=CARTESIAN_POINT('Ctrl Pts',(-2.19093901948667,-1.,3.21859043114095));
#35986=CARTESIAN_POINT('Ctrl Pts',(-2.18848253363901,-1.,3.21156188355769));
#35987=CARTESIAN_POINT('Ctrl Pts',(-2.18594876115934,-1.,3.20452259717976));
#35988=CARTESIAN_POINT('Ctrl Pts',(-2.18332898656602,-1.,3.19746293740411));
#35989=CARTESIAN_POINT('Ctrl Pts',(-2.18062558031778,-1.,3.19038924261573));
#35990=CARTESIAN_POINT('Ctrl Pts',(-2.17785968847142,-1.,3.18333474627807));
#35991=CARTESIAN_POINT('Ctrl Pts',(-2.17506466903694,-1.,3.17635032802523));
#35992=CARTESIAN_POINT('Ctrl Pts',(-2.17227212063817,-1.,3.16948480019497));
#35993=CARTESIAN_POINT('Ctrl Pts',(-2.16949910801219,-1.,3.16276685102972));
#35994=CARTESIAN_POINT('Ctrl Pts',(-2.1667372844769,-1.,3.15618975593656));
#35995=CARTESIAN_POINT('Ctrl Pts',(-2.16393520288072,-1.,3.14968624389054));
#35996=CARTESIAN_POINT('Ctrl Pts',(-2.16100905914435,-1.,3.14314440427022));
#35997=CARTESIAN_POINT('Ctrl Pts',(-2.15787423530676,-1.,3.13645356563038));
#35998=CARTESIAN_POINT('Ctrl Pts',(-2.1544724138292,-1.,3.12954386795646));
#35999=CARTESIAN_POINT('Ctrl Pts',(-2.15079698090585,-1.,3.12242318151938));
#36000=CARTESIAN_POINT('Ctrl Pts',(-2.14692798457532,-1.,3.11522827016855));
#36001=CARTESIAN_POINT('Ctrl Pts',(-2.14302815601973,-1.,3.10821808668859));
#36002=CARTESIAN_POINT('Ctrl Pts',(-2.13930228863751,-1.,3.10171267391049));
#36003=CARTESIAN_POINT('Ctrl Pts',(-2.13596538661048,-1.,3.0960450242104));
#36004=CARTESIAN_POINT('Ctrl Pts',(-2.13321032560893,-1.,3.09151235281963));
#36005=CARTESIAN_POINT('Ctrl Pts',(-2.13132142793017,-1.,3.08855597949761));
#36006=CARTESIAN_POINT('Ctrl Pts',(-2.13034980480424,-1.,3.08717896996099));
#36007=CARTESIAN_POINT('Ctrl Pts',(-2.12991938762374,-1.,3.08668447250322));
#36008=CARTESIAN_POINT('Ctrl Pts',(-2.1297578506149,-1.,3.08657131089497));
#36009=CARTESIAN_POINT('Ctrl Pts',(-2.1297112484669,-1.,3.08655633322212));
#36010=CARTESIAN_POINT('',(-2.27737254473378,-1.,2.97927412174388));
#36011=CARTESIAN_POINT('Origin',(0.,-1.,0.));
#36012=CARTESIAN_POINT('',(-2.66939624221984,-1.,3.24257979115744));
#36013=CARTESIAN_POINT('Ctrl Pts',(-2.27737254473378,-1.,2.97927412174388));
#36014=CARTESIAN_POINT('Ctrl Pts',(-2.27737238849212,-1.,2.97932307137589));
#36015=CARTESIAN_POINT('Ctrl Pts',(-2.27743009389704,-1.,2.97951167106106));
#36016=CARTESIAN_POINT('Ctrl Pts',(-2.27776738270369,-1.,2.98007383024333));
#36017=CARTESIAN_POINT('Ctrl Pts',(-2.27877674853833,-1.,2.98142341809623));
#36018=CARTESIAN_POINT('Ctrl Pts',(-2.28100472516582,-1.,2.98413343613858));
#36019=CARTESIAN_POINT('Ctrl Pts',(-2.28446419116036,-1.,2.98815432734929));
#36020=CARTESIAN_POINT('Ctrl Pts',(-2.28882328690601,-1.,2.9930793098434));
#36021=CARTESIAN_POINT('Ctrl Pts',(-2.29385894577999,-1.,2.99863310340004));
#36022=CARTESIAN_POINT('Ctrl Pts',(-2.29932091315939,-1.,3.00450832658822));
#36023=CARTESIAN_POINT('Ctrl Pts',(-2.30496809486529,-1.,3.01041131063882));
#36024=CARTESIAN_POINT('Ctrl Pts',(-2.31060449886577,-1.,3.01610726819019));
#36025=CARTESIAN_POINT('Ctrl Pts',(-2.31612479121528,-1.,3.02147780668029));
#36026=CARTESIAN_POINT('Ctrl Pts',(-2.32151944306299,-1.,3.02652678416478));
#36027=CARTESIAN_POINT('Ctrl Pts',(-2.32683687412027,-1.,3.03133125185047));
#36028=CARTESIAN_POINT('Ctrl Pts',(-2.33215619079807,-1.,3.03600588555765));
#36029=CARTESIAN_POINT('Ctrl Pts',(-2.33755792953726,-1.,3.04066496998569));
#36030=CARTESIAN_POINT('Ctrl Pts',(-2.3430901708402,-1.,3.04537822217311));
#36031=CARTESIAN_POINT('Ctrl Pts',(-2.34875673090816,-1.,3.05015565829976));
#36032=CARTESIAN_POINT('Ctrl Pts',(-2.35453559889506,-1.,3.05497218368188));
#36033=CARTESIAN_POINT('Ctrl Pts',(-2.36039011602084,-1.,3.05978266240056));
#36034=CARTESIAN_POINT('Ctrl Pts',(-2.36628220107001,-1.,3.06453964643152));
#36035=CARTESIAN_POINT('Ctrl Pts',(-2.37218678163157,-1.,3.06921275497472));
#36036=CARTESIAN_POINT('Ctrl Pts',(-2.37809856205524,-1.,3.07379777492133));
#36037=CARTESIAN_POINT('Ctrl Pts',(-2.38402401216107,-1.,3.07830597244301));
#36038=CARTESIAN_POINT('Ctrl Pts',(-2.38997659219192,-1.,3.08275773747083));
#36039=CARTESIAN_POINT('Ctrl Pts',(-2.39597098250635,-1.,3.08717489512919));
#36040=CARTESIAN_POINT('Ctrl Pts',(-2.40201704423352,-1.,3.09157266051115));
#36041=CARTESIAN_POINT('Ctrl Pts',(-2.40811612696382,-1.,3.09595472616093));
#36042=CARTESIAN_POINT('Ctrl Pts',(-2.41426441798067,-1.,3.10031775027683));
#36043=CARTESIAN_POINT('Ctrl Pts',(-2.42045498612494,-1.,3.10465410280902));
#36044=CARTESIAN_POINT('Ctrl Pts',(-2.42668025870013,-1.,3.10895518969592));
#36045=CARTESIAN_POINT('Ctrl Pts',(-2.4329344968514,-1.,3.11321477659012));
#36046=CARTESIAN_POINT('Ctrl Pts',(-2.43921571477975,-1.,3.11743156744182));
#36047=CARTESIAN_POINT('Ctrl Pts',(-2.44552433364716,-1.,3.12160740887768));
#36048=CARTESIAN_POINT('Ctrl Pts',(-2.45186227369848,-1.,3.12574608210849));
#36049=CARTESIAN_POINT('Ctrl Pts',(-2.45823188859367,-1.,3.12985188384372));
#36050=CARTESIAN_POINT('Ctrl Pts',(-2.4646349433237,-1.,3.13392826623902));
#36051=CARTESIAN_POINT('Ctrl Pts',(-2.47107164236827,-1.,3.13797654408931));
#36052=CARTESIAN_POINT('Ctrl Pts',(-2.47754112428028,-1.,3.14199655778845));
#36053=CARTESIAN_POINT('Ctrl Pts',(-2.48404187418376,-1.,3.1459872272388));
#36054=CARTESIAN_POINT('Ctrl Pts',(-2.49057217131985,-1.,3.14994715298903));
#36055=CARTESIAN_POINT('Ctrl Pts',(-2.49713050858911,-1.,3.15387518039064));
#36056=CARTESIAN_POINT('Ctrl Pts',(-2.50371605688287,-1.,3.15777102413998));
#36057=CARTESIAN_POINT('Ctrl Pts',(-2.51032851007939,-1.,3.16163506380211));
#36058=CARTESIAN_POINT('Ctrl Pts',(-2.51696788755616,-1.,3.16546808277069));
#36059=CARTESIAN_POINT('Ctrl Pts',(-2.523634346718,-1.,3.16927102130751));
#36060=CARTESIAN_POINT('Ctrl Pts',(-2.5303280040691,-1.,3.17304474093574));
#36061=CARTESIAN_POINT('Ctrl Pts',(-2.53704871950871,-1.,3.17678974135225));
#36062=CARTESIAN_POINT('Ctrl Pts',(-2.54379612552948,-1.,3.18050619750515));
#36063=CARTESIAN_POINT('Ctrl Pts',(-2.55056972387638,-1.,3.18419408529482));
#36064=CARTESIAN_POINT('Ctrl Pts',(-2.55736896206016,-1.,3.1878532811617));
#36065=CARTESIAN_POINT('Ctrl Pts',(-2.56419331092909,-1.,3.19148366395201));
#36066=CARTESIAN_POINT('Ctrl Pts',(-2.57104235898053,-1.,3.19508523784548));
#36067=CARTESIAN_POINT('Ctrl Pts',(-2.577915819091,-1.,3.19865814628955));
#36068=CARTESIAN_POINT('Ctrl Pts',(-2.58481347777953,-1.,3.20220261408685));
#36069=CARTESIAN_POINT('Ctrl Pts',(-2.59173516023605,-1.,3.20571891028879));
#36070=CARTESIAN_POINT('Ctrl Pts',(-2.59868069194267,-1.,3.2092073056959));
#36071=CARTESIAN_POINT('Ctrl Pts',(-2.60564985359699,-1.,3.21266802609297));
#36072=CARTESIAN_POINT('Ctrl Pts',(-2.61264236718662,-1.,3.21610123232465));
#36073=CARTESIAN_POINT('Ctrl Pts',(-2.61965792832396,-1.,3.21950704108654));
#36074=CARTESIAN_POINT('Ctrl Pts',(-2.62669622735548,-1.,3.222885536128));
#36075=CARTESIAN_POINT('Ctrl Pts',(-2.63375697391438,-1.,3.22623678292539));
#36076=CARTESIAN_POINT('Ctrl Pts',(-2.64083992182478,-1.,3.2295608435934));
#36077=CARTESIAN_POINT('Ctrl Pts',(-2.64794488744246,-1.,3.23285778738558));
#36078=CARTESIAN_POINT('Ctrl Pts',(-2.6550717396303,-1.,3.23612768065687));
#36079=CARTESIAN_POINT('Ctrl Pts',(-2.6607906631973,-1.,3.23872200036311));
#36080=CARTESIAN_POINT('Ctrl Pts',(-2.66508964664767,-1.,3.24065561087681));
#36081=CARTESIAN_POINT('Ctrl Pts',(-2.66795998539861,-1.,3.24193929584813));
#36082=CARTESIAN_POINT('Ctrl Pts',(-2.66939624221984,-1.,3.24257979115744));
#36083=CARTESIAN_POINT('',(-2.78507268004356,-1.,3.14378277984898));
#36084=CARTESIAN_POINT('',(-2.66939624221984,-1.,3.24257979115744));
#36085=CARTESIAN_POINT('',(-2.58633475774921,-1.,2.71539546306948));
#36086=CARTESIAN_POINT('Ctrl Pts',(-2.78507268004356,-1.,3.14378277984898));
#36087=CARTESIAN_POINT('Ctrl Pts',(-2.7846647503589,-1.,3.14226401018816));
#36088=CARTESIAN_POINT('Ctrl Pts',(-2.78384588958166,-1.,3.13922819749279));
#36089=CARTESIAN_POINT('Ctrl Pts',(-2.78260859419319,-1.,3.13467965833037));
#36090=CARTESIAN_POINT('Ctrl Pts',(-2.78094085161413,-1.,3.12862530318457));
#36091=CARTESIAN_POINT('Ctrl Pts',(-2.77882610146731,-1.,3.12107467037201));
#36092=CARTESIAN_POINT('Ctrl Pts',(-2.77668121002545,-1.,3.11354142303921));
#36093=CARTESIAN_POINT('Ctrl Pts',(-2.77450609123362,-1.,3.10602568032564));
#36094=CARTESIAN_POINT('Ctrl Pts',(-2.77230064796057,-1.,3.0985276127786));
#36095=CARTESIAN_POINT('Ctrl Pts',(-2.7700647803451,-1.,3.09104745382531));
#36096=CARTESIAN_POINT('Ctrl Pts',(-2.76779837829373,-1.,3.08358548001504));
#36097=CARTESIAN_POINT('Ctrl Pts',(-2.76550131064852,-1.,3.07614198408862));
#36098=CARTESIAN_POINT('Ctrl Pts',(-2.76317341453493,-1.,3.0687172484321));
#36099=CARTESIAN_POINT('Ctrl Pts',(-2.76081448759882,-1.,3.06131152247454));
#36100=CARTESIAN_POINT('Ctrl Pts',(-2.75842427252931,-1.,3.05392498749847));
#36101=CARTESIAN_POINT('Ctrl Pts',(-2.75600247455925,-1.,3.04655777351067));
#36102=CARTESIAN_POINT('Ctrl Pts',(-2.75354880060314,-1.,3.03921001107977));
#36103=CARTESIAN_POINT('Ctrl Pts',(-2.75106299522979,-1.,3.03188187589107));
#36104=CARTESIAN_POINT('Ctrl Pts',(-2.7485448718414,-1.,3.02457362909245));
#36105=CARTESIAN_POINT('Ctrl Pts',(-2.74599436193625,-1.,3.01728567646611));
#36106=CARTESIAN_POINT('Ctrl Pts',(-2.74341150239887,-1.,3.01001855960162));
#36107=CARTESIAN_POINT('Ctrl Pts',(-2.74079632883931,-1.,3.00277284351521));
#36108=CARTESIAN_POINT('Ctrl Pts',(-2.73814878711641,-1.,2.99554902409778));
#36109=CARTESIAN_POINT('Ctrl Pts',(-2.73546864694536,-1.,2.9883474369644));
#36110=CARTESIAN_POINT('Ctrl Pts',(-2.73275539286497,-1.,2.98116814232129));
#36111=CARTESIAN_POINT('Ctrl Pts',(-2.73000819218414,-1.,2.97401089032677));
#36112=CARTESIAN_POINT('Ctrl Pts',(-2.72722614084076,-1.,2.96687537842451));
#36113=CARTESIAN_POINT('Ctrl Pts',(-2.72440846811729,-1.,2.95976146492576));
#36114=CARTESIAN_POINT('Ctrl Pts',(-2.72155475123364,-1.,2.95266939280621));
#36115=CARTESIAN_POINT('Ctrl Pts',(-2.71866514227965,-1.,2.94560002559806));
#36116=CARTESIAN_POINT('Ctrl Pts',(-2.71574054592591,-1.,2.93855503247266));
#36117=CARTESIAN_POINT('Ctrl Pts',(-2.71278207520817,-1.,2.93153633192595));
#36118=CARTESIAN_POINT('Ctrl Pts',(-2.70979055994754,-1.,2.92454558914778));
#36119=CARTESIAN_POINT('Ctrl Pts',(-2.70676602302518,-1.,2.91758367994737));
#36120=CARTESIAN_POINT('Ctrl Pts',(-2.70370719782113,-1.,2.91065019668329));
#36121=CARTESIAN_POINT('Ctrl Pts',(-2.70061095078692,-1.,2.90374285605838));
#36122=CARTESIAN_POINT('Ctrl Pts',(-2.69747340630625,-1.,2.89685866123671));
#36123=CARTESIAN_POINT('Ctrl Pts',(-2.69429113011374,-1.,2.88999512410309));
#36124=CARTESIAN_POINT('Ctrl Pts',(-2.69106236420198,-1.,2.88315153980466));
#36125=CARTESIAN_POINT('Ctrl Pts',(-2.68778807801686,-1.,2.8763300724388));
#36126=CARTESIAN_POINT('Ctrl Pts',(-2.68447353139599,-1.,2.86953736547238));
#36127=CARTESIAN_POINT('Ctrl Pts',(-2.68112602796308,-1.,2.86278224277689));
#36128=CARTESIAN_POINT('Ctrl Pts',(-2.67775201955724,-1.,2.85607274378018));
#36129=CARTESIAN_POINT('Ctrl Pts',(-2.67435421039677,-1.,2.84941315703092));
#36130=CARTESIAN_POINT('Ctrl Pts',(-2.67092916452125,-1.,2.84280157191323));
#36131=CARTESIAN_POINT('Ctrl Pts',(-2.66746339678107,-1.,2.83622586853982));
#36132=CARTESIAN_POINT('Ctrl Pts',(-2.6639376472693,-1.,2.82966813308998));
#36133=CARTESIAN_POINT('Ctrl Pts',(-2.66033388273461,-1.,2.82311188135078));
#36134=CARTESIAN_POINT('Ctrl Pts',(-2.65664198781344,-1.,2.81654896073883));
#36135=CARTESIAN_POINT('Ctrl Pts',(-2.65286529532208,-1.,2.80998526078165));
#36136=CARTESIAN_POINT('Ctrl Pts',(-2.64902988983337,-1.,2.80345029781152));
#36137=CARTESIAN_POINT('Ctrl Pts',(-2.6451766779932,-1.,2.79698910670736));
#36138=CARTESIAN_POINT('Ctrl Pts',(-2.64134450532584,-1.,2.79064495573224));
#36139=CARTESIAN_POINT('Ctrl Pts',(-2.637554714303,-1.,2.78444351041571));
#36140=CARTESIAN_POINT('Ctrl Pts',(-2.63379800904599,-1.,2.77837943466449));
#36141=CARTESIAN_POINT('Ctrl Pts',(-2.63001305229625,-1.,2.77239433377921));
#36142=CARTESIAN_POINT('Ctrl Pts',(-2.62609956506355,-1.,2.76639078479021));
#36143=CARTESIAN_POINT('Ctrl Pts',(-2.62195665834605,-1.,2.76027271596686));
#36144=CARTESIAN_POINT('Ctrl Pts',(-2.61751580407667,-1.,2.7539802502603));
#36145=CARTESIAN_POINT('Ctrl Pts',(-2.61277170105813,-1.,2.74752219567252));
#36146=CARTESIAN_POINT('Ctrl Pts',(-2.60782480638448,-1.,2.7410211099909));
#36147=CARTESIAN_POINT('Ctrl Pts',(-2.60287635688728,-1.,2.73470730109615));
#36148=CARTESIAN_POINT('Ctrl Pts',(-2.59817869034746,-1.,2.7288648348152));
#36149=CARTESIAN_POINT('Ctrl Pts',(-2.59399625537278,-1.,2.72378896977134));
#36150=CARTESIAN_POINT('Ctrl Pts',(-2.59056604771971,-1.,2.71974308958086));
#36151=CARTESIAN_POINT('Ctrl Pts',(-2.58823792682672,-1.,2.71711860281815));
#36152=CARTESIAN_POINT('Ctrl Pts',(-2.58706285424358,-1.,2.71591054189786));
#36153=CARTESIAN_POINT('Ctrl Pts',(-2.58656037976753,-1.,2.71548946460575));
#36154=CARTESIAN_POINT('Ctrl Pts',(-2.58638312917168,-1.,2.71540296616024));
#36155=CARTESIAN_POINT('Ctrl Pts',(-2.58633475774921,-1.,2.71539546306948));
#36156=CARTESIAN_POINT('',(-2.71539546306824,-1.,2.58633475775051));
#36157=CARTESIAN_POINT('Origin',(0.,-1.,0.));
#36158=CARTESIAN_POINT('',(-3.14378277984898,-1.,2.78507268004356));
#36159=CARTESIAN_POINT('Ctrl Pts',(-2.71539546306824,-1.,2.58633475775051));
#36160=CARTESIAN_POINT('Ctrl Pts',(-2.71540296615967,-1.,2.58638312917291));
#36161=CARTESIAN_POINT('Ctrl Pts',(-2.71548946460616,-1.,2.58656037976884));
#36162=CARTESIAN_POINT('Ctrl Pts',(-2.71591054189884,-1.,2.58706285424469));
#36163=CARTESIAN_POINT('Ctrl Pts',(-2.7171186028189,-1.,2.58823792682724));
#36164=CARTESIAN_POINT('Ctrl Pts',(-2.7197430895797,-1.,2.59056604771863));
#36165=CARTESIAN_POINT('Ctrl Pts',(-2.72378896977273,-1.,2.59399625537407));
#36166=CARTESIAN_POINT('Ctrl Pts',(-2.72886483481804,-1.,2.5981786903501));
#36167=CARTESIAN_POINT('Ctrl Pts',(-2.73470730109906,-1.,2.60287635689));
#36168=CARTESIAN_POINT('Ctrl Pts',(-2.74102110999284,-1.,2.60782480638629));
#36169=CARTESIAN_POINT('Ctrl Pts',(-2.74752219567307,-1.,2.61277170105864));
#36170=CARTESIAN_POINT('Ctrl Pts',(-2.75398025025967,-1.,2.61751580407608));
#36171=CARTESIAN_POINT('Ctrl Pts',(-2.76027271596564,-1.,2.62195665834491));
#36172=CARTESIAN_POINT('Ctrl Pts',(-2.76639078478898,-1.,2.6260995650624));
#36173=CARTESIAN_POINT('Ctrl Pts',(-2.77239433377839,-1.,2.63001305229548));
#36174=CARTESIAN_POINT('Ctrl Pts',(-2.77837943466423,-1.,2.63379800904575));
#36175=CARTESIAN_POINT('Ctrl Pts',(-2.78444351041594,-1.,2.63755471430322));
#36176=CARTESIAN_POINT('Ctrl Pts',(-2.79064495573275,-1.,2.64134450532632));
#36177=CARTESIAN_POINT('Ctrl Pts',(-2.7969891067079,-1.,2.6451766779937));
#36178=CARTESIAN_POINT('Ctrl Pts',(-2.80345029781191,-1.,2.64902988983373));
#36179=CARTESIAN_POINT('Ctrl Pts',(-2.80998526078179,-1.,2.65286529532221));
#36180=CARTESIAN_POINT('Ctrl Pts',(-2.81654896073874,-1.,2.65664198781335));
#36181=CARTESIAN_POINT('Ctrl Pts',(-2.82311188135053,-1.,2.66033388273437));
#36182=CARTESIAN_POINT('Ctrl Pts',(-2.82966813308969,-1.,2.66393764726902));
#36183=CARTESIAN_POINT('Ctrl Pts',(-2.8362258685396,-1.,2.66746339678085));
#36184=CARTESIAN_POINT('Ctrl Pts',(-2.84280157191314,-1.,2.67092916452117));
#36185=CARTESIAN_POINT('Ctrl Pts',(-2.84941315703096,-1.,2.67435421039682));
#36186=CARTESIAN_POINT('Ctrl Pts',(-2.85607274378031,-1.,2.67775201955736));
#36187=CARTESIAN_POINT('Ctrl Pts',(-2.86278224277705,-1.,2.68112602796323));
#36188=CARTESIAN_POINT('Ctrl Pts',(-2.8695373654725,-1.,2.68447353139611));
#36189=CARTESIAN_POINT('Ctrl Pts',(-2.87633007243885,-1.,2.68778807801691));
#36190=CARTESIAN_POINT('Ctrl Pts',(-2.88315153980464,-1.,2.69106236420197));
#36191=CARTESIAN_POINT('Ctrl Pts',(-2.88999512410304,-1.,2.69429113011369));
#36192=CARTESIAN_POINT('Ctrl Pts',(-2.89685866123668,-1.,2.69747340630621));
#36193=CARTESIAN_POINT('Ctrl Pts',(-2.90374285605839,-1.,2.70061095078692));
#36194=CARTESIAN_POINT('Ctrl Pts',(-2.91065019668331,-1.,2.70370719782114));
#36195=CARTESIAN_POINT('Ctrl Pts',(-2.91758367994738,-1.,2.70676602302518));
#36196=CARTESIAN_POINT('Ctrl Pts',(-2.92454558914774,-1.,2.70979055994751));
#36197=CARTESIAN_POINT('Ctrl Pts',(-2.93153633192583,-1.,2.71278207520807));
#36198=CARTESIAN_POINT('Ctrl Pts',(-2.93855503247248,-1.,2.71574054592575));
#36199=CARTESIAN_POINT('Ctrl Pts',(-2.94560002559789,-1.,2.71866514227952));
#36200=CARTESIAN_POINT('Ctrl Pts',(-2.95266939280617,-1.,2.72155475123361));
#36201=CARTESIAN_POINT('Ctrl Pts',(-2.95976146492595,-1.,2.72440846811745));
#36202=CARTESIAN_POINT('Ctrl Pts',(-2.96687537842492,-1.,2.72722614084112));
#36203=CARTESIAN_POINT('Ctrl Pts',(-2.97401089032729,-1.,2.7300081921846));
#36204=CARTESIAN_POINT('Ctrl Pts',(-2.98116814232175,-1.,2.73275539286537));
#36205=CARTESIAN_POINT('Ctrl Pts',(-2.98834743696455,-1.,2.73546864694548));
#36206=CARTESIAN_POINT('Ctrl Pts',(-2.99554902409741,-1.,2.73814878711609));
#36207=CARTESIAN_POINT('Ctrl Pts',(-3.00277284351431,-1.,2.74079632883852));
#36208=CARTESIAN_POINT('Ctrl Pts',(-3.01001855960041,-1.,2.7434115023978));
#36209=CARTESIAN_POINT('Ctrl Pts',(-3.01728567646502,-1.,2.74599436193528));
#36210=CARTESIAN_POINT('Ctrl Pts',(-3.02457362909199,-1.,2.74854487184099));
#36211=CARTESIAN_POINT('Ctrl Pts',(-3.03188187589168,-1.,2.75106299523032));
#36212=CARTESIAN_POINT('Ctrl Pts',(-3.03921001108158,-1.,2.75354880060473));
#36213=CARTESIAN_POINT('Ctrl Pts',(-3.04655777351333,-1.,2.7560024745616));
#36214=CARTESIAN_POINT('Ctrl Pts',(-3.05392498750112,-1.,2.75842427253164));
#36215=CARTESIAN_POINT('Ctrl Pts',(-3.06131152247599,-1.,2.76081448760011));
#36216=CARTESIAN_POINT('Ctrl Pts',(-3.06871724843121,-1.,2.76317341453415));
#36217=CARTESIAN_POINT('Ctrl Pts',(-3.07614198408488,-1.,2.76550131064522));
#36218=CARTESIAN_POINT('Ctrl Pts',(-3.08358548000904,-1.,2.76779837828843));
#36219=CARTESIAN_POINT('Ctrl Pts',(-3.09104745381882,-1.,2.77006478033937));
#36220=CARTESIAN_POINT('Ctrl Pts',(-3.09852761277432,-1.,2.77230064795679));
#36221=CARTESIAN_POINT('Ctrl Pts',(-3.10602568032641,-1.,2.7745060912343));
#36222=CARTESIAN_POINT('Ctrl Pts',(-3.11354142304692,-1.,2.77668121003225));
#36223=CARTESIAN_POINT('Ctrl Pts',(-3.12107467038623,-1.,2.77882610147986));
#36224=CARTESIAN_POINT('Ctrl Pts',(-3.12862530320194,-1.,2.78094085162947));
#36225=CARTESIAN_POINT('Ctrl Pts',(-3.1346796583452,-1.,2.78260859420629));
#36226=CARTESIAN_POINT('Ctrl Pts',(-3.13922819750185,-1.,2.78384588958965));
#36227=CARTESIAN_POINT('Ctrl Pts',(-3.14226401019149,-1.,2.78466475036183));
#36228=CARTESIAN_POINT('Ctrl Pts',(-3.14378277984898,-1.,2.78507268004356));
#36229=CARTESIAN_POINT('',(-3.24257979115744,-1.,2.66939624221984));
#36230=CARTESIAN_POINT('',(-3.14378277984898,-1.,2.78507268004356));
#36231=CARTESIAN_POINT('',(-2.97927412174279,-1.,2.27737254473521));
#36232=CARTESIAN_POINT('Ctrl Pts',(-3.24257979115744,-1.,2.66939624221984));
#36233=CARTESIAN_POINT('Ctrl Pts',(-3.24193929584471,-1.,2.66795998539579));
#36234=CARTESIAN_POINT('Ctrl Pts',(-3.24065561086749,-1.,2.66508964663997));
#36235=CARTESIAN_POINT('Ctrl Pts',(-3.23872200034785,-1.,2.6607906631847));
#36236=CARTESIAN_POINT('Ctrl Pts',(-3.236127680639,-1.,2.65507173961555));
#36237=CARTESIAN_POINT('Ctrl Pts',(-3.23285778737096,-1.,2.64794488743038));
#36238=CARTESIAN_POINT('Ctrl Pts',(-3.22956084358547,-1.,2.64083992181823));
#36239=CARTESIAN_POINT('Ctrl Pts',(-3.2262367829246,-1.,2.63375697391372));
#36240=CARTESIAN_POINT('Ctrl Pts',(-3.2228855361324,-1.,2.62669622735912));
#36241=CARTESIAN_POINT('Ctrl Pts',(-3.21950704109321,-1.,2.61965792832947));
#36242=CARTESIAN_POINT('Ctrl Pts',(-3.21610123233082,-1.,2.61264236719171));
#36243=CARTESIAN_POINT('Ctrl Pts',(-3.21266802609682,-1.,2.60564985360017));
#36244=CARTESIAN_POINT('Ctrl Pts',(-3.20920730569681,-1.,2.59868069194342));
#36245=CARTESIAN_POINT('Ctrl Pts',(-3.2057189102873,-1.,2.59173516023481));
#36246=CARTESIAN_POINT('Ctrl Pts',(-3.20220261408414,-1.,2.58481347777729));
#36247=CARTESIAN_POINT('Ctrl Pts',(-3.19865814628682,-1.,2.57791581908875));
#36248=CARTESIAN_POINT('Ctrl Pts',(-3.19508523784363,-1.,2.57104235897899));
#36249=CARTESIAN_POINT('Ctrl Pts',(-3.19148366395139,-1.,2.56419331092858));
#36250=CARTESIAN_POINT('Ctrl Pts',(-3.18785328116218,-1.,2.55736896206056));
#36251=CARTESIAN_POINT('Ctrl Pts',(-3.18419408529594,-1.,2.55056972387731));
#36252=CARTESIAN_POINT('Ctrl Pts',(-3.1805061975064,-1.,2.54379612553051));
#36253=CARTESIAN_POINT('Ctrl Pts',(-3.17678974135318,-1.,2.53704871950948));
#36254=CARTESIAN_POINT('Ctrl Pts',(-3.17304474093612,-1.,2.53032800406941));
#36255=CARTESIAN_POINT('Ctrl Pts',(-3.16927102130736,-1.,2.52363434671788));
#36256=CARTESIAN_POINT('Ctrl Pts',(-3.16546808277023,-1.,2.51696788755577));
#36257=CARTESIAN_POINT('Ctrl Pts',(-3.16163506380157,-1.,2.51032851007894));
#36258=CARTESIAN_POINT('Ctrl Pts',(-3.15777102413957,-1.,2.50371605688252));
#36259=CARTESIAN_POINT('Ctrl Pts',(-3.15387518039046,-1.,2.49713050858896));
#36260=CARTESIAN_POINT('Ctrl Pts',(-3.14994715298907,-1.,2.49057217131988));
#36261=CARTESIAN_POINT('Ctrl Pts',(-3.14598722723896,-1.,2.4840418741839));
#36262=CARTESIAN_POINT('Ctrl Pts',(-3.14199655778863,-1.,2.47754112428043));
#36263=CARTESIAN_POINT('Ctrl Pts',(-3.13797654408943,-1.,2.47107164236838));
#36264=CARTESIAN_POINT('Ctrl Pts',(-3.13392826623906,-1.,2.46463494332374));
#36265=CARTESIAN_POINT('Ctrl Pts',(-3.12985188384371,-1.,2.45823188859366));
#36266=CARTESIAN_POINT('Ctrl Pts',(-3.12574608210847,-1.,2.45186227369846));
#36267=CARTESIAN_POINT('Ctrl Pts',(-3.12160740887768,-1.,2.44552433364715));
#36268=CARTESIAN_POINT('Ctrl Pts',(-3.11743156744186,-1.,2.43921571477977));
#36269=CARTESIAN_POINT('Ctrl Pts',(-3.11321477659018,-1.,2.43293449685144));
#36270=CARTESIAN_POINT('Ctrl Pts',(-3.10895518969595,-1.,2.42668025870015));
#36271=CARTESIAN_POINT('Ctrl Pts',(-3.10465410280896,-1.,2.42045498612489));
#36272=CARTESIAN_POINT('Ctrl Pts',(-3.1003177502767,-1.,2.41426441798057));
#36273=CARTESIAN_POINT('Ctrl Pts',(-3.09595472616076,-1.,2.40811612696369));
#36274=CARTESIAN_POINT('Ctrl Pts',(-3.091572660511,-1.,2.40201704423341));
#36275=CARTESIAN_POINT('Ctrl Pts',(-3.08717489512914,-1.,2.39597098250631));
#36276=CARTESIAN_POINT('Ctrl Pts',(-3.08275773747093,-1.,2.38997659219199));
#36277=CARTESIAN_POINT('Ctrl Pts',(-3.07830597244326,-1.,2.38402401216126));
#36278=CARTESIAN_POINT('Ctrl Pts',(-3.07379777492165,-1.,2.37809856205548));
#36279=CARTESIAN_POINT('Ctrl Pts',(-3.069212754975,-1.,2.37218678163178));
#36280=CARTESIAN_POINT('Ctrl Pts',(-3.06453964643162,-1.,2.36628220107009));
#36281=CARTESIAN_POINT('Ctrl Pts',(-3.0597826624004,-1.,2.36039011602072));
#36282=CARTESIAN_POINT('Ctrl Pts',(-3.05497218368146,-1.,2.35453559889474));
#36283=CARTESIAN_POINT('Ctrl Pts',(-3.05015565829918,-1.,2.34875673090771));
#36284=CARTESIAN_POINT('Ctrl Pts',(-3.04537822217256,-1.,2.34309017083977));
#36285=CARTESIAN_POINT('Ctrl Pts',(-3.04066496998544,-1.,2.33755792953706));
#36286=CARTESIAN_POINT('Ctrl Pts',(-3.03600588555793,-1.,2.33215619079829));
#36287=CARTESIAN_POINT('Ctrl Pts',(-3.03133125185136,-1.,2.32683687412097));
#36288=CARTESIAN_POINT('Ctrl Pts',(-3.02652678416611,-1.,2.32151944306402));
#36289=CARTESIAN_POINT('Ctrl Pts',(-3.02147780668161,-1.,2.31612479121631));
#36290=CARTESIAN_POINT('Ctrl Pts',(-3.01610726819086,-1.,2.31060449886629));
#36291=CARTESIAN_POINT('Ctrl Pts',(-3.01041131063823,-1.,2.30496809486482));
#36292=CARTESIAN_POINT('Ctrl Pts',(-3.00450832658613,-1.,2.29932091315775));
#36293=CARTESIAN_POINT('Ctrl Pts',(-2.99863310339691,-1.,2.29385894577754));
#36294=CARTESIAN_POINT('Ctrl Pts',(-2.99307930984034,-1.,2.28882328690362));
#36295=CARTESIAN_POINT('Ctrl Pts',(-2.9881543273478,-1.,2.28446419115919));
#36296=CARTESIAN_POINT('Ctrl Pts',(-2.98413343613983,-1.,2.28100472516679));
#36297=CARTESIAN_POINT('Ctrl Pts',(-2.9814234180956,-1.,2.27877674853766));
#36298=CARTESIAN_POINT('Ctrl Pts',(-2.98007383024207,-1.,2.27776738270289));
#36299=CARTESIAN_POINT('Ctrl Pts',(-2.9795116710597,-1.,2.27743009389684));
#36300=CARTESIAN_POINT('Ctrl Pts',(-2.97932307137477,-1.,2.27737238849287));
#36301=CARTESIAN_POINT('Ctrl Pts',(-2.97927412174279,-1.,2.27737254473521));
#36302=CARTESIAN_POINT('',(-3.08655633322109,-1.,2.12971124846838));
#36303=CARTESIAN_POINT('Origin',(0.,-1.,0.));
#36304=CARTESIAN_POINT('',(-3.54075895182139,-1.,2.25898783642071));
#36305=CARTESIAN_POINT('Ctrl Pts',(-3.08655633322109,-1.,2.12971124846838));
#36306=CARTESIAN_POINT('Ctrl Pts',(-3.0865713108946,-1.,2.1297578506162));
#36307=CARTESIAN_POINT('Ctrl Pts',(-3.08668447250383,-1.,2.12991938762497));
#36308=CARTESIAN_POINT('Ctrl Pts',(-3.08717896996213,-1.,2.13034980480519));
#36309=CARTESIAN_POINT('Ctrl Pts',(-3.08855597949844,-1.,2.13132142793056));
#36310=CARTESIAN_POINT('Ctrl Pts',(-3.09151235281832,-1.,2.13321032560805));
#36311=CARTESIAN_POINT('Ctrl Pts',(-3.09604502421197,-1.,2.13596538661154));
#36312=CARTESIAN_POINT('Ctrl Pts',(-3.1017126739137,-1.,2.13930228863968));
#36313=CARTESIAN_POINT('Ctrl Pts',(-3.10821808669189,-1.,2.14302815602195));
#36314=CARTESIAN_POINT('Ctrl Pts',(-3.11522827017075,-1.,2.1469279845768));
#36315=CARTESIAN_POINT('Ctrl Pts',(-3.12242318152001,-1.,2.15079698090627));
#36316=CARTESIAN_POINT('Ctrl Pts',(-3.12954386795575,-1.,2.15447241382872));
#36317=CARTESIAN_POINT('Ctrl Pts',(-3.136453565629,-1.,2.15787423530583));
#36318=CARTESIAN_POINT('Ctrl Pts',(-3.14314440426882,-1.,2.16100905914341));
#36319=CARTESIAN_POINT('Ctrl Pts',(-3.14968624388961,-1.,2.16393520288009));
#36320=CARTESIAN_POINT('Ctrl Pts',(-3.15618975593627,-1.,2.1667372844767));
#36321=CARTESIAN_POINT('Ctrl Pts',(-3.16276685102999,-1.,2.16949910801237));
#36322=CARTESIAN_POINT('Ctrl Pts',(-3.16948480019555,-1.,2.17227212063857));
#36323=CARTESIAN_POINT('Ctrl Pts',(-3.17635032802584,-1.,2.17506466903736));
#36324=CARTESIAN_POINT('Ctrl Pts',(-3.18333474627851,-1.,2.17785968847172));
#36325=CARTESIAN_POINT('Ctrl Pts',(-3.19038924261589,-1.,2.18062558031789));
#36326=CARTESIAN_POINT('Ctrl Pts',(-3.197462937404,-1.,2.18332898656595));
#36327=CARTESIAN_POINT('Ctrl Pts',(-3.20452259717947,-1.,2.18594876115914));
#36328=CARTESIAN_POINT('Ctrl Pts',(-3.21156188355736,-1.,2.18848253363878));
#36329=CARTESIAN_POINT('Ctrl Pts',(-3.21859043114069,-1.,2.1909390194865));
#36330=CARTESIAN_POINT('Ctrl Pts',(-3.22562734221636,-1.,2.19333345123531));
#36331=CARTESIAN_POINT('Ctrl Pts',(-3.23269332296938,-1.,2.19568204933172));
#36332=CARTESIAN_POINT('Ctrl Pts',(-3.23980245361323,-1.,2.19799623693263));
#36333=CARTESIAN_POINT('Ctrl Pts',(-3.24695715874356,-1.,2.20027910880993));
#36334=CARTESIAN_POINT('Ctrl Pts',(-3.25415277957789,-1.,2.20252866491554));
#36335=CARTESIAN_POINT('Ctrl Pts',(-3.26138036637711,-1.,2.20473979048682));
#36336=CARTESIAN_POINT('Ctrl Pts',(-3.2686300613678,-1.,2.20690665217741));
#36337=CARTESIAN_POINT('Ctrl Pts',(-3.27589448005534,-1.,2.20902509417425));
#36338=CARTESIAN_POINT('Ctrl Pts',(-3.28317133333127,-1.,2.21109449750638));
#36339=CARTESIAN_POINT('Ctrl Pts',(-3.29046159238344,-1.,2.21311648827391));
#36340=CARTESIAN_POINT('Ctrl Pts',(-3.29776825193162,-1.,2.21509406923369));
#36341=CARTESIAN_POINT('Ctrl Pts',(-3.3050948781957,-1.,2.21703059947837));
#36342=CARTESIAN_POINT('Ctrl Pts',(-3.31244421655662,-1.,2.21892881679083));
#36343=CARTESIAN_POINT('Ctrl Pts',(-3.31981686778008,-1.,2.22078990842768));
#36344=CARTESIAN_POINT('Ctrl Pts',(-3.32721196326019,-1.,2.22261398879623));
#36345=CARTESIAN_POINT('Ctrl Pts',(-3.3346277284958,-1.,2.224400498785));
#36346=CARTESIAN_POINT('Ctrl Pts',(-3.34206209449371,-1.,2.22614863918044));
#36347=CARTESIAN_POINT('Ctrl Pts',(-3.34951327111117,-1.,2.22785777756588));
#36348=CARTESIAN_POINT('Ctrl Pts',(-3.35698038165529,-1.,2.22952789881011));
#36349=CARTESIAN_POINT('Ctrl Pts',(-3.36446325227908,-1.,2.23115945849777));
#36350=CARTESIAN_POINT('Ctrl Pts',(-3.37196214349356,-1.,2.23275319569253));
#36351=CARTESIAN_POINT('Ctrl Pts',(-3.37947749555649,-1.,2.23430995599572));
#36352=CARTESIAN_POINT('Ctrl Pts',(-3.38700968549522,-1.,2.23583052276281));
#36353=CARTESIAN_POINT('Ctrl Pts',(-3.39455873448088,-1.,2.23731541452727));
#36354=CARTESIAN_POINT('Ctrl Pts',(-3.40212434705511,-1.,2.23876491124064));
#36355=CARTESIAN_POINT('Ctrl Pts',(-3.40970604190205,-1.,2.24017914395211));
#36356=CARTESIAN_POINT('Ctrl Pts',(-3.41730325539119,-1.,2.24155816587811));
#36357=CARTESIAN_POINT('Ctrl Pts',(-3.42491544683075,-1.,2.24290202531144));
#36358=CARTESIAN_POINT('Ctrl Pts',(-3.43254222615007,-1.,2.24421085338856));
#36359=CARTESIAN_POINT('Ctrl Pts',(-3.44018336460619,-1.,2.24548487526212));
#36360=CARTESIAN_POINT('Ctrl Pts',(-3.44783872863448,-1.,2.24672437070139));
#36361=CARTESIAN_POINT('Ctrl Pts',(-3.45550823512213,-1.,2.24792964960874));
#36362=CARTESIAN_POINT('Ctrl Pts',(-3.46319180177474,-1.,2.24910102345977));
#36363=CARTESIAN_POINT('Ctrl Pts',(-3.47088928979467,-1.,2.25023877475674));
#36364=CARTESIAN_POINT('Ctrl Pts',(-3.47860048448015,-1.,2.25134314238258));
#36365=CARTESIAN_POINT('Ctrl Pts',(-3.48632513240231,-1.,2.25241433138231));
#36366=CARTESIAN_POINT('Ctrl Pts',(-3.49406296494309,-1.,2.25345251709453));
#36367=CARTESIAN_POINT('Ctrl Pts',(-3.50181372618058,-1.,2.25445785151923));
#36368=CARTESIAN_POINT('Ctrl Pts',(-3.50957720118209,-1.,2.25543046980351));
#36369=CARTESIAN_POINT('Ctrl Pts',(-3.51735323669213,-1.,2.25637049456061));
#36370=CARTESIAN_POINT('Ctrl Pts',(-3.52514172849666,-1.,2.25727802942141));
#36371=CARTESIAN_POINT('Ctrl Pts',(-3.53138243689932,-1.,2.25797812951166));
#36372=CARTESIAN_POINT('Ctrl Pts',(-3.53606853163247,-1.,2.25848864344599));
#36373=CARTESIAN_POINT('Ctrl Pts',(-3.5391950664771,-1.,2.25882251694918));
#36374=CARTESIAN_POINT('Ctrl Pts',(-3.54075895182139,-1.,2.25898783642071));
#36375=CARTESIAN_POINT('',(-3.62024382630768,-1.,2.12928030988903));
#36376=CARTESIAN_POINT('',(-3.54075895182139,-1.,2.25898783642071));
#36377=CARTESIAN_POINT('',(-3.29885386921513,-1.,1.78327315618341));
#36378=CARTESIAN_POINT('Ctrl Pts',(-3.62024382630768,-1.,2.12928030988903));
#36379=CARTESIAN_POINT('Ctrl Pts',(-3.61938653648716,-1.,2.12796193131142));
#36380=CARTESIAN_POINT('Ctrl Pts',(-3.61766963589442,-1.,2.12532774376144));
#36381=CARTESIAN_POINT('Ctrl Pts',(-3.61508732215187,-1.,2.12138417125349));
#36382=CARTESIAN_POINT('Ctrl Pts',(-3.61163030607452,-1.,2.11614149813928));
#36383=CARTESIAN_POINT('Ctrl Pts',(-3.60728578530968,-1.,2.10961391333497));
#36384=CARTESIAN_POINT('Ctrl Pts',(-3.60291797087849,-1.,2.10311217727687));
#36385=CARTESIAN_POINT('Ctrl Pts',(-3.59852681775396,-1.,2.09663642986579));
#36386=CARTESIAN_POINT('Ctrl Pts',(-3.5941122862608,-1.,2.09018686331706));
#36387=CARTESIAN_POINT('Ctrl Pts',(-3.58967435355834,-1.,2.08376373049196));
#36388=CARTESIAN_POINT('Ctrl Pts',(-3.58521300039988,-1.,2.07736732842524));
#36389=CARTESIAN_POINT('Ctrl Pts',(-3.58072819250872,-1.,2.07099797606));
#36390=CARTESIAN_POINT('Ctrl Pts',(-3.57621986224402,-1.,2.06465599229234));
#36391=CARTESIAN_POINT('Ctrl Pts',(-3.5716878942334,-1.,2.05834167687425));
#36392=CARTESIAN_POINT('Ctrl Pts',(-3.56713209977904,-1.,2.05205528172911));
#36393=CARTESIAN_POINT('Ctrl Pts',(-3.56255223871505,-1.,2.04579702158876));
#36394=CARTESIAN_POINT('Ctrl Pts',(-3.55794807264844,-1.,2.03956711119976));
#36395=CARTESIAN_POINT('Ctrl Pts',(-3.55331941293949,-1.,2.03336579658133));
#36396=CARTESIAN_POINT('Ctrl Pts',(-3.54866616282227,-1.,2.02719338376175));
#36397=CARTESIAN_POINT('Ctrl Pts',(-3.54398838254136,-1.,2.02105027983104));
#36398=CARTESIAN_POINT('Ctrl Pts',(-3.53928627453642,-1.,2.01493698847351));
#36399=CARTESIAN_POINT('Ctrl Pts',(-3.53456004727424,-1.,2.00885403604746));
#36400=CARTESIAN_POINT('Ctrl Pts',(-3.52980980250224,-1.,2.00280191090366));
#36401=CARTESIAN_POINT('Ctrl Pts',(-3.52503542491728,-1.,1.99678100339295));
#36402=CARTESIAN_POINT('Ctrl Pts',(-3.52023644289142,-1.,1.99079153006112));
#36403=CARTESIAN_POINT('Ctrl Pts',(-3.51541198728301,-1.,1.9848335106103));
#36404=CARTESIAN_POINT('Ctrl Pts',(-3.51056110478287,-1.,1.97890693666288));
#36405=CARTESIAN_POINT('Ctrl Pts',(-3.5056830186108,-1.,1.97301191162968));
#36406=CARTESIAN_POINT('Ctrl Pts',(-3.50077740176267,-1.,1.96714879724052));
#36407=CARTESIAN_POINT('Ctrl Pts',(-3.49584466573064,-1.,1.961318367765));
#36408=CARTESIAN_POINT('Ctrl Pts',(-3.49088618670987,-1.,1.95552193112084));
#36409=CARTESIAN_POINT('Ctrl Pts',(-3.48590361610814,-1.,1.94976096795911));
#36410=CARTESIAN_POINT('Ctrl Pts',(-3.48089825770416,-1.,1.94403680554065));
#36411=CARTESIAN_POINT('Ctrl Pts',(-3.47587040389915,-1.,1.93835026973887));
#36412=CARTESIAN_POINT('Ctrl Pts',(-3.47081872409781,-1.,1.93270136427081));
#36413=CARTESIAN_POINT('Ctrl Pts',(-3.46573953254084,-1.,1.92708888591158));
#36414=CARTESIAN_POINT('Ctrl Pts',(-3.46062821722485,-1.,1.92151118213212));
#36415=CARTESIAN_POINT('Ctrl Pts',(-3.4554807430995,-1.,1.91596694784063));
#36416=CARTESIAN_POINT('Ctrl Pts',(-3.45029522038888,-1.,1.91045605593639));
#36417=CARTESIAN_POINT('Ctrl Pts',(-3.44507323983367,-1.,1.90498026502304));
#36418=CARTESIAN_POINT('Ctrl Pts',(-3.4398218567809,-1.,1.89954426803384));
#36419=CARTESIAN_POINT('Ctrl Pts',(-3.43455074411571,-1.,1.89415420002542));
#36420=CARTESIAN_POINT('Ctrl Pts',(-3.42926852222158,-1.,1.88881571322009));
#36421=CARTESIAN_POINT('Ctrl Pts',(-3.42397908819736,-1.,1.8835320506206));
#36422=CARTESIAN_POINT('Ctrl Pts',(-3.41867858383771,-1.,1.87830245689344));
#36423=CARTESIAN_POINT('Ctrl Pts',(-3.41335043875209,-1.,1.87311957248121));
#36424=CARTESIAN_POINT('Ctrl Pts',(-3.40797080000549,-1.,1.86797231196654));
#36425=CARTESIAN_POINT('Ctrl Pts',(-3.40251742305476,-1.,1.86285057051245));
#36426=CARTESIAN_POINT('Ctrl Pts',(-3.39697816833067,-1.,1.85774972037062));
#36427=CARTESIAN_POINT('Ctrl Pts',(-3.39135802549398,-1.,1.85267433291769));
#36428=CARTESIAN_POINT('Ctrl Pts',(-3.38569092349592,-1.,1.84764441927753));
#36429=CARTESIAN_POINT('Ctrl Pts',(-3.38002968341157,-1.,1.84269016931643));
#36430=CARTESIAN_POINT('Ctrl Pts',(-3.37442462015853,-1.,1.83784072967077));
#36431=CARTESIAN_POINT('Ctrl Pts',(-3.36890396271836,-1.,1.83311391452322));
#36432=CARTESIAN_POINT('Ctrl Pts',(-3.36345722124158,-1.,1.82850752153199));
#36433=CARTESIAN_POINT('Ctrl Pts',(-3.35800801557424,-1.,1.82398496829301));
#36434=CARTESIAN_POINT('Ctrl Pts',(-3.35243086937598,-1.,1.81948458796829));
#36435=CARTESIAN_POINT('Ctrl Pts',(-3.34660014370673,-1.,1.81494618732853));
#36436=CARTESIAN_POINT('Ctrl Pts',(-3.34043216147606,-1.,1.81033399625352));
#36437=CARTESIAN_POINT('Ctrl Pts',(-3.33392460276808,-1.,1.80565802981102));
#36438=CARTESIAN_POINT('Ctrl Pts',(-3.32721088039578,-1.,1.80100380443406));
#36439=CARTESIAN_POINT('Ctrl Pts',(-3.3205535510082,-1.,1.79652817033251));
#36440=CARTESIAN_POINT('Ctrl Pts',(-3.31428038326424,-1.,1.79242331349949));
#36441=CARTESIAN_POINT('Ctrl Pts',(-3.30873412266788,-1.,1.78888832245873));
#36442=CARTESIAN_POINT('Ctrl Pts',(-3.30422155559112,-1.,1.78610045419846));
#36443=CARTESIAN_POINT('Ctrl Pts',(-3.30119637003393,-1.,1.78432384788174));
#36444=CARTESIAN_POINT('Ctrl Pts',(-3.299705498242,-1.,1.78353803106924));
#36445=CARTESIAN_POINT('Ctrl Pts',(-3.29909749657808,-1.,1.78329283591905));
#36446=CARTESIAN_POINT('Ctrl Pts',(-3.29890219175423,-1.,1.78326534445518));
#36447=CARTESIAN_POINT('Ctrl Pts',(-3.29885386921513,-1.,1.78327315618341));
#36448=CARTESIAN_POINT('',(-3.38171594275687,-1.,1.62064718014256));
#36449=CARTESIAN_POINT('Origin',(0.,-1.,0.));
#36450=CARTESIAN_POINT('',(-3.85054988729471,-1.,1.67727921511438));
#36451=CARTESIAN_POINT('Ctrl Pts',(-3.38171594275687,-1.,1.62064718014256));
#36452=CARTESIAN_POINT('Ctrl Pts',(-3.38173802621243,-1.,1.62069086551626));
#36453=CARTESIAN_POINT('Ctrl Pts',(-3.38187506457001,-1.,1.62083271136059));
#36454=CARTESIAN_POINT('Ctrl Pts',(-3.38243080602536,-1.,1.62118047294574));
#36455=CARTESIAN_POINT('Ctrl Pts',(-3.3839428576331,-1.,1.62192472202795));
#36456=CARTESIAN_POINT('Ctrl Pts',(-3.38715832178929,-1.,1.62332788556183));
#36457=CARTESIAN_POINT('Ctrl Pts',(-3.39206617497078,-1.,1.62533996116793));
#36458=CARTESIAN_POINT('Ctrl Pts',(-3.39818605298342,-1.,1.62774916464571));
#36459=CARTESIAN_POINT('Ctrl Pts',(-3.40519422740596,-1.,1.63041148964996));
#36460=CARTESIAN_POINT('Ctrl Pts',(-3.41272817148719,-1.,1.63316667054156));
#36461=CARTESIAN_POINT('Ctrl Pts',(-3.4204397459095,-1.,1.63586250099804));
#36462=CARTESIAN_POINT('Ctrl Pts',(-3.42804772926213,-1.,1.6383787624689));
#36463=CARTESIAN_POINT('Ctrl Pts',(-3.43540451921397,-1.,1.64065778701952));
#36464=CARTESIAN_POINT('Ctrl Pts',(-3.44250337701736,-1.,1.64270733821042));
#36465=CARTESIAN_POINT('Ctrl Pts',(-3.44942242546693,-1.,1.64457408708059));
#36466=CARTESIAN_POINT('Ctrl Pts',(-3.4562842106239,-1.,1.64632429697506));
#36467=CARTESIAN_POINT('Ctrl Pts',(-3.46321237515029,-1.,1.64802323352752));
#36468=CARTESIAN_POINT('Ctrl Pts',(-3.47028140996055,-1.,1.64971118698285));
#36469=CARTESIAN_POINT('Ctrl Pts',(-3.47749926256543,-1.,1.65139534930353));
#36470=CARTESIAN_POINT('Ctrl Pts',(-3.48483492840942,-1.,1.65306335367762));
#36471=CARTESIAN_POINT('Ctrl Pts',(-3.49223525300194,-1.,1.65469162644476));
#36472=CARTESIAN_POINT('Ctrl Pts',(-3.49964476477929,-1.,1.65625517961583));
#36473=CARTESIAN_POINT('Ctrl Pts',(-3.5070273314651,-1.,1.65773832633617));
#36474=CARTESIAN_POINT('Ctrl Pts',(-3.51437632188903,-1.,1.65913971687324));
#36475=CARTESIAN_POINT('Ctrl Pts',(-3.52170261543787,-1.,1.66046645222266));
#36476=CARTESIAN_POINT('Ctrl Pts',(-3.52902746211081,-1.,1.66173058912365));
#36477=CARTESIAN_POINT('Ctrl Pts',(-3.53637385060225,-1.,1.66294490916113));
#36478=CARTESIAN_POINT('Ctrl Pts',(-3.5437574747503,-1.,1.66411849222334));
#36479=CARTESIAN_POINT('Ctrl Pts',(-3.5511812134288,-1.,1.66525401569004));
#36480=CARTESIAN_POINT('Ctrl Pts',(-3.55864015233617,-1.,1.66635023293121));
#36481=CARTESIAN_POINT('Ctrl Pts',(-3.56612465179429,-1.,1.66740349220308));
#36482=CARTESIAN_POINT('Ctrl Pts',(-3.57362406285884,-1.,1.66840957407299));
#36483=CARTESIAN_POINT('Ctrl Pts',(-3.58113044183823,-1.,1.66936552908228));
#36484=CARTESIAN_POINT('Ctrl Pts',(-3.5886414309783,-1.,1.67027110397601));
#36485=CARTESIAN_POINT('Ctrl Pts',(-3.59615824388808,-1.,1.67112775290706));
#36486=CARTESIAN_POINT('Ctrl Pts',(-3.60368430815203,-1.,1.67193797318598));
#36487=CARTESIAN_POINT('Ctrl Pts',(-3.61122367156182,-1.,1.67270452466968));
#36488=CARTESIAN_POINT('Ctrl Pts',(-3.61877947398179,-1.,1.67342968196223));
#36489=CARTESIAN_POINT('Ctrl Pts',(-3.62635249450908,-1.,1.67411452372265));
#36490=CARTESIAN_POINT('Ctrl Pts',(-3.63394189312902,-1.,1.67475929882962));
#36491=CARTESIAN_POINT('Ctrl Pts',(-3.6415458297232,-1.,1.67536373264839));
#36492=CARTESIAN_POINT('Ctrl Pts',(-3.64916213574663,-1.,1.6759273594669));
#36493=CARTESIAN_POINT('Ctrl Pts',(-3.65678894416442,-1.,1.67644983469459));
#36494=CARTESIAN_POINT('Ctrl Pts',(-3.66442538671018,-1.,1.67693128053153));
#36495=CARTESIAN_POINT('Ctrl Pts',(-3.67207136294639,-1.,1.67737217414901));
#36496=CARTESIAN_POINT('Ctrl Pts',(-3.6797272457918,-1.,1.67777320475872));
#36497=CARTESIAN_POINT('Ctrl Pts',(-3.68739360236505,-1.,1.67813513867973));
#36498=CARTESIAN_POINT('Ctrl Pts',(-3.69507092759545,-1.,1.67845869064304));
#36499=CARTESIAN_POINT('Ctrl Pts',(-3.70275932350998,-1.,1.6787443694862));
#36500=CARTESIAN_POINT('Ctrl Pts',(-3.71045854208195,-1.,1.67899249793398));
#36501=CARTESIAN_POINT('Ctrl Pts',(-3.71816812842188,-1.,1.6792032807165));
#36502=CARTESIAN_POINT('Ctrl Pts',(-3.72588753416339,-1.,1.67937685856627));
#36503=CARTESIAN_POINT('Ctrl Pts',(-3.73361623282617,-1.,1.67951336376434));
#36504=CARTESIAN_POINT('Ctrl Pts',(-3.74135385965622,-1.,1.67961298685316));
#36505=CARTESIAN_POINT('Ctrl Pts',(-3.74910022394845,-1.,1.67967598599665));
#36506=CARTESIAN_POINT('Ctrl Pts',(-3.75685523754816,-1.,1.67970265841379));
#36507=CARTESIAN_POINT('Ctrl Pts',(-3.76461886684523,-1.,1.67969332319322));
#36508=CARTESIAN_POINT('Ctrl Pts',(-3.77239107928394,-1.,1.67964830084946));
#36509=CARTESIAN_POINT('Ctrl Pts',(-3.78017178196859,-1.,1.67956789211943));
#36510=CARTESIAN_POINT('Ctrl Pts',(-3.78796080021026,-1.,1.67945236653175));
#36511=CARTESIAN_POINT('Ctrl Pts',(-3.7957579157763,-1.,1.67930196625203));
#36512=CARTESIAN_POINT('Ctrl Pts',(-3.80356289078481,-1.,1.67911690648128));
#36513=CARTESIAN_POINT('Ctrl Pts',(-3.81137549624273,-1.,1.67889737738311));
#36514=CARTESIAN_POINT('Ctrl Pts',(-3.81919554100522,-1.,1.67864354606363));
#36515=CARTESIAN_POINT('Ctrl Pts',(-3.82702289288453,-1.,1.67835555760094));
#36516=CARTESIAN_POINT('Ctrl Pts',(-3.83485746516115,-1.,1.67803353065273));
#36517=CARTESIAN_POINT('Ctrl Pts',(-3.8411308598706,-1.,1.67774874946867));
#36518=CARTESIAN_POINT('Ctrl Pts',(-3.84583912297567,-1.,1.67751991140661));
#36519=CARTESIAN_POINT('Ctrl Pts',(-3.84897939431104,-1.,1.6773605765671));
#36520=CARTESIAN_POINT('Ctrl Pts',(-3.85054988729471,-1.,1.67727921511438));
#36521=CARTESIAN_POINT('',(-3.90876544355381,-1.,1.53673442965255));
#36522=CARTESIAN_POINT('',(-3.85054988729471,-1.,1.67727921511438));
#36523=CARTESIAN_POINT('',(-3.5372048861591,-1.,1.24526366418208));
#36524=CARTESIAN_POINT('Ctrl Pts',(-3.90876544355381,-1.,1.53673442965255));
#36525=CARTESIAN_POINT('Ctrl Pts',(-3.90771246854607,-1.,1.53556639217742));
#36526=CARTESIAN_POINT('Ctrl Pts',(-3.90560462812846,-1.,1.53323321827311));
#36527=CARTESIAN_POINT('Ctrl Pts',(-3.90243719629755,-1.,1.5297421605556));
#36528=CARTESIAN_POINT('Ctrl Pts',(-3.8982026070607,-1.,1.52510482990784));
#36529=CARTESIAN_POINT('Ctrl Pts',(-3.89289043531893,-1.,1.51933724328609));
#36530=CARTESIAN_POINT('Ctrl Pts',(-3.88755930032927,-1.,1.51359883110181));
#36531=CARTESIAN_POINT('Ctrl Pts',(-3.88220917950443,-1.,1.50788973857719));
#36532=CARTESIAN_POINT('Ctrl Pts',(-3.87684006372665,-1.,1.50221016176766));
#36533=CARTESIAN_POINT('Ctrl Pts',(-3.8714519699927,-1.,1.4965603539944));
#36534=CARTESIAN_POINT('Ctrl Pts',(-3.86604492575933,-1.,1.49094061164604));
#36535=CARTESIAN_POINT('Ctrl Pts',(-3.86061894706551,-1.,1.48535125510102));
#36536=CARTESIAN_POINT('Ctrl Pts',(-3.85517401698952,-1.,1.47979260991063));
#36537=CARTESIAN_POINT('Ctrl Pts',(-3.84971006847096,-1.,1.47426499018467));
#36538=CARTESIAN_POINT('Ctrl Pts',(-3.84422695454469,-1.,1.46876867426374));
#36539=CARTESIAN_POINT('Ctrl Pts',(-3.83872447159309,-1.,1.46330391180621));
#36540=CARTESIAN_POINT('Ctrl Pts',(-3.83320241775199,-1.,1.45787095220763));
#36541=CARTESIAN_POINT('Ctrl Pts',(-3.82766064519,-1.,1.45247006796807));
#36542=CARTESIAN_POINT('Ctrl Pts',(-3.82209910620591,-1.,1.44710157648562));
#36543=CARTESIAN_POINT('Ctrl Pts',(-3.8165179239855,-1.,1.441765870414));
#36544=CARTESIAN_POINT('Ctrl Pts',(-3.81091737726965,-1.,1.43646341556783));
#36545=CARTESIAN_POINT('Ctrl Pts',(-3.80529775429916,-1.,1.43119469921364));
#36546=CARTESIAN_POINT('Ctrl Pts',(-3.79965923196365,-1.,1.42596018777301));
#36547=CARTESIAN_POINT('Ctrl Pts',(-3.7940017574439,-1.,1.42076028482828));
#36548=CARTESIAN_POINT('Ctrl Pts',(-3.78832489879369,-1.,1.41559527803808));
#36549=CARTESIAN_POINT('Ctrl Pts',(-3.78262780065406,-1.,1.41046532282567));
#36550=CARTESIAN_POINT('Ctrl Pts',(-3.77690952014209,-1.,1.40537056004702));
#36551=CARTESIAN_POINT('Ctrl Pts',(-3.77116930621804,-1.,1.40031121335495));
#36552=CARTESIAN_POINT('Ctrl Pts',(-3.76540689249078,-1.,1.39528769118054));
#36553=CARTESIAN_POINT('Ctrl Pts',(-3.75962280650875,-1.,1.39030069388926));
#36554=CARTESIAN_POINT('Ctrl Pts',(-3.75381861212728,-1.,1.38535129801185));
#36555=CARTESIAN_POINT('Ctrl Pts',(-3.74799617204744,-1.,1.38044070763302));
#36556=CARTESIAN_POINT('Ctrl Pts',(-3.7421569816256,-1.,1.3755700297169));
#36557=CARTESIAN_POINT('Ctrl Pts',(-3.73630145885809,-1.,1.37074003422739));
#36558=CARTESIAN_POINT('Ctrl Pts',(-3.73042829011293,-1.,1.36595093298674));
#36559=CARTESIAN_POINT('Ctrl Pts',(-3.72453364678279,-1.,1.36120211416353));
#36560=CARTESIAN_POINT('Ctrl Pts',(-3.71861271513318,-1.,1.35649266705038));
#36561=CARTESIAN_POINT('Ctrl Pts',(-3.71266130563061,-1.,1.35182193384426));
#36562=CARTESIAN_POINT('Ctrl Pts',(-3.7066775318825,-1.,1.34719008463535));
#36563=CARTESIAN_POINT('Ctrl Pts',(-3.70066324015112,-1.,1.3425986075293));
#36564=CARTESIAN_POINT('Ctrl Pts',(-3.69462613305692,-1.,1.33805103398214));
#36565=CARTESIAN_POINT('Ctrl Pts',(-3.68857672413013,-1.,1.33355191034515));
#36566=CARTESIAN_POINT('Ctrl Pts',(-3.68252441182534,-1.,1.32910547072734));
#36567=CARTESIAN_POINT('Ctrl Pts',(-3.67647355257906,-1.,1.32471430856413));
#36568=CARTESIAN_POINT('Ctrl Pts',(-3.67042021752668,-1.,1.3203782813777));
#36569=CARTESIAN_POINT('Ctrl Pts',(-3.66434688899822,-1.,1.31609271239922));
#36570=CARTESIAN_POINT('Ctrl Pts',(-3.65822827358655,-1.,1.31185038411231));
#36571=CARTESIAN_POINT('Ctrl Pts',(-3.65204081987101,-1.,1.30764479590051));
#36572=CARTESIAN_POINT('Ctrl Pts',(-3.64577181380125,-1.,1.30347327603778));
#36573=CARTESIAN_POINT('Ctrl Pts',(-3.6394268987279,-1.,1.29933955906463));
#36574=CARTESIAN_POINT('Ctrl Pts',(-3.63304271630995,-1.,1.29525810207744));
#36575=CARTESIAN_POINT('Ctrl Pts',(-3.62667616004299,-1.,1.29125046021853));
#36576=CARTESIAN_POINT('Ctrl Pts',(-3.62038148492295,-1.,1.2873375502936));
#36577=CARTESIAN_POINT('Ctrl Pts',(-3.61418935913793,-1.,1.28353255117754));
#36578=CARTESIAN_POINT('Ctrl Pts',(-3.60808907746372,-1.,1.27983492861703));
#36579=CARTESIAN_POINT('Ctrl Pts',(-3.60199947736404,-1.,1.27622049908664));
#36580=CARTESIAN_POINT('Ctrl Pts',(-3.59578698050164,-1.,1.27264798379365));
#36581=CARTESIAN_POINT('Ctrl Pts',(-3.5893180784647,-1.,1.26907758484766));
#36582=CARTESIAN_POINT('Ctrl Pts',(-3.58250452868699,-1.,1.26548706249891));
#36583=CARTESIAN_POINT('Ctrl Pts',(-3.5753456065164,-1.,1.26188667142784));
#36584=CARTESIAN_POINT('Ctrl Pts',(-3.56798645995025,-1.,1.25834000485626));
#36585=CARTESIAN_POINT('Ctrl Pts',(-3.56071094990825,-1.,1.25496090899873));
#36586=CARTESIAN_POINT('Ctrl Pts',(-3.5538728741862,-1.,1.25188792940508));
#36587=CARTESIAN_POINT('Ctrl Pts',(-3.54784190282889,-1.,1.24926408627938));
#36588=CARTESIAN_POINT('Ctrl Pts',(-3.54294877426113,-1.,1.2472164623202));
#36589=CARTESIAN_POINT('Ctrl Pts',(-3.53968291129942,-1.,1.24593497225964));
#36590=CARTESIAN_POINT('Ctrl Pts',(-3.53808746578052,-1.,1.2453920538873));
#36591=CARTESIAN_POINT('Ctrl Pts',(-3.53744859265385,-1.,1.24524498991133));
#36592=CARTESIAN_POINT('Ctrl Pts',(-3.53725139174402,-1.,1.24524838931864));
#36593=CARTESIAN_POINT('Ctrl Pts',(-3.5372048861591,-1.,1.24526366418208));
#36594=CARTESIAN_POINT('',(-3.59360648251021,-1.,1.071677399622));
#36595=CARTESIAN_POINT('Origin',(0.,-1.,0.));
#36596=CARTESIAN_POINT('',(-4.06552750530042,-1.,1.05427041296137));
#36597=CARTESIAN_POINT('Ctrl Pts',(-3.59360648251021,-1.,1.071677399622));
#36598=CARTESIAN_POINT('Ctrl Pts',(-3.59363512797985,-1.,1.07171709254271));
#36599=CARTESIAN_POINT('Ctrl Pts',(-3.59379266874663,-1.,1.07183575450716));
#36600=CARTESIAN_POINT('Ctrl Pts',(-3.59439597,-1.,1.07209229745284));
#36601=CARTESIAN_POINT('Ctrl Pts',(-3.59600583195037,-1.,1.07259084660947));
#36602=CARTESIAN_POINT('Ctrl Pts',(-3.59940121154383,-1.,1.0734737254567));
#36603=CARTESIAN_POINT('Ctrl Pts',(-3.6045633988796,-1.,1.0746932716863));
#36604=CARTESIAN_POINT('Ctrl Pts',(-3.61098481349577,-1.,1.07611545402841));
#36605=CARTESIAN_POINT('Ctrl Pts',(-3.61832318504957,-1.,1.07764868137729));
#36606=CARTESIAN_POINT('Ctrl Pts',(-3.62619537902616,-1.,1.07919137290815));
#36607=CARTESIAN_POINT('Ctrl Pts',(-3.63423373196602,-1.,1.08064765719887));
#36608=CARTESIAN_POINT('Ctrl Pts',(-3.64214167843595,-1.,1.08194278850972));
#36609=CARTESIAN_POINT('Ctrl Pts',(-3.64976441208197,-1.,1.08304289898577));
#36610=CARTESIAN_POINT('Ctrl Pts',(-3.65709649161004,-1.,1.08395671077761));
#36611=CARTESIAN_POINT('Ctrl Pts',(-3.66422237895256,-1.,1.0847180992287));
#36612=CARTESIAN_POINT('Ctrl Pts',(-3.67127347729632,-1.,1.0853733414448));
#36613=CARTESIAN_POINT('Ctrl Pts',(-3.67838211685148,-1.,1.08596755755768));
#36614=CARTESIAN_POINT('Ctrl Pts',(-3.68562817420864,-1.,1.08652888882609));
#36615=CARTESIAN_POINT('Ctrl Pts',(-3.69302062410229,-1.,1.08706319540291));
#36616=CARTESIAN_POINT('Ctrl Pts',(-3.70052690909884,-1.,1.08756311291324));
#36617=CARTESIAN_POINT('Ctrl Pts',(-3.70809084139476,-1.,1.0880136731219));
#36618=CARTESIAN_POINT('Ctrl Pts',(-3.71565372339063,-1.,1.08839887334776));
#36619=CARTESIAN_POINT('Ctrl Pts',(-3.72317741369364,-1.,1.08870887220072));
#36620=CARTESIAN_POINT('Ctrl Pts',(-3.73065515162949,-1.,1.08894337390925));
#36621=CARTESIAN_POINT('Ctrl Pts',(-3.73809879348209,-1.,1.08910769013288));
#36622=CARTESIAN_POINT('Ctrl Pts',(-3.74553121371745,-1.,1.08921040494013));
#36623=CARTESIAN_POINT('Ctrl Pts',(-3.75297711748138,-1.,1.08926054632927));
#36624=CARTESIAN_POINT('Ctrl Pts',(-3.76045342580226,-1.,1.08926462734287));
#36625=CARTESIAN_POINT('Ctrl Pts',(-3.76796340094469,-1.,1.08922484204263));
#36626=CARTESIAN_POINT('Ctrl Pts',(-3.7755019940944,-1.,1.08914072791275));
#36627=CARTESIAN_POINT('Ctrl Pts',(-3.78305911299511,-1.,1.08901018614638));
#36628=CARTESIAN_POINT('Ctrl Pts',(-3.79062357974401,-1.,1.08883071512097));
#36629=CARTESIAN_POINT('Ctrl Pts',(-3.79818708705252,-1.,1.08860064435776));
#36630=CARTESIAN_POINT('Ctrl Pts',(-3.80574726657656,-1.,1.08832009255378));
#36631=CARTESIAN_POINT('Ctrl Pts',(-3.81330554446324,-1.,1.08799030610861));
#36632=CARTESIAN_POINT('Ctrl Pts',(-3.82086569676321,-1.,1.08761321539442));
#36633=CARTESIAN_POINT('Ctrl Pts',(-3.82843215316985,-1.,1.08719091307558));
#36634=CARTESIAN_POINT('Ctrl Pts',(-3.83600837071702,-1.,1.08672515456901));
#36635=CARTESIAN_POINT('Ctrl Pts',(-3.84359528764934,-1.,1.08621688337601));
#36636=CARTESIAN_POINT('Ctrl Pts',(-3.85119211322732,-1.,1.08566647671838));
#36637=CARTESIAN_POINT('Ctrl Pts',(-3.85879698702511,-1.,1.08507395120054));
#36638=CARTESIAN_POINT('Ctrl Pts',(-3.86640769434269,-1.,1.08443918607926));
#36639=CARTESIAN_POINT('Ctrl Pts',(-3.87402233722563,-1.,1.0837621330751));
#36640=CARTESIAN_POINT('Ctrl Pts',(-3.88164007721365,-1.,1.08304304871042));
#36641=CARTESIAN_POINT('Ctrl Pts',(-3.88926088975182,-1.,1.08228241999363));
#36642=CARTESIAN_POINT('Ctrl Pts',(-3.89688525098408,-1.,1.08148086931373));
#36643=CARTESIAN_POINT('Ctrl Pts',(-3.90451384092564,-1.,1.08063906483822));
#36644=CARTESIAN_POINT('Ctrl Pts',(-3.91214726022096,-1.,1.0797576350746));
#36645=CARTESIAN_POINT('Ctrl Pts',(-3.91978568924062,-1.,1.07883706663524));
#36646=CARTESIAN_POINT('Ctrl Pts',(-3.92742893349684,-1.,1.07787771707155));
#36647=CARTESIAN_POINT('Ctrl Pts',(-3.93507657572743,-1.,1.07687985975348));
#36648=CARTESIAN_POINT('Ctrl Pts',(-3.94272809633271,-1.,1.07584371946428));
#36649=CARTESIAN_POINT('Ctrl Pts',(-3.95038299600754,-1.,1.07476950921607));
#36650=CARTESIAN_POINT('Ctrl Pts',(-3.95804094429606,-1.,1.07365747426551));
#36651=CARTESIAN_POINT('Ctrl Pts',(-3.96570179322681,-1.,1.07250789943095));
#36652=CARTESIAN_POINT('Ctrl Pts',(-3.97336550222571,-1.,1.07132109206252));
#36653=CARTESIAN_POINT('Ctrl Pts',(-3.98103208801289,-1.,1.07009737257815));
#36654=CARTESIAN_POINT('Ctrl Pts',(-3.98870156857298,-1.,1.06883706263912));
#36655=CARTESIAN_POINT('Ctrl Pts',(-3.99637389919958,-1.,1.06754047381188));
#36656=CARTESIAN_POINT('Ctrl Pts',(-4.00404894951804,-1.,1.06620789963406));
#36657=CARTESIAN_POINT('Ctrl Pts',(-4.0117265418656,-1.,1.06483961342894));
#36658=CARTESIAN_POINT('Ctrl Pts',(-4.0194064749539,-1.,1.06343586496094));
#36659=CARTESIAN_POINT('Ctrl Pts',(-4.02708855235732,-1.,1.06199687787488));
#36660=CARTESIAN_POINT('Ctrl Pts',(-4.03477261142549,-1.,1.06052284712114));
#36661=CARTESIAN_POINT('Ctrl Pts',(-4.04245854429333,-1.,1.05901393667039));
#36662=CARTESIAN_POINT('Ctrl Pts',(-4.05014628387112,-1.,1.05747027728537));
#36663=CARTESIAN_POINT('Ctrl Pts',(-4.05629789308941,-1.,1.0562076270849));
#36664=CARTESIAN_POINT('Ctrl Pts',(-4.06091239150293,-1.,1.05524507177901));
#36665=CARTESIAN_POINT('Ctrl Pts',(-4.06398907542679,-1.,1.05459645194934));
#36666=CARTESIAN_POINT('Ctrl Pts',(-4.06552750530042,-1.,1.05427041296137));
#36667=CARTESIAN_POINT('',(-4.10104028313088,-1.,0.906349047628866));
#36668=CARTESIAN_POINT('',(-4.06552750530042,-1.,1.05427041296137));
#36669=CARTESIAN_POINT('',(-3.68845817949586,-1.,0.676591647975428));
#36670=CARTESIAN_POINT('Ctrl Pts',(-4.10104028313088,-1.,0.906349047628866));
#36671=CARTESIAN_POINT('Ctrl Pts',(-4.09981755067523,-1.,0.905360112215337));
#36672=CARTESIAN_POINT('Ctrl Pts',(-4.09737067245935,-1.,0.903385402441587));
#36673=CARTESIAN_POINT('Ctrl Pts',(-4.09369611522387,-1.,0.900432820941674));
#36674=CARTESIAN_POINT('Ctrl Pts',(-4.08878822246833,-1.,0.896515019231333));
#36675=CARTESIAN_POINT('Ctrl Pts',(-4.08263920304799,-1.,0.891649447916277));
#36676=CARTESIAN_POINT('Ctrl Pts',(-4.07647601773635,-1.,0.886815658358501));
#36677=CARTESIAN_POINT('Ctrl Pts',(-4.07029866694192,-1.,0.882013797525692));
#36678=CARTESIAN_POINT('Ctrl Pts',(-4.06410717232905,-1.,0.877244060485837));
#36679=CARTESIAN_POINT('Ctrl Pts',(-4.0579015903134,-1.,0.872506694782446));
#36680=CARTESIAN_POINT('Ctrl Pts',(-4.05168199437909,-1.,0.867801988859917));
#36681=CARTESIAN_POINT('Ctrl Pts',(-4.04544845048584,-1.,0.863130256643259));
#36682=CARTESIAN_POINT('Ctrl Pts',(-4.03920099284773,-1.,0.858491822322827));
#36683=CARTESIAN_POINT('Ctrl Pts',(-4.03293960436756,-1.,0.853887006631755));
#36684=CARTESIAN_POINT('Ctrl Pts',(-4.02666418343164,-1.,0.849316107474245));
#36685=CARTESIAN_POINT('Ctrl Pts',(-4.02037456798441,-1.,0.844779403287745));
#36686=CARTESIAN_POINT('Ctrl Pts',(-4.01407059766103,-1.,0.840277171975855));
#36687=CARTESIAN_POINT('Ctrl Pts',(-4.00775216907856,-1.,0.835809705809646));
#36688=CARTESIAN_POINT('Ctrl Pts',(-4.00141928477507,-1.,0.831377325741622));
#36689=CARTESIAN_POINT('Ctrl Pts',(-3.99507212784431,-1.,0.826980400320789));
#36690=CARTESIAN_POINT('Ctrl Pts',(-3.98871104646485,-1.,0.822619346022119));
#36691=CARTESIAN_POINT('Ctrl Pts',(-3.98233640155404,-1.,0.818294599022293));
#36692=CARTESIAN_POINT('Ctrl Pts',(-3.97594844078811,-1.,0.814006592328843));
#36693=CARTESIAN_POINT('Ctrl Pts',(-3.96954717513232,-1.,0.80975573281809));
#36694=CARTESIAN_POINT('Ctrl Pts',(-3.96313222295815,-1.,0.805542372178361));
#36695=CARTESIAN_POINT('Ctrl Pts',(-3.95670276375108,-1.,0.801366797727049));
#36696=CARTESIAN_POINT('Ctrl Pts',(-3.95025788827136,-1.,0.797229296085315));
#36697=CARTESIAN_POINT('Ctrl Pts',(-3.94379688971283,-1.,0.793130205640961));
#36698=CARTESIAN_POINT('Ctrl Pts',(-3.93731956885676,-1.,0.789069971469333));
#36699=CARTESIAN_POINT('Ctrl Pts',(-3.93082655631789,-1.,0.785049202786507));
#36700=CARTESIAN_POINT('Ctrl Pts',(-3.92431956510441,-1.,0.781068718228451));
#36701=CARTESIAN_POINT('Ctrl Pts',(-3.9178006233448,-1.,0.777129415664956));
#36702=CARTESIAN_POINT('Ctrl Pts',(-3.91127138115243,-1.,0.773232154506321));
#36703=CARTESIAN_POINT('Ctrl Pts',(-3.90473237182633,-1.,0.769377629847874));
#36704=CARTESIAN_POINT('Ctrl Pts',(-3.89818233104378,-1.,0.765566256401295));
#36705=CARTESIAN_POINT('Ctrl Pts',(-3.89161738162245,-1.,0.761798028793969));
#36706=CARTESIAN_POINT('Ctrl Pts',(-3.88503262662689,-1.,0.758072800564801));
#36707=CARTESIAN_POINT('Ctrl Pts',(-3.87842382520065,-1.,0.754390577396856));
#36708=CARTESIAN_POINT('Ctrl Pts',(-3.87178914078374,-1.,0.750751822383027));
#36709=CARTESIAN_POINT('Ctrl Pts',(-3.86513062969889,-1.,0.747157716488871));
#36710=CARTESIAN_POINT('Ctrl Pts',(-3.85845645217594,-1.,0.743610542737012));
#36711=CARTESIAN_POINT('Ctrl Pts',(-3.85177770351216,-1.,0.740113146827137));
#36712=CARTESIAN_POINT('Ctrl Pts',(-3.84510432881213,-1.,0.736668240497117));
#36713=CARTESIAN_POINT('Ctrl Pts',(-3.83844103658009,-1.,0.733277703756078));
#36714=CARTESIAN_POINT('Ctrl Pts',(-3.83178392403383,-1.,0.729942010490167));
#36715=CARTESIAN_POINT('Ctrl Pts',(-3.82511495756713,-1.,0.726659281876664));
#36716=CARTESIAN_POINT('Ctrl Pts',(-3.81840802610835,-1.,0.723426346019422));
#36717=CARTESIAN_POINT('Ctrl Pts',(-3.81163885127344,-1.,0.720240466589236));
#36718=CARTESIAN_POINT('Ctrl Pts',(-3.80479445759309,-1.,0.717100993669114));
#36719=CARTESIAN_POINT('Ctrl Pts',(-3.79788100314975,-1.,0.71401073300664));
#36720=CARTESIAN_POINT('Ctrl Pts',(-3.79093694007094,-1.,0.710978231689017));
#36721=CARTESIAN_POINT('Ctrl Pts',(-3.78402183336605,-1.,0.708015879375459));
#36722=CARTESIAN_POINT('Ctrl Pts',(-3.77719254217129,-1.,0.705135847999816));
#36723=CARTESIAN_POINT('Ctrl Pts',(-3.77048141872872,-1.,0.702346356621551));
#36724=CARTESIAN_POINT('Ctrl Pts',(-3.76387780603759,-1.,0.699648552230917));
#36725=CARTESIAN_POINT('Ctrl Pts',(-3.75729775767023,-1.,0.697031245659743));
#36726=CARTESIAN_POINT('Ctrl Pts',(-3.75060288243455,-1.,0.694474562581492));
#36727=CARTESIAN_POINT('Ctrl Pts',(-3.74365508986712,-1.,0.69196008040082));
#36728=CARTESIAN_POINT('Ctrl Pts',(-3.73636374475077,-1.,0.689479637354813));
#36729=CARTESIAN_POINT('Ctrl Pts',(-3.72872973554051,-1.,0.687043475232354));
#36730=CARTESIAN_POINT('Ctrl Pts',(-3.7209063713926,-1.,0.684691698167848));
#36731=CARTESIAN_POINT('Ctrl Pts',(-3.71319182789943,-1.,0.68249234510893));
#36732=CARTESIAN_POINT('Ctrl Pts',(-3.70595722031785,-1.,0.680526909710877));
#36733=CARTESIAN_POINT('Ctrl Pts',(-3.69959004073005,-1.,0.678878822226026));
#36734=CARTESIAN_POINT('Ctrl Pts',(-3.69443683573598,-1.,0.677621861865498));
#36735=CARTESIAN_POINT('Ctrl Pts',(-3.69101071175464,-1.,0.676867042599401));
#36736=CARTESIAN_POINT('Ctrl Pts',(-3.68934997767243,-1.,0.676580391119396));
#36737=CARTESIAN_POINT('Ctrl Pts',(-3.68869596425969,-1.,0.676535079520806));
#36738=CARTESIAN_POINT('Ctrl Pts',(-3.68850172300477,-1.,0.676569286094606));
#36739=CARTESIAN_POINT('Ctrl Pts',(-3.68845817949586,-1.,0.676591647975428));
#36740=CARTESIAN_POINT('',(-3.71701050416802,-1.,0.496319364829374));
#36741=CARTESIAN_POINT('Origin',(0.,-1.,0.));
#36742=CARTESIAN_POINT('',(-4.18039834341342,-1.,0.405301974318349));
#36743=CARTESIAN_POINT('Ctrl Pts',(-3.71701050416802,-1.,0.496319364829374));
#36744=CARTESIAN_POINT('Ctrl Pts',(-3.71704500630521,-1.,0.496354087925645));
#36745=CARTESIAN_POINT('Ctrl Pts',(-3.71721917030465,-1.,0.496446644158827));
#36746=CARTESIAN_POINT('Ctrl Pts',(-3.71785517607694,-1.,0.496605651526313));
#36747=CARTESIAN_POINT('Ctrl Pts',(-3.7195232082259,-1.,0.496846224822534));
#36748=CARTESIAN_POINT('Ctrl Pts',(-3.72301489774241,-1.,0.497187079575794));
#36749=CARTESIAN_POINT('Ctrl Pts',(-3.72830430904794,-1.,0.497584067153279));
#36750=CARTESIAN_POINT('Ctrl Pts',(-3.73486914372834,-1.,0.497984209510495));
#36751=CARTESIAN_POINT('Ctrl Pts',(-3.74235701735109,-1.,0.498350586058176));
#36752=CARTESIAN_POINT('Ctrl Pts',(-3.75037362168103,-1.,0.498642802042929));
#36753=CARTESIAN_POINT('Ctrl Pts',(-3.75854082221127,-1.,0.498823681615513));
#36754=CARTESIAN_POINT('Ctrl Pts',(-3.76655401191144,-1.,0.498865792335185));
#36755=CARTESIAN_POINT('Ctrl Pts',(-3.77425499225089,-1.,0.498759900365687));
#36756=CARTESIAN_POINT('Ctrl Pts',(-3.78163975337189,-1.,0.498515471679378));
#36757=CARTESIAN_POINT('Ctrl Pts',(-3.78879701661152,-1.,0.498152751800819));
#36758=CARTESIAN_POINT('Ctrl Pts',(-3.79586380669959,-1.,0.49769689210058));
#36759=CARTESIAN_POINT('Ctrl Pts',(-3.80297788298545,-1.,0.49717175620109));
#36760=CARTESIAN_POINT('Ctrl Pts',(-3.81022254090909,-1.,0.496592643443789));
#36761=CARTESIAN_POINT('Ctrl Pts',(-3.81760756144099,-1.,0.495963937875572));
#36762=CARTESIAN_POINT('Ctrl Pts',(-3.82509963594156,-1.,0.495283458893903));
#36763=CARTESIAN_POINT('Ctrl Pts',(-3.8326409268245,-1.,0.494545212256425));
#36764=CARTESIAN_POINT('Ctrl Pts',(-3.84017095578438,-1.,0.493742574629117));
#36765=CARTESIAN_POINT('Ctrl Pts',(-3.84765051147965,-1.,0.492871792414095));
#36766=CARTESIAN_POINT('Ctrl Pts',(-3.85507287020223,-1.,0.49193363108376));
#36767=CARTESIAN_POINT('Ctrl Pts',(-3.86245057319215,-1.,0.490931482170849));
#36768=CARTESIAN_POINT('Ctrl Pts',(-3.86980755613694,-1.,0.489870245704899));
#36769=CARTESIAN_POINT('Ctrl Pts',(-3.87716963231115,-1.,0.488754973798281));
#36770=CARTESIAN_POINT('Ctrl Pts',(-3.88455453328156,-1.,0.487589452275179));
#36771=CARTESIAN_POINT('Ctrl Pts',(-3.89196582437574,-1.,0.486375337854133));
#36772=CARTESIAN_POINT('Ctrl Pts',(-3.89939844658529,-1.,0.485112963522246));
#36773=CARTESIAN_POINT('Ctrl Pts',(-3.90684210358063,-1.,0.48380183508916));
#36774=CARTESIAN_POINT('Ctrl Pts',(-3.91428536373749,-1.,0.482441230340708));
#36775=CARTESIAN_POINT('Ctrl Pts',(-3.92171976072334,-1.,0.481030798910735));
#36776=CARTESIAN_POINT('Ctrl Pts',(-3.92914297392067,-1.,0.479571028525566));
#36777=CARTESIAN_POINT('Ctrl Pts',(-3.93655660689819,-1.,0.478062927140957));
#36778=CARTESIAN_POINT('Ctrl Pts',(-3.94396469119385,-1.,0.476507810658534));
#36779=CARTESIAN_POINT('Ctrl Pts',(-3.95137192932898,-1.,0.47490705302179));
#36780=CARTESIAN_POINT('Ctrl Pts',(-3.95878201038332,-1.,0.473261847236296));
#36781=CARTESIAN_POINT('Ctrl Pts',(-3.96619600864626,-1.,0.471572978413493));
#36782=CARTESIAN_POINT('Ctrl Pts',(-3.97361320212413,-1.,0.469840942829878));
#36783=CARTESIAN_POINT('Ctrl Pts',(-3.98103175589349,-1.,0.468066047920139));
#36784=CARTESIAN_POINT('Ctrl Pts',(-3.98844946363258,-1.,0.466248520883034));
#36785=CARTESIAN_POINT('Ctrl Pts',(-3.99586444320135,-1.,0.464388610938995));
#36786=CARTESIAN_POINT('Ctrl Pts',(-4.00327590659129,-1.,0.462486702616252));
#36787=CARTESIAN_POINT('Ctrl Pts',(-4.01068390573469,-1.,0.460543280768577));
#36788=CARTESIAN_POINT('Ctrl Pts',(-4.01808900827647,-1.,0.458558885637001));
#36789=CARTESIAN_POINT('Ctrl Pts',(-4.02549199038414,-1.,0.456534070784968));
#36790=CARTESIAN_POINT('Ctrl Pts',(-4.03289354362745,-1.,0.454469363020495));
#36791=CARTESIAN_POINT('Ctrl Pts',(-4.0402939222793,-1.,0.452365214748779));
#36792=CARTESIAN_POINT('Ctrl Pts',(-4.0476929901797,-1.,0.450222009543774));
#36793=CARTESIAN_POINT('Ctrl Pts',(-4.05509037796815,-1.,0.448040082683976));
#36794=CARTESIAN_POINT('Ctrl Pts',(-4.06248560760596,-1.,0.445819737468478));
#36795=CARTESIAN_POINT('Ctrl Pts',(-4.0698782192577,-1.,0.443561262395408));
#36796=CARTESIAN_POINT('Ctrl Pts',(-4.07726792490256,-1.,0.441264951396587));
#36797=CARTESIAN_POINT('Ctrl Pts',(-4.08465462294625,-1.,0.438931108931613));
#36798=CARTESIAN_POINT('Ctrl Pts',(-4.09203832139439,-1.,0.436560044913814));
#36799=CARTESIAN_POINT('Ctrl Pts',(-4.09941908688567,-1.,0.434152073200642));
#36800=CARTESIAN_POINT('Ctrl Pts',(-4.10679698750219,-1.,0.431707508679772));
#36801=CARTESIAN_POINT('Ctrl Pts',(-4.1141720278277,-1.,0.429226666075372));
#36802=CARTESIAN_POINT('Ctrl Pts',(-4.1215441250121,-1.,0.426709855706243));
#36803=CARTESIAN_POINT('Ctrl Pts',(-4.1289131463371,-1.,0.424157375323155));
#36804=CARTESIAN_POINT('Ctrl Pts',(-4.13627893206433,-1.,0.421569503103971));
#36805=CARTESIAN_POINT('Ctrl Pts',(-4.14364132317223,-1.,0.418946490667799));
#36806=CARTESIAN_POINT('Ctrl Pts',(-4.15100018950989,-1.,0.416288556008986));
#36807=CARTESIAN_POINT('Ctrl Pts',(-4.1583554501909,-1.,0.413595877953269));
#36808=CARTESIAN_POINT('Ctrl Pts',(-4.16570705940731,-1.,0.410868596148613));
#36809=CARTESIAN_POINT('Ctrl Pts',(-4.17158541009947,-1.,0.408659167570153));
#36810=CARTESIAN_POINT('Ctrl Pts',(-4.17599251955585,-1.,0.406986596326602));
#36811=CARTESIAN_POINT('Ctrl Pts',(-4.17892985789908,-1.,0.40586466267963));
#36812=CARTESIAN_POINT('Ctrl Pts',(-4.18039834341342,-1.,0.405301974318349));
#36813=CARTESIAN_POINT('',(-4.1923339003649,-1.,0.253646344052521));
#36814=CARTESIAN_POINT('',(-4.18039834341342,-1.,0.405301974318349));
#36815=CARTESIAN_POINT('',(-3.74888939116255,-1.,0.0912596999166822));
#36816=CARTESIAN_POINT('Ctrl Pts',(-4.1923339003649,-1.,0.253646344052521));
#36817=CARTESIAN_POINT('Ctrl Pts',(-4.19097151819241,-1.,0.252860861572565));
#36818=CARTESIAN_POINT('Ctrl Pts',(-4.18824585244066,-1.,0.251293239837692));
#36819=CARTESIAN_POINT('Ctrl Pts',(-4.18415464959491,-1.,0.248951836910963));
#36820=CARTESIAN_POINT('Ctrl Pts',(-4.17869430192868,-1.,0.245850033418583));
#36821=CARTESIAN_POINT('Ctrl Pts',(-4.17185984409533,-1.,0.242006283923911));
#36822=CARTESIAN_POINT('Ctrl Pts',(-4.1650163665385,-1.,0.238196140933976));
#36823=CARTESIAN_POINT('Ctrl Pts',(-4.1581638926525,-1.,0.234419749543143));
#36824=CARTESIAN_POINT('Ctrl Pts',(-4.15130247435029,-1.,0.230677299028738));
#36825=CARTESIAN_POINT('Ctrl Pts',(-4.14443220607733,-1.,0.226969025061243));
#36826=CARTESIAN_POINT('Ctrl Pts',(-4.13755320553563,-1.,0.223295201038383));
#36827=CARTESIAN_POINT('Ctrl Pts',(-4.13066558698156,-1.,0.219656126701851));
#36828=CARTESIAN_POINT('Ctrl Pts',(-4.12376943492249,-1.,0.216052116898425));
#36829=CARTESIAN_POINT('Ctrl Pts',(-4.11686478264545,-1.,0.212483491087068));
#36830=CARTESIAN_POINT('Ctrl Pts',(-4.10995157639026,-1.,0.208950559400172));
#36831=CARTESIAN_POINT('Ctrl Pts',(-4.10302969965374,-1.,0.205453622198233));
#36832=CARTESIAN_POINT('Ctrl Pts',(-4.09609903751912,-1.,0.201992979049984));
#36833=CARTESIAN_POINT('Ctrl Pts',(-4.08915953359753,-1.,0.19856893480081));
#36834=CARTESIAN_POINT('Ctrl Pts',(-4.08221124060385,-1.,0.195181806054714));
#36835=CARTESIAN_POINT('Ctrl Pts',(-4.07525439703137,-1.,0.191831928181081));
#36836=CARTESIAN_POINT('Ctrl Pts',(-4.06828941192308,-1.,0.188519658060255));
#36837=CARTESIAN_POINT('Ctrl Pts',(-4.06131670998589,-1.,0.185245370038948));
#36838=CARTESIAN_POINT('Ctrl Pts',(-4.05433660358402,-1.,0.18200945304855));
#36839=CARTESIAN_POINT('Ctrl Pts',(-4.04734916719722,-1.,0.178812307240715));
#36840=CARTESIAN_POINT('Ctrl Pts',(-4.04035407891161,-1.,0.175654339673757));
#36841=CARTESIAN_POINT('Ctrl Pts',(-4.03335057326093,-1.,0.172535962484466));
#36842=CARTESIAN_POINT('Ctrl Pts',(-4.0263377970371,-1.,0.169457601001653));
#36843=CARTESIAN_POINT('Ctrl Pts',(-4.01931510507143,-1.,0.166419700015847));
#36844=CARTESIAN_POINT('Ctrl Pts',(-4.01228237022301,-1.,0.163422730287458));
#36845=CARTESIAN_POINT('Ctrl Pts',(-4.00524031064509,-1.,0.160467194882219));
#36846=CARTESIAN_POINT('Ctrl Pts',(-3.99819074631874,-1.,0.157553634383809));
#36847=CARTESIAN_POINT('Ctrl Pts',(-3.99113582086059,-1.,0.154682618338563));
#36848=CARTESIAN_POINT('Ctrl Pts',(-3.9840772985098,-1.,0.151854737441405));
#36849=CARTESIAN_POINT('Ctrl Pts',(-3.97701581473643,-1.,0.149070594803543));
#36850=CARTESIAN_POINT('Ctrl Pts',(-3.96995018565891,-1.,0.146330797814513));
#36851=CARTESIAN_POINT('Ctrl Pts',(-3.96287658098896,-1.,0.143635947692791));
#36852=CARTESIAN_POINT('Ctrl Pts',(-3.95579014116899,-1.,0.140986665829937));
#36853=CARTESIAN_POINT('Ctrl Pts',(-3.94868667844355,-1.,0.138383621255159));
#36854=CARTESIAN_POINT('Ctrl Pts',(-3.94156445130744,-1.,0.135827558661188));
#36855=CARTESIAN_POINT('Ctrl Pts',(-3.93442567551035,-1.,0.133319322794189));
#36856=CARTESIAN_POINT('Ctrl Pts',(-3.9272787679596,-1.,0.130859892027798));
#36857=CARTESIAN_POINT('Ctrl Pts',(-3.92013513251642,-1.,0.128450341339528));
#36858=CARTESIAN_POINT('Ctrl Pts',(-3.91300501605392,-1.,0.126091793324136));
#36859=CARTESIAN_POINT('Ctrl Pts',(-3.90589336320508,-1.,0.123785368272377));
#36860=CARTESIAN_POINT('Ctrl Pts',(-3.89879639336952,-1.,0.121532144765723));
#36861=CARTESIAN_POINT('Ctrl Pts',(-3.89169600105201,-1.,0.119333088190417));
#36862=CARTESIAN_POINT('Ctrl Pts',(-3.88456590045767,-1.,0.117189150373144));
#36863=CARTESIAN_POINT('Ctrl Pts',(-3.87738168405343,-1.,0.11510142664947));
#36864=CARTESIAN_POINT('Ctrl Pts',(-3.87013043445014,-1.,0.113071304914561));
#36865=CARTESIAN_POINT('Ctrl Pts',(-3.86281867282965,-1.,0.11110059303626));
#36866=CARTESIAN_POINT('Ctrl Pts',(-3.855485714969,-1.,0.109191717634943));
#36867=CARTESIAN_POINT('Ctrl Pts',(-3.84819233070317,-1.,0.107347597812183));
#36868=CARTESIAN_POINT('Ctrl Pts',(-3.84099658324803,-1.,0.105571360916569));
#36869=CARTESIAN_POINT('Ctrl Pts',(-3.83393171228002,-1.,0.103866063811622));
#36870=CARTESIAN_POINT('Ctrl Pts',(-3.82698737143255,-1.,0.102234506488456));
#36871=CARTESIAN_POINT('Ctrl Pts',(-3.82007889742625,-1.,0.100678769650632));
#36872=CARTESIAN_POINT('Ctrl Pts',(-3.81306649386461,-1.,0.0992008728096513));
#36873=CARTESIAN_POINT('Ctrl Pts',(-3.80581088847809,-1.,0.0978042222906642));
#36874=CARTESIAN_POINT('Ctrl Pts',(-3.79822128513845,-1.,0.0964949352873131));
#36875=CARTESIAN_POINT('Ctrl Pts',(-3.79030016353111,-1.,0.09528298851008));
#36876=CARTESIAN_POINT('Ctrl Pts',(-3.782205218991,-1.,0.0941840095090813));
#36877=CARTESIAN_POINT('Ctrl Pts',(-3.77424159971059,-1.,0.0932185546203178));
#36878=CARTESIAN_POINT('Ctrl Pts',(-3.76678860031841,-1.,0.092409058960269));
#36879=CARTESIAN_POINT('Ctrl Pts',(-3.76024199359303,-1.,0.0917773084998334));
#36880=CARTESIAN_POINT('Ctrl Pts',(-3.75495560118212,-1.,0.0913419622736397));
#36881=CARTESIAN_POINT('Ctrl Pts',(-3.75145357872422,-1.,0.0911323999574425));
#36882=CARTESIAN_POINT('Ctrl Pts',(-3.74976844886346,-1.,0.0911090736805509));
#36883=CARTESIAN_POINT('Ctrl Pts',(-3.74911539914542,-1.,0.0911666301812817));
#36884=CARTESIAN_POINT('Ctrl Pts',(-3.74892890040975,-1.,0.0912308016421982));
#36885=CARTESIAN_POINT('Ctrl Pts',(-3.74888939116255,-1.,0.0912596999166822));
#36886=CARTESIAN_POINT('',(-3.74888939116259,-1.,-0.0912596999148858));
#36887=CARTESIAN_POINT('Origin',(0.,-1.,0.));
#36888=CARTESIAN_POINT('',(-4.1923339003649,-1.,-0.253646344052522));
#36889=CARTESIAN_POINT('Ctrl Pts',(-3.74888939116259,-1.,-0.0912596999148858));
#36890=CARTESIAN_POINT('Ctrl Pts',(-3.74892890041021,-1.,-0.0912308016409232));
#36891=CARTESIAN_POINT('Ctrl Pts',(-3.74911539914664,-1.,-0.0911666301806425));
#36892=CARTESIAN_POINT('Ctrl Pts',(-3.74976844886495,-1.,-0.0911090736804571));
#36893=CARTESIAN_POINT('Ctrl Pts',(-3.75145357872511,-1.,-0.0911323999576144));
#36894=CARTESIAN_POINT('Ctrl Pts',(-3.75495560118053,-1.,-0.0913419622735852));
#36895=CARTESIAN_POINT('Ctrl Pts',(-3.76024199359493,-1.,-0.0917773084999007));
#36896=CARTESIAN_POINT('Ctrl Pts',(-3.76678860032228,-1.,-0.0924090589604056));
#36897=CARTESIAN_POINT('Ctrl Pts',(-3.77424159971456,-1.,-0.0932185546204574));
#36898=CARTESIAN_POINT('Ctrl Pts',(-3.78220521899366,-1.,-0.0941840095091744));
#36899=CARTESIAN_POINT('Ctrl Pts',(-3.79030016353186,-1.,-0.0952829885101068));
#36900=CARTESIAN_POINT('Ctrl Pts',(-3.7982212851376,-1.,-0.0964949352872844));
#36901=CARTESIAN_POINT('Ctrl Pts',(-3.80581088847642,-1.,-0.0978042222906075));
#36902=CARTESIAN_POINT('Ctrl Pts',(-3.81306649386293,-1.,-0.0992008728095943));
#36903=CARTESIAN_POINT('Ctrl Pts',(-3.82007889742512,-1.,-0.100678769650594));
#36904=CARTESIAN_POINT('Ctrl Pts',(-3.8269873714322,-1.,-0.102234506488445));
#36905=CARTESIAN_POINT('Ctrl Pts',(-3.83393171228034,-1.,-0.103866063811634));
#36906=CARTESIAN_POINT('Ctrl Pts',(-3.84099658324873,-1.,-0.105571360916593));
#36907=CARTESIAN_POINT('Ctrl Pts',(-3.84819233070391,-1.,-0.107347597812208));
#36908=CARTESIAN_POINT('Ctrl Pts',(-3.85548571496953,-1.,-0.109191717634961));
#36909=CARTESIAN_POINT('Ctrl Pts',(-3.86281867282984,-1.,-0.111100593036267));
#36910=CARTESIAN_POINT('Ctrl Pts',(-3.87013043445001,-1.,-0.113071304914559));
#36911=CARTESIAN_POINT('Ctrl Pts',(-3.87738168405308,-1.,-0.115101426649461));
#36912=CARTESIAN_POINT('Ctrl Pts',(-3.88456590045726,-1.,-0.117189150373134));
#36913=CARTESIAN_POINT('Ctrl Pts',(-3.8916960010517,-1.,-0.11933308819041));
#36914=CARTESIAN_POINT('Ctrl Pts',(-3.89879639336939,-1.,-0.121532144765721));
#36915=CARTESIAN_POINT('Ctrl Pts',(-3.90589336320515,-1.,-0.12378536827238));
#36916=CARTESIAN_POINT('Ctrl Pts',(-3.91300501605411,-1.,-0.126091793324141));
#36917=CARTESIAN_POINT('Ctrl Pts',(-3.92013513251664,-1.,-0.128450341339532));
#36918=CARTESIAN_POINT('Ctrl Pts',(-3.92727876795977,-1.,-0.130859892027801));
#36919=CARTESIAN_POINT('Ctrl Pts',(-3.93442567551042,-1.,-0.133319322794191));
#36920=CARTESIAN_POINT('Ctrl Pts',(-3.94156445130741,-1.,-0.135827558661188));
#36921=CARTESIAN_POINT('Ctrl Pts',(-3.94868667844347,-1.,-0.138383621255161));
#36922=CARTESIAN_POINT('Ctrl Pts',(-3.95579014116894,-1.,-0.140986665829942));
#36923=CARTESIAN_POINT('Ctrl Pts',(-3.96287658098896,-1.,-0.143635947692799));
#36924=CARTESIAN_POINT('Ctrl Pts',(-3.96995018565893,-1.,-0.14633079781452));
#36925=CARTESIAN_POINT('Ctrl Pts',(-3.97701581473644,-1.,-0.149070594803545));
#36926=CARTESIAN_POINT('Ctrl Pts',(-3.98407729850975,-1.,-0.151854737441398));
#36927=CARTESIAN_POINT('Ctrl Pts',(-3.99113582086043,-1.,-0.154682618338547));
#36928=CARTESIAN_POINT('Ctrl Pts',(-3.9981907463185,-1.,-0.15755363438379));
#36929=CARTESIAN_POINT('Ctrl Pts',(-4.00524031064487,-1.,-0.160467194882203));
#36930=CARTESIAN_POINT('Ctrl Pts',(-4.01228237022296,-1.,-0.163422730287456));
#36931=CARTESIAN_POINT('Ctrl Pts',(-4.01931510507167,-1.,-0.166419700015866));
#36932=CARTESIAN_POINT('Ctrl Pts',(-4.02633779703764,-1.,-0.169457601001691));
#36933=CARTESIAN_POINT('Ctrl Pts',(-4.03335057326163,-1.,-0.172535962484514));
#36934=CARTESIAN_POINT('Ctrl Pts',(-4.04035407891222,-1.,-0.175654339673797));
#36935=CARTESIAN_POINT('Ctrl Pts',(-4.04734916719741,-1.,-0.178812307240728));
#36936=CARTESIAN_POINT('Ctrl Pts',(-4.05433660358353,-1.,-0.18200945304852));
#36937=CARTESIAN_POINT('Ctrl Pts',(-4.06131670998469,-1.,-0.185245370038874));
#36938=CARTESIAN_POINT('Ctrl Pts',(-4.06828941192148,-1.,-0.188519658060155));
#36939=CARTESIAN_POINT('Ctrl Pts',(-4.07525439702992,-1.,-0.191831928180991));
#36940=CARTESIAN_POINT('Ctrl Pts',(-4.08221124060322,-1.,-0.195181806054676));
#36941=CARTESIAN_POINT('Ctrl Pts',(-4.08915953359833,-1.,-0.198568934800862));
#36942=CARTESIAN_POINT('Ctrl Pts',(-4.09609903752152,-1.,-0.201992979050136));
#36943=CARTESIAN_POINT('Ctrl Pts',(-4.10302969965728,-1.,-0.205453622198455));
#36944=CARTESIAN_POINT('Ctrl Pts',(-4.10995157639377,-1.,-0.208950559400392));
#36945=CARTESIAN_POINT('Ctrl Pts',(-4.11686478264739,-1.,-0.21248349108719));
#36946=CARTESIAN_POINT('Ctrl Pts',(-4.12376943492132,-1.,-0.216052116898352));
#36947=CARTESIAN_POINT('Ctrl Pts',(-4.13066558697658,-1.,-0.219656126701541));
#36948=CARTESIAN_POINT('Ctrl Pts',(-4.13755320552764,-1.,-0.223295201037886));
#36949=CARTESIAN_POINT('Ctrl Pts',(-4.14443220606869,-1.,-0.226969025060705));
#36950=CARTESIAN_POINT('Ctrl Pts',(-4.15130247434459,-1.,-0.230677299028383));
#36951=CARTESIAN_POINT('Ctrl Pts',(-4.15816389265352,-1.,-0.234419749543208));
#36952=CARTESIAN_POINT('Ctrl Pts',(-4.16501636654877,-1.,-0.238196140934616));
#36953=CARTESIAN_POINT('Ctrl Pts',(-4.17185984411426,-1.,-0.242006283925088));
#36954=CARTESIAN_POINT('Ctrl Pts',(-4.1786943019518,-1.,-0.245850033420019));
#36955=CARTESIAN_POINT('Ctrl Pts',(-4.18415464961466,-1.,-0.248951836912189));
#36956=CARTESIAN_POINT('Ctrl Pts',(-4.18824585245272,-1.,-0.251293239838441));
#36957=CARTESIAN_POINT('Ctrl Pts',(-4.19097151819684,-1.,-0.25286086157284));
#36958=CARTESIAN_POINT('Ctrl Pts',(-4.1923339003649,-1.,-0.253646344052522));
#36959=CARTESIAN_POINT('',(-4.18039834341342,-1.,-0.40530197431835));
#36960=CARTESIAN_POINT('',(-4.1923339003649,-1.,-0.253646344052522));
#36961=CARTESIAN_POINT('',(-3.71701050416825,-1.,-0.496319364827592));
#36962=CARTESIAN_POINT('Ctrl Pts',(-4.18039834341342,-1.,-0.40530197431835));
#36963=CARTESIAN_POINT('Ctrl Pts',(-4.17892985789466,-1.,-0.40586466267921));
#36964=CARTESIAN_POINT('Ctrl Pts',(-4.17599251954382,-1.,-0.406986596325455));
#36965=CARTESIAN_POINT('Ctrl Pts',(-4.17158541007977,-1.,-0.408659167568273));
#36966=CARTESIAN_POINT('Ctrl Pts',(-4.16570705938425,-1.,-0.410868596146414));
#36967=CARTESIAN_POINT('Ctrl Pts',(-4.15835545017202,-1.,-0.41359587795147));
#36968=CARTESIAN_POINT('Ctrl Pts',(-4.15100018949965,-1.,-0.416288556008012));
#36969=CARTESIAN_POINT('Ctrl Pts',(-4.14364132317121,-1.,-0.418946490667703));
#36970=CARTESIAN_POINT('Ctrl Pts',(-4.13627893207002,-1.,-0.421569503104513));
#36971=CARTESIAN_POINT('Ctrl Pts',(-4.12891314634572,-1.,-0.424157375323975));
#36972=CARTESIAN_POINT('Ctrl Pts',(-4.12154412502007,-1.,-0.426709855707));
#36973=CARTESIAN_POINT('Ctrl Pts',(-4.11417202783267,-1.,-0.429226666075845));
#36974=CARTESIAN_POINT('Ctrl Pts',(-4.10679698750336,-1.,-0.431707508679884));
#36975=CARTESIAN_POINT('Ctrl Pts',(-4.09941908688373,-1.,-0.43415207320046));
#36976=CARTESIAN_POINT('Ctrl Pts',(-4.09203832139089,-1.,-0.436560044913482));
#36977=CARTESIAN_POINT('Ctrl Pts',(-4.08465462294273,-1.,-0.438931108931279));
#36978=CARTESIAN_POINT('Ctrl Pts',(-4.07726792490016,-1.,-0.44126495139636));
#36979=CARTESIAN_POINT('Ctrl Pts',(-4.0698782192569,-1.,-0.443561262395333));
#36980=CARTESIAN_POINT('Ctrl Pts',(-4.06248560760659,-1.,-0.445819737468538));
#36981=CARTESIAN_POINT('Ctrl Pts',(-4.0550903779696,-1.,-0.448040082684114));
#36982=CARTESIAN_POINT('Ctrl Pts',(-4.0476929901813,-1.,-0.450222009543926));
#36983=CARTESIAN_POINT('Ctrl Pts',(-4.04029392228049,-1.,-0.452365214748892));
#36984=CARTESIAN_POINT('Ctrl Pts',(-4.03289354362794,-1.,-0.454469363020542));
#36985=CARTESIAN_POINT('Ctrl Pts',(-4.02549199038394,-1.,-0.456534070784951));
#36986=CARTESIAN_POINT('Ctrl Pts',(-4.01808900827587,-1.,-0.458558885636945));
#36987=CARTESIAN_POINT('Ctrl Pts',(-4.01068390573399,-1.,-0.460543280768515));
#36988=CARTESIAN_POINT('Ctrl Pts',(-4.00327590659075,-1.,-0.462486702616205));
#36989=CARTESIAN_POINT('Ctrl Pts',(-3.9958644432011,-1.,-0.464388610938975));
#36990=CARTESIAN_POINT('Ctrl Pts',(-3.98844946363262,-1.,-0.46624852088304));
#36991=CARTESIAN_POINT('Ctrl Pts',(-3.98103175589371,-1.,-0.468066047920157));
#36992=CARTESIAN_POINT('Ctrl Pts',(-3.97361320212436,-1.,-0.469840942829895));
#36993=CARTESIAN_POINT('Ctrl Pts',(-3.96619600864643,-1.,-0.471572978413503));
#36994=CARTESIAN_POINT('Ctrl Pts',(-3.95878201038338,-1.,-0.473261847236297));
#36995=CARTESIAN_POINT('Ctrl Pts',(-3.95137192932897,-1.,-0.47490705302179));
#36996=CARTESIAN_POINT('Ctrl Pts',(-3.94396469119383,-1.,-0.476507810658537));
#36997=CARTESIAN_POINT('Ctrl Pts',(-3.93655660689819,-1.,-0.478062927140964));
#36998=CARTESIAN_POINT('Ctrl Pts',(-3.92914297392071,-1.,-0.479571028525579));
#36999=CARTESIAN_POINT('Ctrl Pts',(-3.92171976072341,-1.,-0.481030798910748));
#37000=CARTESIAN_POINT('Ctrl Pts',(-3.91428536373751,-1.,-0.482441230340713));
#37001=CARTESIAN_POINT('Ctrl Pts',(-3.90684210358056,-1.,-0.48380183508915));
#37002=CARTESIAN_POINT('Ctrl Pts',(-3.89939844658513,-1.,-0.485112963522222));
#37003=CARTESIAN_POINT('Ctrl Pts',(-3.89196582437552,-1.,-0.486375337854103));
#37004=CARTESIAN_POINT('Ctrl Pts',(-3.88455453328138,-1.,-0.487589452275154));
#37005=CARTESIAN_POINT('Ctrl Pts',(-3.87716963231109,-1.,-0.488754973798274));
#37006=CARTESIAN_POINT('Ctrl Pts',(-3.86980755613707,-1.,-0.489870245704918));
#37007=CARTESIAN_POINT('Ctrl Pts',(-3.86245057319246,-1.,-0.490931482170891));
#37008=CARTESIAN_POINT('Ctrl Pts',(-3.85507287020263,-1.,-0.491933631083813));
#37009=CARTESIAN_POINT('Ctrl Pts',(-3.84765051147999,-1.,-0.492871792414141));
#37010=CARTESIAN_POINT('Ctrl Pts',(-3.84017095578451,-1.,-0.493742574629134));
#37011=CARTESIAN_POINT('Ctrl Pts',(-3.83264092682431,-1.,-0.494545212256401));
#37012=CARTESIAN_POINT('Ctrl Pts',(-3.82509963594103,-1.,-0.495283458893837));
#37013=CARTESIAN_POINT('Ctrl Pts',(-3.81760756144025,-1.,-0.49596393787548));
#37014=CARTESIAN_POINT('Ctrl Pts',(-3.81022254090839,-1.,-0.496592643443704));
#37015=CARTESIAN_POINT('Ctrl Pts',(-3.80297788298514,-1.,-0.497171756201052));
#37016=CARTESIAN_POINT('Ctrl Pts',(-3.79586380669994,-1.,-0.497696892100625));
#37017=CARTESIAN_POINT('Ctrl Pts',(-3.78879701661264,-1.,-0.498152751800958));
#37018=CARTESIAN_POINT('Ctrl Pts',(-3.78163975337356,-1.,-0.498515471679585));
#37019=CARTESIAN_POINT('Ctrl Pts',(-3.77425499225255,-1.,-0.498759900365892));
#37020=CARTESIAN_POINT('Ctrl Pts',(-3.76655401191229,-1.,-0.49886579233529));
#37021=CARTESIAN_POINT('Ctrl Pts',(-3.75854082221053,-1.,-0.498823681615422));
#37022=CARTESIAN_POINT('Ctrl Pts',(-3.75037362167839,-1.,-0.498642802042606));
#37023=CARTESIAN_POINT('Ctrl Pts',(-3.74235701734714,-1.,-0.498350586057692));
#37024=CARTESIAN_POINT('Ctrl Pts',(-3.73486914372449,-1.,-0.497984209510024));
#37025=CARTESIAN_POINT('Ctrl Pts',(-3.72830430904606,-1.,-0.497584067153049));
#37026=CARTESIAN_POINT('Ctrl Pts',(-3.72301489774398,-1.,-0.497187079575988));
#37027=CARTESIAN_POINT('Ctrl Pts',(-3.71952320822499,-1.,-0.496846224822563));
#37028=CARTESIAN_POINT('Ctrl Pts',(-3.71785517607549,-1.,-0.496605651525989));
#37029=CARTESIAN_POINT('Ctrl Pts',(-3.71721917030355,-1.,-0.496446644158005));
#37030=CARTESIAN_POINT('Ctrl Pts',(-3.71704500630495,-1.,-0.496354087924313));
#37031=CARTESIAN_POINT('Ctrl Pts',(-3.71701050416825,-1.,-0.496319364827592));
#37032=CARTESIAN_POINT('',(-3.68845817949618,-1.,-0.676591647973661));
#37033=CARTESIAN_POINT('Origin',(0.,-1.,0.));
#37034=CARTESIAN_POINT('',(-4.10104028313088,-1.,-0.906349047628866));
#37035=CARTESIAN_POINT('Ctrl Pts',(-3.68845817949618,-1.,-0.676591647973661));
#37036=CARTESIAN_POINT('Ctrl Pts',(-3.68850172300543,-1.,-0.67656928609342));
#37037=CARTESIAN_POINT('Ctrl Pts',(-3.68869596426099,-1.,-0.676535079520365));
#37038=CARTESIAN_POINT('Ctrl Pts',(-3.68934997767391,-1.,-0.676580391119535));
#37039=CARTESIAN_POINT('Ctrl Pts',(-3.6910107117555,-1.,-0.676867042599711));
#37040=CARTESIAN_POINT('Ctrl Pts',(-3.69443683573443,-1.,-0.677621861865196));
#37041=CARTESIAN_POINT('Ctrl Pts',(-3.69959004073192,-1.,-0.678878822226389));
#37042=CARTESIAN_POINT('Ctrl Pts',(-3.70595722032165,-1.,-0.680526909711617));
#37043=CARTESIAN_POINT('Ctrl Pts',(-3.71319182790334,-1.,-0.682492345109689));
#37044=CARTESIAN_POINT('Ctrl Pts',(-3.7209063713952,-1.,-0.684691698168355));
#37045=CARTESIAN_POINT('Ctrl Pts',(-3.72872973554125,-1.,-0.687043475232499));
#37046=CARTESIAN_POINT('Ctrl Pts',(-3.73636374474993,-1.,-0.689479637354651));
#37047=CARTESIAN_POINT('Ctrl Pts',(-3.74365508986548,-1.,-0.691960080400503));
#37048=CARTESIAN_POINT('Ctrl Pts',(-3.7506028824329,-1.,-0.694474562581173));
#37049=CARTESIAN_POINT('Ctrl Pts',(-3.75729775766913,-1.,-0.69703124565953));
#37050=CARTESIAN_POINT('Ctrl Pts',(-3.76387780603725,-1.,-0.699648552230851));
#37051=CARTESIAN_POINT('Ctrl Pts',(-3.77048141872904,-1.,-0.702346356621613));
#37052=CARTESIAN_POINT('Ctrl Pts',(-3.77719254217197,-1.,-0.705135847999949));
#37053=CARTESIAN_POINT('Ctrl Pts',(-3.78402183336678,-1.,-0.7080158793756));
#37054=CARTESIAN_POINT('Ctrl Pts',(-3.79093694007146,-1.,-0.710978231689117));
#37055=CARTESIAN_POINT('Ctrl Pts',(-3.79788100314994,-1.,-0.714010733006677));
#37056=CARTESIAN_POINT('Ctrl Pts',(-3.80479445759296,-1.,-0.717100993669091));
#37057=CARTESIAN_POINT('Ctrl Pts',(-3.81163885127309,-1.,-0.720240466589172));
#37058=CARTESIAN_POINT('Ctrl Pts',(-3.81840802610795,-1.,-0.723426346019349));
#37059=CARTESIAN_POINT('Ctrl Pts',(-3.82511495756682,-1.,-0.726659281876608));
#37060=CARTESIAN_POINT('Ctrl Pts',(-3.8317839240337,-1.,-0.729942010490145));
#37061=CARTESIAN_POINT('Ctrl Pts',(-3.83844103658016,-1.,-0.73327770375609));
#37062=CARTESIAN_POINT('Ctrl Pts',(-3.84510432881231,-1.,-0.736668240497151));
#37063=CARTESIAN_POINT('Ctrl Pts',(-3.85177770351237,-1.,-0.740113146827176));
#37064=CARTESIAN_POINT('Ctrl Pts',(-3.85845645217611,-1.,-0.743610542737042));
#37065=CARTESIAN_POINT('Ctrl Pts',(-3.86513062969896,-1.,-0.747157716488884));
#37066=CARTESIAN_POINT('Ctrl Pts',(-3.87178914078372,-1.,-0.750751822383023));
#37067=CARTESIAN_POINT('Ctrl Pts',(-3.87842382520058,-1.,-0.754390577396846));
#37068=CARTESIAN_POINT('Ctrl Pts',(-3.88503262662684,-1.,-0.758072800564798));
#37069=CARTESIAN_POINT('Ctrl Pts',(-3.89161738162245,-1.,-0.761798028793978));
#37070=CARTESIAN_POINT('Ctrl Pts',(-3.89818233104381,-1.,-0.765566256401306));
#37071=CARTESIAN_POINT('Ctrl Pts',(-3.90473237182634,-1.,-0.769377629847876));
#37072=CARTESIAN_POINT('Ctrl Pts',(-3.91127138115238,-1.,-0.773232154506305));
#37073=CARTESIAN_POINT('Ctrl Pts',(-3.91780062334464,-1.,-0.777129415664915));
#37074=CARTESIAN_POINT('Ctrl Pts',(-3.92431956510418,-1.,-0.781068718228395));
#37075=CARTESIAN_POINT('Ctrl Pts',(-3.93082655631768,-1.,-0.785049202786458));
#37076=CARTESIAN_POINT('Ctrl Pts',(-3.93731956885671,-1.,-0.789069971469323));
#37077=CARTESIAN_POINT('Ctrl Pts',(-3.94379688971307,-1.,-0.793130205641017));
#37078=CARTESIAN_POINT('Ctrl Pts',(-3.95025788827189,-1.,-0.797229296085438));
#37079=CARTESIAN_POINT('Ctrl Pts',(-3.95670276375176,-1.,-0.801366797727206));
#37080=CARTESIAN_POINT('Ctrl Pts',(-3.96313222295874,-1.,-0.805542372178496));
#37081=CARTESIAN_POINT('Ctrl Pts',(-3.96954717513251,-1.,-0.809755732818134));
#37082=CARTESIAN_POINT('Ctrl Pts',(-3.97594844078763,-1.,-0.814006592328737));
#37083=CARTESIAN_POINT('Ctrl Pts',(-3.98233640155287,-1.,-0.818294599022033));
#37084=CARTESIAN_POINT('Ctrl Pts',(-3.98871104646328,-1.,-0.822619346021769));
#37085=CARTESIAN_POINT('Ctrl Pts',(-3.99507212784289,-1.,-0.826980400320473));
#37086=CARTESIAN_POINT('Ctrl Pts',(-4.00141928477447,-1.,-0.831377325741487));
#37087=CARTESIAN_POINT('Ctrl Pts',(-4.00775216907934,-1.,-0.835809705809821));
#37088=CARTESIAN_POINT('Ctrl Pts',(-4.01407059766338,-1.,-0.84027717197638));
#37089=CARTESIAN_POINT('Ctrl Pts',(-4.02037456798787,-1.,-0.844779403288517));
#37090=CARTESIAN_POINT('Ctrl Pts',(-4.02666418343508,-1.,-0.849316107475012));
#37091=CARTESIAN_POINT('Ctrl Pts',(-4.03293960436945,-1.,-0.853887006632178));
#37092=CARTESIAN_POINT('Ctrl Pts',(-4.03920099284658,-1.,-0.858491822322571));
#37093=CARTESIAN_POINT('Ctrl Pts',(-4.04544845048097,-1.,-0.863130256642173));
#37094=CARTESIAN_POINT('Ctrl Pts',(-4.05168199437128,-1.,-0.867801988858176));
#37095=CARTESIAN_POINT('Ctrl Pts',(-4.05790159030495,-1.,-0.872506694780563));
#37096=CARTESIAN_POINT('Ctrl Pts',(-4.06410717232347,-1.,-0.877244060484595));
#37097=CARTESIAN_POINT('Ctrl Pts',(-4.07029866694292,-1.,-0.882013797525916));
#37098=CARTESIAN_POINT('Ctrl Pts',(-4.07647601774639,-1.,-0.886815658360739));
#37099=CARTESIAN_POINT('Ctrl Pts',(-4.08263920306651,-1.,-0.891649447920401));
#37100=CARTESIAN_POINT('Ctrl Pts',(-4.08878822249095,-1.,-0.896515019236368));
#37101=CARTESIAN_POINT('Ctrl Pts',(-4.09369611524319,-1.,-0.900432820945975));
#37102=CARTESIAN_POINT('Ctrl Pts',(-4.09737067247114,-1.,-0.903385402444212));
#37103=CARTESIAN_POINT('Ctrl Pts',(-4.09981755067956,-1.,-0.905360112216302));
#37104=CARTESIAN_POINT('Ctrl Pts',(-4.10104028313088,-1.,-0.906349047628866));
#37105=CARTESIAN_POINT('',(-4.06552750530042,-1.,-1.05427041296137));
#37106=CARTESIAN_POINT('',(-4.10104028313088,-1.,-0.906349047628866));
#37107=CARTESIAN_POINT('',(-3.59360648251073,-1.,-1.07167739962028));
#37108=CARTESIAN_POINT('Ctrl Pts',(-4.06552750530042,-1.,-1.05427041296137));
#37109=CARTESIAN_POINT('Ctrl Pts',(-4.06398907542249,-1.,-1.05459645194823));
#37110=CARTESIAN_POINT('Ctrl Pts',(-4.06091239149123,-1.,-1.05524507177599));
#37111=CARTESIAN_POINT('Ctrl Pts',(-4.05629789307025,-1.,-1.05620762707996));
#37112=CARTESIAN_POINT('Ctrl Pts',(-4.05014628384869,-1.,-1.05747027727959));
#37113=CARTESIAN_POINT('Ctrl Pts',(-4.04245854427496,-1.,-1.05901393666566));
#37114=CARTESIAN_POINT('Ctrl Pts',(-4.03477261141553,-1.,-1.06052284711857));
#37115=CARTESIAN_POINT('Ctrl Pts',(-4.02708855235633,-1.,-1.06199687787462));
#37116=CARTESIAN_POINT('Ctrl Pts',(-4.01940647495943,-1.,-1.06343586496236));
#37117=CARTESIAN_POINT('Ctrl Pts',(-4.01172654187398,-1.,-1.06483961343109));
#37118=CARTESIAN_POINT('Ctrl Pts',(-4.00404894952579,-1.,-1.06620789963606));
#37119=CARTESIAN_POINT('Ctrl Pts',(-3.99637389920441,-1.,-1.06754047381312));
#37120=CARTESIAN_POINT('Ctrl Pts',(-3.98870156857412,-1.,-1.06883706263941));
#37121=CARTESIAN_POINT('Ctrl Pts',(-3.98103208801101,-1.,-1.07009737257767));
#37122=CARTESIAN_POINT('Ctrl Pts',(-3.9733655022223,-1.,-1.07132109206164));
#37123=CARTESIAN_POINT('Ctrl Pts',(-3.96570179322338,-1.,-1.07250789943007));
#37124=CARTESIAN_POINT('Ctrl Pts',(-3.95804094429373,-1.,-1.07365747426491));
#37125=CARTESIAN_POINT('Ctrl Pts',(-3.95038299600676,-1.,-1.07476950921587));
#37126=CARTESIAN_POINT('Ctrl Pts',(-3.94272809633331,-1.,-1.07584371946443));
#37127=CARTESIAN_POINT('Ctrl Pts',(-3.93507657572883,-1.,-1.07687985975384));
#37128=CARTESIAN_POINT('Ctrl Pts',(-3.9274289334984,-1.,-1.07787771707195));
#37129=CARTESIAN_POINT('Ctrl Pts',(-3.91978568924178,-1.,-1.07883706663554));
#37130=CARTESIAN_POINT('Ctrl Pts',(-3.91214726022143,-1.,-1.07975763507473));
#37131=CARTESIAN_POINT('Ctrl Pts',(-3.90451384092545,-1.,-1.08063906483818));
#37132=CARTESIAN_POINT('Ctrl Pts',(-3.8968852509835,-1.,-1.08148086931358));
#37133=CARTESIAN_POINT('Ctrl Pts',(-3.88926088975114,-1.,-1.08228241999346));
#37134=CARTESIAN_POINT('Ctrl Pts',(-3.88164007721312,-1.,-1.08304304871028));
#37135=CARTESIAN_POINT('Ctrl Pts',(-3.8740223372254,-1.,-1.08376213307504));
#37136=CARTESIAN_POINT('Ctrl Pts',(-3.86640769434274,-1.,-1.08443918607927));
#37137=CARTESIAN_POINT('Ctrl Pts',(-3.85879698702532,-1.,-1.08507395120059));
#37138=CARTESIAN_POINT('Ctrl Pts',(-3.85119211322755,-1.,-1.08566647671844));
#37139=CARTESIAN_POINT('Ctrl Pts',(-3.8435952876495,-1.,-1.08621688337604));
#37140=CARTESIAN_POINT('Ctrl Pts',(-3.83600837071708,-1.,-1.08672515456902));
#37141=CARTESIAN_POINT('Ctrl Pts',(-3.82843215316984,-1.,-1.08719091307558));
#37142=CARTESIAN_POINT('Ctrl Pts',(-3.82086569676319,-1.,-1.08761321539442));
#37143=CARTESIAN_POINT('Ctrl Pts',(-3.81330554446323,-1.,-1.08799030610862));
#37144=CARTESIAN_POINT('Ctrl Pts',(-3.8057472665766,-1.,-1.0883200925538));
#37145=CARTESIAN_POINT('Ctrl Pts',(-3.79818708705259,-1.,-1.08860064435778));
#37146=CARTESIAN_POINT('Ctrl Pts',(-3.79062357974404,-1.,-1.08883071512098));
#37147=CARTESIAN_POINT('Ctrl Pts',(-3.78305911299504,-1.,-1.08901018614636));
#37148=CARTESIAN_POINT('Ctrl Pts',(-3.77550199409424,-1.,-1.0891407279127));
#37149=CARTESIAN_POINT('Ctrl Pts',(-3.76796340094448,-1.,-1.08922484204256));
#37150=CARTESIAN_POINT('Ctrl Pts',(-3.76045342580208,-1.,-1.08926462734281));
#37151=CARTESIAN_POINT('Ctrl Pts',(-3.75297711748132,-1.,-1.08926054632925));
#37152=CARTESIAN_POINT('Ctrl Pts',(-3.74553121371757,-1.,-1.08921040494017));
#37153=CARTESIAN_POINT('Ctrl Pts',(-3.73809879348239,-1.,-1.08910769013297));
#37154=CARTESIAN_POINT('Ctrl Pts',(-3.73065515162988,-1.,-1.08894337390937));
#37155=CARTESIAN_POINT('Ctrl Pts',(-3.72317741369398,-1.,-1.08870887220082));
#37156=CARTESIAN_POINT('Ctrl Pts',(-3.71565372339075,-1.,-1.0883988733478));
#37157=CARTESIAN_POINT('Ctrl Pts',(-3.70809084139457,-1.,-1.08801367312185));
#37158=CARTESIAN_POINT('Ctrl Pts',(-3.70052690909833,-1.,-1.08756311291309));
#37159=CARTESIAN_POINT('Ctrl Pts',(-3.69302062410157,-1.,-1.08706319540271));
#37160=CARTESIAN_POINT('Ctrl Pts',(-3.68562817420797,-1.,-1.0865288888259));
#37161=CARTESIAN_POINT('Ctrl Pts',(-3.67838211685117,-1.,-1.0859675575576));
#37162=CARTESIAN_POINT('Ctrl Pts',(-3.67127347729666,-1.,-1.0853733414449));
#37163=CARTESIAN_POINT('Ctrl Pts',(-3.66422237895365,-1.,-1.08471809922901));
#37164=CARTESIAN_POINT('Ctrl Pts',(-3.65709649161166,-1.,-1.08395671077807));
#37165=CARTESIAN_POINT('Ctrl Pts',(-3.64976441208358,-1.,-1.08304289898623));
#37166=CARTESIAN_POINT('Ctrl Pts',(-3.64214167843677,-1.,-1.08194278850996));
#37167=CARTESIAN_POINT('Ctrl Pts',(-3.63423373196529,-1.,-1.08064765719867));
#37168=CARTESIAN_POINT('Ctrl Pts',(-3.62619537902361,-1.,-1.07919137290742));
#37169=CARTESIAN_POINT('Ctrl Pts',(-3.61832318504574,-1.,-1.07764868137619));
#37170=CARTESIAN_POINT('Ctrl Pts',(-3.61098481349204,-1.,-1.07611545402734));
#37171=CARTESIAN_POINT('Ctrl Pts',(-3.60456339887778,-1.,-1.07469327168578));
#37172=CARTESIAN_POINT('Ctrl Pts',(-3.59940121154535,-1.,-1.07347372545714));
#37173=CARTESIAN_POINT('Ctrl Pts',(-3.59600583194946,-1.,-1.07259084660936));
#37174=CARTESIAN_POINT('Ctrl Pts',(-3.59439596999862,-1.,-1.07209229745229));
#37175=CARTESIAN_POINT('Ctrl Pts',(-3.59379266874567,-1.,-1.07183575450617));
#37176=CARTESIAN_POINT('Ctrl Pts',(-3.5936351279798,-1.,-1.07171709254135));
#37177=CARTESIAN_POINT('Ctrl Pts',(-3.59360648251073,-1.,-1.07167739962028));
#37178=CARTESIAN_POINT('',(-3.5372048861597,-1.,-1.24526366418038));
#37179=CARTESIAN_POINT('Origin',(0.,-1.,0.));
#37180=CARTESIAN_POINT('',(-3.90876544355381,-1.,-1.53673442965256));
#37181=CARTESIAN_POINT('Ctrl Pts',(-3.5372048861597,-1.,-1.24526366418038));
#37182=CARTESIAN_POINT('Ctrl Pts',(-3.53725139174486,-1.,-1.24524838931757));
#37183=CARTESIAN_POINT('Ctrl Pts',(-3.5374485926552,-1.,-1.2452449899111));
#37184=CARTESIAN_POINT('Ctrl Pts',(-3.53808746578196,-1.,-1.24539205388767));
#37185=CARTESIAN_POINT('Ctrl Pts',(-3.53968291130022,-1.,-1.24593497226008));
#37186=CARTESIAN_POINT('Ctrl Pts',(-3.54294877425964,-1.,-1.24721646231966));
#37187=CARTESIAN_POINT('Ctrl Pts',(-3.54784190283068,-1.,-1.24926408628003));
#37188=CARTESIAN_POINT('Ctrl Pts',(-3.55387287418985,-1.,-1.2518879294064));
#37189=CARTESIAN_POINT('Ctrl Pts',(-3.56071094991199,-1.,-1.25496090900009));
#37190=CARTESIAN_POINT('Ctrl Pts',(-3.56798645995275,-1.,-1.25834000485716));
#37191=CARTESIAN_POINT('Ctrl Pts',(-3.5753456065171,-1.,-1.2618866714281));
#37192=CARTESIAN_POINT('Ctrl Pts',(-3.58250452868618,-1.,-1.26548706249862));
#37193=CARTESIAN_POINT('Ctrl Pts',(-3.58931807846313,-1.,-1.26907758484709));
#37194=CARTESIAN_POINT('Ctrl Pts',(-3.59578698050006,-1.,-1.27264798379307));
#37195=CARTESIAN_POINT('Ctrl Pts',(-3.60199947736298,-1.,-1.27622049908625));
#37196=CARTESIAN_POINT('Ctrl Pts',(-3.60808907746339,-1.,-1.27983492861691));
#37197=CARTESIAN_POINT('Ctrl Pts',(-3.61418935913823,-1.,-1.28353255117765));
#37198=CARTESIAN_POINT('Ctrl Pts',(-3.6203814849236,-1.,-1.28733755029384));
#37199=CARTESIAN_POINT('Ctrl Pts',(-3.62667616004369,-1.,-1.29125046021878));
#37200=CARTESIAN_POINT('Ctrl Pts',(-3.63304271631046,-1.,-1.29525810207762));
#37201=CARTESIAN_POINT('Ctrl Pts',(-3.63942689872808,-1.,-1.2993395590647));
#37202=CARTESIAN_POINT('Ctrl Pts',(-3.64577181380113,-1.,-1.30347327603774));
#37203=CARTESIAN_POINT('Ctrl Pts',(-3.65204081987068,-1.,-1.30764479590039));
#37204=CARTESIAN_POINT('Ctrl Pts',(-3.65822827358617,-1.,-1.31185038411218));
#37205=CARTESIAN_POINT('Ctrl Pts',(-3.66434688899793,-1.,-1.31609271239911));
#37206=CARTESIAN_POINT('Ctrl Pts',(-3.67042021752656,-1.,-1.32037828137766));
#37207=CARTESIAN_POINT('Ctrl Pts',(-3.67647355257912,-1.,-1.32471430856415));
#37208=CARTESIAN_POINT('Ctrl Pts',(-3.68252441182551,-1.,-1.3291054707274));
#37209=CARTESIAN_POINT('Ctrl Pts',(-3.68857672413033,-1.,-1.33355191034523));
#37210=CARTESIAN_POINT('Ctrl Pts',(-3.69462613305708,-1.,-1.33805103398219));
#37211=CARTESIAN_POINT('Ctrl Pts',(-3.70066324015119,-1.,-1.34259860752933));
#37212=CARTESIAN_POINT('Ctrl Pts',(-3.70667753188248,-1.,-1.34719008463534));
#37213=CARTESIAN_POINT('Ctrl Pts',(-3.71266130563054,-1.,-1.35182193384424));
#37214=CARTESIAN_POINT('Ctrl Pts',(-3.71861271513313,-1.,-1.35649266705037));
#37215=CARTESIAN_POINT('Ctrl Pts',(-3.72453364678279,-1.,-1.36120211416354));
#37216=CARTESIAN_POINT('Ctrl Pts',(-3.73042829011295,-1.,-1.36595093298676));
#37217=CARTESIAN_POINT('Ctrl Pts',(-3.7363014588581,-1.,-1.37074003422739));
#37218=CARTESIAN_POINT('Ctrl Pts',(-3.74215698162555,-1.,-1.37557002971687));
#37219=CARTESIAN_POINT('Ctrl Pts',(-3.74799617204729,-1.,-1.38044070763295));
#37220=CARTESIAN_POINT('Ctrl Pts',(-3.75381861212707,-1.,-1.38535129801176));
#37221=CARTESIAN_POINT('Ctrl Pts',(-3.75962280650855,-1.,-1.39030069388918));
#37222=CARTESIAN_POINT('Ctrl Pts',(-3.76540689249074,-1.,-1.39528769118052));
#37223=CARTESIAN_POINT('Ctrl Pts',(-3.77116930621827,-1.,-1.40031121335505));
#37224=CARTESIAN_POINT('Ctrl Pts',(-3.77690952014259,-1.,-1.40537056004722));
#37225=CARTESIAN_POINT('Ctrl Pts',(-3.78262780065471,-1.,-1.41046532282593));
#37226=CARTESIAN_POINT('Ctrl Pts',(-3.78832489879426,-1.,-1.4155952780383));
#37227=CARTESIAN_POINT('Ctrl Pts',(-3.79400175744408,-1.,-1.42076028482836));
#37228=CARTESIAN_POINT('Ctrl Pts',(-3.7996592319632,-1.,-1.42596018777283));
#37229=CARTESIAN_POINT('Ctrl Pts',(-3.80529775429805,-1.,-1.4311946992132));
#37230=CARTESIAN_POINT('Ctrl Pts',(-3.81091737726815,-1.,-1.43646341556724));
#37231=CARTESIAN_POINT('Ctrl Pts',(-3.81651792398414,-1.,-1.44176587041347));
#37232=CARTESIAN_POINT('Ctrl Pts',(-3.82209910620533,-1.,-1.44710157648539));
#37233=CARTESIAN_POINT('Ctrl Pts',(-3.82766064519074,-1.,-1.45247006796836));
#37234=CARTESIAN_POINT('Ctrl Pts',(-3.83320241775423,-1.,-1.45787095220852));
#37235=CARTESIAN_POINT('Ctrl Pts',(-3.83872447159639,-1.,-1.46330391180752));
#37236=CARTESIAN_POINT('Ctrl Pts',(-3.84422695454796,-1.,-1.46876867426504));
#37237=CARTESIAN_POINT('Ctrl Pts',(-3.84971006847277,-1.,-1.47426499018538));
#37238=CARTESIAN_POINT('Ctrl Pts',(-3.85517401698843,-1.,-1.4797926099102));
#37239=CARTESIAN_POINT('Ctrl Pts',(-3.86061894706087,-1.,-1.48535125509919));
#37240=CARTESIAN_POINT('Ctrl Pts',(-3.86604492575189,-1.,-1.4909406116431));
#37241=CARTESIAN_POINT('Ctrl Pts',(-3.87145196998465,-1.,-1.49656035399122));
#37242=CARTESIAN_POINT('Ctrl Pts',(-3.87684006372134,-1.,-1.50221016176556));
#37243=CARTESIAN_POINT('Ctrl Pts',(-3.88220917950538,-1.,-1.50788973857757));
#37244=CARTESIAN_POINT('Ctrl Pts',(-3.88755930033884,-1.,-1.51359883110559));
#37245=CARTESIAN_POINT('Ctrl Pts',(-3.89289043533657,-1.,-1.51933724329305));
#37246=CARTESIAN_POINT('Ctrl Pts',(-3.89820260708225,-1.,-1.52510482991635));
#37247=CARTESIAN_POINT('Ctrl Pts',(-3.90243719631596,-1.,-1.52974216056287));
#37248=CARTESIAN_POINT('Ctrl Pts',(-3.90560462813969,-1.,-1.53323321827755));
#37249=CARTESIAN_POINT('Ctrl Pts',(-3.90771246855019,-1.,-1.53556639217905));
#37250=CARTESIAN_POINT('Ctrl Pts',(-3.90876544355381,-1.,-1.53673442965256));
#37251=CARTESIAN_POINT('',(-3.85054988729471,-1.,-1.67727921511438));
#37252=CARTESIAN_POINT('',(-3.90876544355381,-1.,-1.53673442965256));
#37253=CARTESIAN_POINT('',(-3.38171594275765,-1.,-1.62064718014094));
#37254=CARTESIAN_POINT('Ctrl Pts',(-3.85054988729471,-1.,-1.67727921511438));
#37255=CARTESIAN_POINT('Ctrl Pts',(-3.84897939430696,-1.,-1.67736057656533));
#37256=CARTESIAN_POINT('Ctrl Pts',(-3.84583912296459,-1.,-1.6775199114018));
#37257=CARTESIAN_POINT('Ctrl Pts',(-3.84113085985244,-1.,-1.67774874946079));
#37258=CARTESIAN_POINT('Ctrl Pts',(-3.83485746513989,-1.,-1.67803353064351));
#37259=CARTESIAN_POINT('Ctrl Pts',(-3.82702289286713,-1.,-1.6783555575934));
#37260=CARTESIAN_POINT('Ctrl Pts',(-3.81919554099578,-1.,-1.67864354605954));
#37261=CARTESIAN_POINT('Ctrl Pts',(-3.81137549624178,-1.,-1.6788973773827));
#37262=CARTESIAN_POINT('Ctrl Pts',(-3.80356289079005,-1.,-1.67911690648355));
#37263=CARTESIAN_POINT('Ctrl Pts',(-3.79575791578424,-1.,-1.67930196625548));
#37264=CARTESIAN_POINT('Ctrl Pts',(-3.7879608002176,-1.,-1.67945236653493));
#37265=CARTESIAN_POINT('Ctrl Pts',(-3.78017178197317,-1.,-1.67956789212141));
#37266=CARTESIAN_POINT('Ctrl Pts',(-3.77239107928502,-1.,-1.67964830084993));
#37267=CARTESIAN_POINT('Ctrl Pts',(-3.76461886684344,-1.,-1.67969332319245));
#37268=CARTESIAN_POINT('Ctrl Pts',(-3.75685523754493,-1.,-1.67970265841239));
#37269=CARTESIAN_POINT('Ctrl Pts',(-3.7491002239452,-1.,-1.67967598599525));
#37270=CARTESIAN_POINT('Ctrl Pts',(-3.74135385965401,-1.,-1.6796129868522));
#37271=CARTESIAN_POINT('Ctrl Pts',(-3.73361623282543,-1.,-1.67951336376402));
#37272=CARTESIAN_POINT('Ctrl Pts',(-3.72588753416396,-1.,-1.67937685856652));
#37273=CARTESIAN_POINT('Ctrl Pts',(-3.71816812842322,-1.,-1.67920328071708));
#37274=CARTESIAN_POINT('Ctrl Pts',(-3.71045854208343,-1.,-1.67899249793462));
#37275=CARTESIAN_POINT('Ctrl Pts',(-3.70275932351108,-1.,-1.67874436948667));
#37276=CARTESIAN_POINT('Ctrl Pts',(-3.6950709275959,-1.,-1.67845869064323));
#37277=CARTESIAN_POINT('Ctrl Pts',(-3.68739360236487,-1.,-1.67813513867965));
#37278=CARTESIAN_POINT('Ctrl Pts',(-3.67972724579124,-1.,-1.67777320475848));
#37279=CARTESIAN_POINT('Ctrl Pts',(-3.67207136294575,-1.,-1.67737217414874));
#37280=CARTESIAN_POINT('Ctrl Pts',(-3.66442538670968,-1.,-1.67693128053132));
#37281=CARTESIAN_POINT('Ctrl Pts',(-3.6567889441642,-1.,-1.67644983469449));
#37282=CARTESIAN_POINT('Ctrl Pts',(-3.64916213574667,-1.,-1.67592735946692));
#37283=CARTESIAN_POINT('Ctrl Pts',(-3.6415458297234,-1.,-1.67536373264848));
#37284=CARTESIAN_POINT('Ctrl Pts',(-3.63394189312924,-1.,-1.67475929882971));
#37285=CARTESIAN_POINT('Ctrl Pts',(-3.62635249450923,-1.,-1.67411452372271));
#37286=CARTESIAN_POINT('Ctrl Pts',(-3.61877947398184,-1.,-1.67342968196224));
#37287=CARTESIAN_POINT('Ctrl Pts',(-3.61122367156181,-1.,-1.67270452466968));
#37288=CARTESIAN_POINT('Ctrl Pts',(-3.603684308152,-1.,-1.67193797318597));
#37289=CARTESIAN_POINT('Ctrl Pts',(-3.59615824388807,-1.,-1.67112775290707));
#37290=CARTESIAN_POINT('Ctrl Pts',(-3.58864143097834,-1.,-1.67027110397604));
#37291=CARTESIAN_POINT('Ctrl Pts',(-3.58113044183829,-1.,-1.66936552908232));
#37292=CARTESIAN_POINT('Ctrl Pts',(-3.57362406285887,-1.,-1.668409574073));
#37293=CARTESIAN_POINT('Ctrl Pts',(-3.56612465179422,-1.,-1.66740349220305));
#37294=CARTESIAN_POINT('Ctrl Pts',(-3.55864015233602,-1.,-1.66635023293114));
#37295=CARTESIAN_POINT('Ctrl Pts',(-3.55118121342861,-1.,-1.66525401568994));
#37296=CARTESIAN_POINT('Ctrl Pts',(-3.54375747475014,-1.,-1.66411849222326));
#37297=CARTESIAN_POINT('Ctrl Pts',(-3.5363738506022,-1.,-1.66294490916111));
#37298=CARTESIAN_POINT('Ctrl Pts',(-3.52902746211093,-1.,-1.66173058912371));
#37299=CARTESIAN_POINT('Ctrl Pts',(-3.52170261543815,-1.,-1.66046645222279));
#37300=CARTESIAN_POINT('Ctrl Pts',(-3.5143763218894,-1.,-1.65913971687342));
#37301=CARTESIAN_POINT('Ctrl Pts',(-3.50702733146542,-1.,-1.65773832633632));
#37302=CARTESIAN_POINT('Ctrl Pts',(-3.4996447647794,-1.,-1.65625517961588));
#37303=CARTESIAN_POINT('Ctrl Pts',(-3.49223525300176,-1.,-1.65469162644468));
#37304=CARTESIAN_POINT('Ctrl Pts',(-3.48483492840894,-1.,-1.65306335367739));
#37305=CARTESIAN_POINT('Ctrl Pts',(-3.47749926256476,-1.,-1.65139534930322));
#37306=CARTESIAN_POINT('Ctrl Pts',(-3.47028140995992,-1.,-1.64971118698256));
#37307=CARTESIAN_POINT('Ctrl Pts',(-3.46321237515,-1.,-1.64802323352738));
#37308=CARTESIAN_POINT('Ctrl Pts',(-3.45628421062422,-1.,-1.64632429697521));
#37309=CARTESIAN_POINT('Ctrl Pts',(-3.44942242546795,-1.,-1.64457408708107));
#37310=CARTESIAN_POINT('Ctrl Pts',(-3.44250337701888,-1.,-1.64270733821113));
#37311=CARTESIAN_POINT('Ctrl Pts',(-3.43540451921548,-1.,-1.64065778702023));
#37312=CARTESIAN_POINT('Ctrl Pts',(-3.42804772926291,-1.,-1.63837876246926));
#37313=CARTESIAN_POINT('Ctrl Pts',(-3.42043974590882,-1.,-1.63586250099773));
#37314=CARTESIAN_POINT('Ctrl Pts',(-3.41272817148478,-1.,-1.63316667054044));
#37315=CARTESIAN_POINT('Ctrl Pts',(-3.40519422740235,-1.,-1.63041148964828));
#37316=CARTESIAN_POINT('Ctrl Pts',(-3.39818605297991,-1.,-1.62774916464408));
#37317=CARTESIAN_POINT('Ctrl Pts',(-3.39206617496906,-1.,-1.62533996116713));
#37318=CARTESIAN_POINT('Ctrl Pts',(-3.38715832179072,-1.,-1.6233278855625));
#37319=CARTESIAN_POINT('Ctrl Pts',(-3.38394285763222,-1.,-1.62192472202769));
#37320=CARTESIAN_POINT('Ctrl Pts',(-3.38243080602409,-1.,-1.62118047294498));
#37321=CARTESIAN_POINT('Ctrl Pts',(-3.38187506456922,-1.,-1.62083271135947));
#37322=CARTESIAN_POINT('Ctrl Pts',(-3.38173802621259,-1.,-1.62069086551492));
#37323=CARTESIAN_POINT('Ctrl Pts',(-3.38171594275765,-1.,-1.62064718014094));
#37324=CARTESIAN_POINT('',(-3.29885386921599,-1.,-1.78327315618183));
#37325=CARTESIAN_POINT('Origin',(0.,-1.,0.));
#37326=CARTESIAN_POINT('',(-3.62024382630768,-1.,-2.12928030988903));
#37327=CARTESIAN_POINT('Ctrl Pts',(-3.29885386921599,-1.,-1.78327315618183));
#37328=CARTESIAN_POINT('Ctrl Pts',(-3.29890219175522,-1.,-1.78326534445426));
#37329=CARTESIAN_POINT('Ctrl Pts',(-3.29909749657945,-1.,-1.78329283591903));
#37330=CARTESIAN_POINT('Ctrl Pts',(-3.29970549824337,-1.,-1.78353803106983));
#37331=CARTESIAN_POINT('Ctrl Pts',(-3.30119637003466,-1.,-1.7843238478823));
#37332=CARTESIAN_POINT('Ctrl Pts',(-3.30422155558973,-1.,-1.78610045419769));
#37333=CARTESIAN_POINT('Ctrl Pts',(-3.30873412266954,-1.,-1.78888832245965));
#37334=CARTESIAN_POINT('Ctrl Pts',(-3.31428038326763,-1.,-1.79242331350137));
#37335=CARTESIAN_POINT('Ctrl Pts',(-3.32055355101168,-1.,-1.79652817033444));
#37336=CARTESIAN_POINT('Ctrl Pts',(-3.3272108803981,-1.,-1.80100380443535));
#37337=CARTESIAN_POINT('Ctrl Pts',(-3.33392460276874,-1.,-1.80565802981138));
#37338=CARTESIAN_POINT('Ctrl Pts',(-3.34043216147532,-1.,-1.81033399625311));
#37339=CARTESIAN_POINT('Ctrl Pts',(-3.34660014370527,-1.,-1.81494618732772));
#37340=CARTESIAN_POINT('Ctrl Pts',(-3.35243086937451,-1.,-1.81948458796748));
#37341=CARTESIAN_POINT('Ctrl Pts',(-3.35800801557326,-1.,-1.82398496829247));
#37342=CARTESIAN_POINT('Ctrl Pts',(-3.36345722124127,-1.,-1.82850752153182));
#37343=CARTESIAN_POINT('Ctrl Pts',(-3.36890396271864,-1.,-1.83311391452338));
#37344=CARTESIAN_POINT('Ctrl Pts',(-3.37442462015914,-1.,-1.83784072967111));
#37345=CARTESIAN_POINT('Ctrl Pts',(-3.38002968341222,-1.,-1.84269016931679));
#37346=CARTESIAN_POINT('Ctrl Pts',(-3.38569092349639,-1.,-1.84764441927778));
#37347=CARTESIAN_POINT('Ctrl Pts',(-3.39135802549415,-1.,-1.85267433291778));
#37348=CARTESIAN_POINT('Ctrl Pts',(-3.39697816833056,-1.,-1.85774972037055));
#37349=CARTESIAN_POINT('Ctrl Pts',(-3.40251742305445,-1.,-1.86285057051228));
#37350=CARTESIAN_POINT('Ctrl Pts',(-3.40797080000513,-1.,-1.86797231196635));
#37351=CARTESIAN_POINT('Ctrl Pts',(-3.41335043875182,-1.,-1.87311957248106));
#37352=CARTESIAN_POINT('Ctrl Pts',(-3.4186785838376,-1.,-1.87830245689338));
#37353=CARTESIAN_POINT('Ctrl Pts',(-3.42397908819741,-1.,-1.88353205062063));
#37354=CARTESIAN_POINT('Ctrl Pts',(-3.42926852222174,-1.,-1.88881571322018));
#37355=CARTESIAN_POINT('Ctrl Pts',(-3.43455074411591,-1.,-1.89415420002553));
#37356=CARTESIAN_POINT('Ctrl Pts',(-3.43982185678105,-1.,-1.89954426803392));
#37357=CARTESIAN_POINT('Ctrl Pts',(-3.44507323983374,-1.,-1.90498026502308));
#37358=CARTESIAN_POINT('Ctrl Pts',(-3.45029522038885,-1.,-1.91045605593638));
#37359=CARTESIAN_POINT('Ctrl Pts',(-3.45548074309943,-1.,-1.9159669478406));
#37360=CARTESIAN_POINT('Ctrl Pts',(-3.4606282172248,-1.,-1.9215111821321));
#37361=CARTESIAN_POINT('Ctrl Pts',(-3.46573953254084,-1.,-1.92708888591159));
#37362=CARTESIAN_POINT('Ctrl Pts',(-3.47081872409783,-1.,-1.93270136427083));
#37363=CARTESIAN_POINT('Ctrl Pts',(-3.47587040389916,-1.,-1.93835026973888));
#37364=CARTESIAN_POINT('Ctrl Pts',(-3.48089825770411,-1.,-1.94403680554062));
#37365=CARTESIAN_POINT('Ctrl Pts',(-3.485903616108,-1.,-1.94976096795902));
#37366=CARTESIAN_POINT('Ctrl Pts',(-3.49088618670967,-1.,-1.95552193112071));
#37367=CARTESIAN_POINT('Ctrl Pts',(-3.49584466573045,-1.,-1.96131836776489));
#37368=CARTESIAN_POINT('Ctrl Pts',(-3.50077740176262,-1.,-1.9671487972405));
#37369=CARTESIAN_POINT('Ctrl Pts',(-3.505683018611,-1.,-1.9730119116298));
#37370=CARTESIAN_POINT('Ctrl Pts',(-3.51056110478334,-1.,-1.97890693666316));
#37371=CARTESIAN_POINT('Ctrl Pts',(-3.51541198728362,-1.,-1.98483351061066));
#37372=CARTESIAN_POINT('Ctrl Pts',(-3.52023644289195,-1.,-1.99079153006143));
#37373=CARTESIAN_POINT('Ctrl Pts',(-3.52503542491745,-1.,-1.99678100339305));
#37374=CARTESIAN_POINT('Ctrl Pts',(-3.52980980250181,-1.,-2.00280191090341));
#37375=CARTESIAN_POINT('Ctrl Pts',(-3.53456004727321,-1.,-2.00885403604685));
#37376=CARTESIAN_POINT('Ctrl Pts',(-3.53928627453503,-1.,-2.0149369884727));
#37377=CARTESIAN_POINT('Ctrl Pts',(-3.54398838254011,-1.,-2.0210502798303));
#37378=CARTESIAN_POINT('Ctrl Pts',(-3.54866616282173,-1.,-2.02719338376144));
#37379=CARTESIAN_POINT('Ctrl Pts',(-3.55331941294018,-1.,-2.03336579658174));
#37380=CARTESIAN_POINT('Ctrl Pts',(-3.55794807265052,-1.,-2.03956711120099));
#37381=CARTESIAN_POINT('Ctrl Pts',(-3.5625522387181,-1.,-2.04579702159056));
#37382=CARTESIAN_POINT('Ctrl Pts',(-3.56713209978207,-1.,-2.0520552817309));
#37383=CARTESIAN_POINT('Ctrl Pts',(-3.57168789423507,-1.,-2.05834167687523));
#37384=CARTESIAN_POINT('Ctrl Pts',(-3.576219862243,-1.,-2.06465599229174));
#37385=CARTESIAN_POINT('Ctrl Pts',(-3.58072819250442,-1.,-2.07099797605747));
#37386=CARTESIAN_POINT('Ctrl Pts',(-3.58521300039299,-1.,-2.07736732842117));
#37387=CARTESIAN_POINT('Ctrl Pts',(-3.58967435355088,-1.,-2.08376373048756));
#37388=CARTESIAN_POINT('Ctrl Pts',(-3.59411228625588,-1.,-2.09018686331416));
#37389=CARTESIAN_POINT('Ctrl Pts',(-3.59852681775485,-1.,-2.09663642986631));
#37390=CARTESIAN_POINT('Ctrl Pts',(-3.60291797088734,-1.,-2.1031121772821));
#37391=CARTESIAN_POINT('Ctrl Pts',(-3.60728578532601,-1.,-2.10961391334462));
#37392=CARTESIAN_POINT('Ctrl Pts',(-3.61163030609447,-1.,-2.11614149815106));
#37393=CARTESIAN_POINT('Ctrl Pts',(-3.61508732216891,-1.,-2.12138417126355));
#37394=CARTESIAN_POINT('Ctrl Pts',(-3.61766963590482,-1.,-2.12532774376758));
#37395=CARTESIAN_POINT('Ctrl Pts',(-3.61938653649098,-1.,-2.12796193131368));
#37396=CARTESIAN_POINT('Ctrl Pts',(-3.62024382630768,-1.,-2.12928030988903));
#37397=CARTESIAN_POINT('',(-3.54075895182139,-1.,-2.25898783642071));
#37398=CARTESIAN_POINT('',(-3.62024382630768,-1.,-2.12928030988903));
#37399=CARTESIAN_POINT('',(-3.08655633322212,-1.,-2.1297112484669));
#37400=CARTESIAN_POINT('Ctrl Pts',(-3.54075895182139,-1.,-2.25898783642071));
#37401=CARTESIAN_POINT('Ctrl Pts',(-3.53919506647335,-1.,-2.2588225169468));
#37402=CARTESIAN_POINT('Ctrl Pts',(-3.53606853162228,-1.,-2.25848864343951));
#37403=CARTESIAN_POINT('Ctrl Pts',(-3.53138243688262,-1.,-2.25797812950104));
#37404=CARTESIAN_POINT('Ctrl Pts',(-3.52514172847711,-1.,-2.25727802940898));
#37405=CARTESIAN_POINT('Ctrl Pts',(-3.51735323667612,-1.,-2.25637049455044));
#37406=CARTESIAN_POINT('Ctrl Pts',(-3.50957720117341,-1.,-2.25543046979799));
#37407=CARTESIAN_POINT('Ctrl Pts',(-3.50181372617971,-1.,-2.25445785151868));
#37408=CARTESIAN_POINT('Ctrl Pts',(-3.49406296494791,-1.,-2.2534525170976));
#37409=CARTESIAN_POINT('Ctrl Pts',(-3.48632513240961,-1.,-2.25241433138695));
#37410=CARTESIAN_POINT('Ctrl Pts',(-3.47860048448691,-1.,-2.25134314238687));
#37411=CARTESIAN_POINT('Ctrl Pts',(-3.47088928979888,-1.,-2.25023877475942));
#37412=CARTESIAN_POINT('Ctrl Pts',(-3.46319180177573,-1.,-2.2491010234604));
#37413=CARTESIAN_POINT('Ctrl Pts',(-3.45550823512049,-1.,-2.2479296496077));
#37414=CARTESIAN_POINT('Ctrl Pts',(-3.44783872863151,-1.,-2.2467243706995));
#37415=CARTESIAN_POINT('Ctrl Pts',(-3.4401833646032,-1.,-2.24548487526022));
#37416=CARTESIAN_POINT('Ctrl Pts',(-3.43254222614803,-1.,-2.24421085338727));
#37417=CARTESIAN_POINT('Ctrl Pts',(-3.42491544683008,-1.,-2.24290202531101));
#37418=CARTESIAN_POINT('Ctrl Pts',(-3.41730325539172,-1.,-2.24155816587844));
#37419=CARTESIAN_POINT('Ctrl Pts',(-3.40970604190328,-1.,-2.24017914395289));
#37420=CARTESIAN_POINT('Ctrl Pts',(-3.40212434705647,-1.,-2.2387649112415));
#37421=CARTESIAN_POINT('Ctrl Pts',(-3.39455873448189,-1.,-2.23731541452791));
#37422=CARTESIAN_POINT('Ctrl Pts',(-3.38700968549563,-1.,-2.23583052276308));
#37423=CARTESIAN_POINT('Ctrl Pts',(-3.37947749555632,-1.,-2.23430995599561));
#37424=CARTESIAN_POINT('Ctrl Pts',(-3.37196214349304,-1.,-2.23275319569221));
#37425=CARTESIAN_POINT('Ctrl Pts',(-3.36446325227848,-1.,-2.23115945849739));
#37426=CARTESIAN_POINT('Ctrl Pts',(-3.35698038165483,-1.,-2.22952789880982));
#37427=CARTESIAN_POINT('Ctrl Pts',(-3.34951327111096,-1.,-2.22785777756576));
#37428=CARTESIAN_POINT('Ctrl Pts',(-3.34206209449375,-1.,-2.22614863918047));
#37429=CARTESIAN_POINT('Ctrl Pts',(-3.33462772849598,-1.,-2.22440049878511));
#37430=CARTESIAN_POINT('Ctrl Pts',(-3.3272119632604,-1.,-2.22261398879635));
#37431=CARTESIAN_POINT('Ctrl Pts',(-3.31981686778022,-1.,-2.22078990842776));
#37432=CARTESIAN_POINT('Ctrl Pts',(-3.31244421655666,-1.,-2.21892881679086));
#37433=CARTESIAN_POINT('Ctrl Pts',(-3.30509487819569,-1.,-2.21703059947836));
#37434=CARTESIAN_POINT('Ctrl Pts',(-3.29776825193159,-1.,-2.21509406923368));
#37435=CARTESIAN_POINT('Ctrl Pts',(-3.29046159238343,-1.,-2.21311648827391));
#37436=CARTESIAN_POINT('Ctrl Pts',(-3.28317133333131,-1.,-2.21109449750641));
#37437=CARTESIAN_POINT('Ctrl Pts',(-3.2758944800554,-1.,-2.2090250941743));
#37438=CARTESIAN_POINT('Ctrl Pts',(-3.26863006136782,-1.,-2.20690665217743));
#37439=CARTESIAN_POINT('Ctrl Pts',(-3.26138036637705,-1.,-2.20473979048678));
#37440=CARTESIAN_POINT('Ctrl Pts',(-3.25415277957775,-1.,-2.20252866491545));
#37441=CARTESIAN_POINT('Ctrl Pts',(-3.24695715874338,-1.,-2.20027910880981));
#37442=CARTESIAN_POINT('Ctrl Pts',(-3.23980245361308,-1.,-2.19799623693253));
#37443=CARTESIAN_POINT('Ctrl Pts',(-3.23269332296933,-1.,-2.19568204933168));
#37444=CARTESIAN_POINT('Ctrl Pts',(-3.22562734221646,-1.,-2.19333345123538));
#37445=CARTESIAN_POINT('Ctrl Pts',(-3.21859043114095,-1.,-2.19093901948667));
#37446=CARTESIAN_POINT('Ctrl Pts',(-3.21156188355769,-1.,-2.18848253363901));
#37447=CARTESIAN_POINT('Ctrl Pts',(-3.20452259717976,-1.,-2.18594876115934));
#37448=CARTESIAN_POINT('Ctrl Pts',(-3.19746293740411,-1.,-2.18332898656602));
#37449=CARTESIAN_POINT('Ctrl Pts',(-3.19038924261573,-1.,-2.18062558031778));
#37450=CARTESIAN_POINT('Ctrl Pts',(-3.18333474627807,-1.,-2.17785968847142));
#37451=CARTESIAN_POINT('Ctrl Pts',(-3.17635032802523,-1.,-2.17506466903694));
#37452=CARTESIAN_POINT('Ctrl Pts',(-3.16948480019497,-1.,-2.17227212063817));
#37453=CARTESIAN_POINT('Ctrl Pts',(-3.16276685102972,-1.,-2.16949910801219));
#37454=CARTESIAN_POINT('Ctrl Pts',(-3.15618975593656,-1.,-2.1667372844769));
#37455=CARTESIAN_POINT('Ctrl Pts',(-3.14968624389054,-1.,-2.16393520288072));
#37456=CARTESIAN_POINT('Ctrl Pts',(-3.14314440427022,-1.,-2.16100905914435));
#37457=CARTESIAN_POINT('Ctrl Pts',(-3.13645356563038,-1.,-2.15787423530676));
#37458=CARTESIAN_POINT('Ctrl Pts',(-3.12954386795646,-1.,-2.1544724138292));
#37459=CARTESIAN_POINT('Ctrl Pts',(-3.12242318151938,-1.,-2.15079698090585));
#37460=CARTESIAN_POINT('Ctrl Pts',(-3.11522827016855,-1.,-2.14692798457532));
#37461=CARTESIAN_POINT('Ctrl Pts',(-3.10821808668859,-1.,-2.14302815601973));
#37462=CARTESIAN_POINT('Ctrl Pts',(-3.10171267391049,-1.,-2.13930228863751));
#37463=CARTESIAN_POINT('Ctrl Pts',(-3.0960450242104,-1.,-2.13596538661048));
#37464=CARTESIAN_POINT('Ctrl Pts',(-3.09151235281963,-1.,-2.13321032560893));
#37465=CARTESIAN_POINT('Ctrl Pts',(-3.08855597949761,-1.,-2.13132142793017));
#37466=CARTESIAN_POINT('Ctrl Pts',(-3.08717896996099,-1.,-2.13034980480424));
#37467=CARTESIAN_POINT('Ctrl Pts',(-3.08668447250322,-1.,-2.12991938762374));
#37468=CARTESIAN_POINT('Ctrl Pts',(-3.08657131089497,-1.,-2.1297578506149));
#37469=CARTESIAN_POINT('Ctrl Pts',(-3.08655633322212,-1.,-2.1297112484669));
#37470=CARTESIAN_POINT('',(-2.97927412174388,-1.,-2.27737254473378));
#37471=CARTESIAN_POINT('Origin',(0.,-1.,0.));
#37472=CARTESIAN_POINT('',(-3.24257979115744,-1.,-2.66939624221984));
#37473=CARTESIAN_POINT('Ctrl Pts',(-2.97927412174388,-1.,-2.27737254473378));
#37474=CARTESIAN_POINT('Ctrl Pts',(-2.97932307137589,-1.,-2.27737238849212));
#37475=CARTESIAN_POINT('Ctrl Pts',(-2.97951167106106,-1.,-2.27743009389704));
#37476=CARTESIAN_POINT('Ctrl Pts',(-2.98007383024333,-1.,-2.27776738270369));
#37477=CARTESIAN_POINT('Ctrl Pts',(-2.98142341809623,-1.,-2.27877674853833));
#37478=CARTESIAN_POINT('Ctrl Pts',(-2.98413343613858,-1.,-2.28100472516582));
#37479=CARTESIAN_POINT('Ctrl Pts',(-2.98815432734929,-1.,-2.28446419116036));
#37480=CARTESIAN_POINT('Ctrl Pts',(-2.9930793098434,-1.,-2.28882328690601));
#37481=CARTESIAN_POINT('Ctrl Pts',(-2.99863310340004,-1.,-2.29385894577999));
#37482=CARTESIAN_POINT('Ctrl Pts',(-3.00450832658822,-1.,-2.29932091315939));
#37483=CARTESIAN_POINT('Ctrl Pts',(-3.01041131063882,-1.,-2.30496809486528));
#37484=CARTESIAN_POINT('Ctrl Pts',(-3.01610726819019,-1.,-2.31060449886577));
#37485=CARTESIAN_POINT('Ctrl Pts',(-3.02147780668029,-1.,-2.31612479121528));
#37486=CARTESIAN_POINT('Ctrl Pts',(-3.02652678416478,-1.,-2.32151944306299));
#37487=CARTESIAN_POINT('Ctrl Pts',(-3.03133125185047,-1.,-2.32683687412027));
#37488=CARTESIAN_POINT('Ctrl Pts',(-3.03600588555765,-1.,-2.33215619079807));
#37489=CARTESIAN_POINT('Ctrl Pts',(-3.04066496998569,-1.,-2.33755792953726));
#37490=CARTESIAN_POINT('Ctrl Pts',(-3.04537822217311,-1.,-2.3430901708402));
#37491=CARTESIAN_POINT('Ctrl Pts',(-3.05015565829976,-1.,-2.34875673090816));
#37492=CARTESIAN_POINT('Ctrl Pts',(-3.05497218368188,-1.,-2.35453559889506));
#37493=CARTESIAN_POINT('Ctrl Pts',(-3.05978266240056,-1.,-2.36039011602084));
#37494=CARTESIAN_POINT('Ctrl Pts',(-3.06453964643152,-1.,-2.36628220107001));
#37495=CARTESIAN_POINT('Ctrl Pts',(-3.06921275497472,-1.,-2.37218678163157));
#37496=CARTESIAN_POINT('Ctrl Pts',(-3.07379777492133,-1.,-2.37809856205524));
#37497=CARTESIAN_POINT('Ctrl Pts',(-3.07830597244301,-1.,-2.38402401216107));
#37498=CARTESIAN_POINT('Ctrl Pts',(-3.08275773747083,-1.,-2.38997659219192));
#37499=CARTESIAN_POINT('Ctrl Pts',(-3.08717489512919,-1.,-2.39597098250635));
#37500=CARTESIAN_POINT('Ctrl Pts',(-3.09157266051115,-1.,-2.40201704423352));
#37501=CARTESIAN_POINT('Ctrl Pts',(-3.09595472616093,-1.,-2.40811612696382));
#37502=CARTESIAN_POINT('Ctrl Pts',(-3.10031775027683,-1.,-2.41426441798067));
#37503=CARTESIAN_POINT('Ctrl Pts',(-3.10465410280902,-1.,-2.42045498612494));
#37504=CARTESIAN_POINT('Ctrl Pts',(-3.10895518969592,-1.,-2.42668025870013));
#37505=CARTESIAN_POINT('Ctrl Pts',(-3.11321477659012,-1.,-2.4329344968514));
#37506=CARTESIAN_POINT('Ctrl Pts',(-3.11743156744182,-1.,-2.43921571477975));
#37507=CARTESIAN_POINT('Ctrl Pts',(-3.12160740887768,-1.,-2.44552433364716));
#37508=CARTESIAN_POINT('Ctrl Pts',(-3.12574608210849,-1.,-2.45186227369848));
#37509=CARTESIAN_POINT('Ctrl Pts',(-3.12985188384372,-1.,-2.45823188859366));
#37510=CARTESIAN_POINT('Ctrl Pts',(-3.13392826623902,-1.,-2.4646349433237));
#37511=CARTESIAN_POINT('Ctrl Pts',(-3.13797654408931,-1.,-2.47107164236827));
#37512=CARTESIAN_POINT('Ctrl Pts',(-3.14199655778845,-1.,-2.47754112428027));
#37513=CARTESIAN_POINT('Ctrl Pts',(-3.1459872272388,-1.,-2.48404187418376));
#37514=CARTESIAN_POINT('Ctrl Pts',(-3.14994715298903,-1.,-2.49057217131985));
#37515=CARTESIAN_POINT('Ctrl Pts',(-3.15387518039064,-1.,-2.49713050858911));
#37516=CARTESIAN_POINT('Ctrl Pts',(-3.15777102413998,-1.,-2.50371605688287));
#37517=CARTESIAN_POINT('Ctrl Pts',(-3.16163506380211,-1.,-2.51032851007939));
#37518=CARTESIAN_POINT('Ctrl Pts',(-3.16546808277069,-1.,-2.51696788755615));
#37519=CARTESIAN_POINT('Ctrl Pts',(-3.16927102130751,-1.,-2.523634346718));
#37520=CARTESIAN_POINT('Ctrl Pts',(-3.17304474093574,-1.,-2.5303280040691));
#37521=CARTESIAN_POINT('Ctrl Pts',(-3.17678974135225,-1.,-2.53704871950871));
#37522=CARTESIAN_POINT('Ctrl Pts',(-3.18050619750515,-1.,-2.54379612552948));
#37523=CARTESIAN_POINT('Ctrl Pts',(-3.18419408529482,-1.,-2.55056972387638));
#37524=CARTESIAN_POINT('Ctrl Pts',(-3.1878532811617,-1.,-2.55736896206016));
#37525=CARTESIAN_POINT('Ctrl Pts',(-3.19148366395201,-1.,-2.56419331092909));
#37526=CARTESIAN_POINT('Ctrl Pts',(-3.19508523784548,-1.,-2.57104235898053));
#37527=CARTESIAN_POINT('Ctrl Pts',(-3.19865814628955,-1.,-2.577915819091));
#37528=CARTESIAN_POINT('Ctrl Pts',(-3.20220261408685,-1.,-2.58481347777953));
#37529=CARTESIAN_POINT('Ctrl Pts',(-3.20571891028879,-1.,-2.59173516023605));
#37530=CARTESIAN_POINT('Ctrl Pts',(-3.2092073056959,-1.,-2.59868069194267));
#37531=CARTESIAN_POINT('Ctrl Pts',(-3.21266802609297,-1.,-2.60564985359699));
#37532=CARTESIAN_POINT('Ctrl Pts',(-3.21610123232465,-1.,-2.61264236718662));
#37533=CARTESIAN_POINT('Ctrl Pts',(-3.21950704108654,-1.,-2.61965792832396));
#37534=CARTESIAN_POINT('Ctrl Pts',(-3.222885536128,-1.,-2.62669622735548));
#37535=CARTESIAN_POINT('Ctrl Pts',(-3.22623678292539,-1.,-2.63375697391438));
#37536=CARTESIAN_POINT('Ctrl Pts',(-3.2295608435934,-1.,-2.64083992182478));
#37537=CARTESIAN_POINT('Ctrl Pts',(-3.23285778738558,-1.,-2.64794488744246));
#37538=CARTESIAN_POINT('Ctrl Pts',(-3.23612768065687,-1.,-2.6550717396303));
#37539=CARTESIAN_POINT('Ctrl Pts',(-3.23872200036311,-1.,-2.6607906631973));
#37540=CARTESIAN_POINT('Ctrl Pts',(-3.24065561087681,-1.,-2.66508964664767));
#37541=CARTESIAN_POINT('Ctrl Pts',(-3.24193929584813,-1.,-2.66795998539861));
#37542=CARTESIAN_POINT('Ctrl Pts',(-3.24257979115744,-1.,-2.66939624221984));
#37543=CARTESIAN_POINT('',(-3.14378277984898,-1.,-2.78507268004356));
#37544=CARTESIAN_POINT('',(-3.24257979115744,-1.,-2.66939624221984));
#37545=CARTESIAN_POINT('',(-2.71539546306948,-1.,-2.58633475774921));
#37546=CARTESIAN_POINT('Ctrl Pts',(-3.14378277984898,-1.,-2.78507268004356));
#37547=CARTESIAN_POINT('Ctrl Pts',(-3.14226401018816,-1.,-2.7846647503589));
#37548=CARTESIAN_POINT('Ctrl Pts',(-3.13922819749279,-1.,-2.78384588958165));
#37549=CARTESIAN_POINT('Ctrl Pts',(-3.13467965833037,-1.,-2.78260859419319));
#37550=CARTESIAN_POINT('Ctrl Pts',(-3.12862530318457,-1.,-2.78094085161413));
#37551=CARTESIAN_POINT('Ctrl Pts',(-3.12107467037201,-1.,-2.77882610146731));
#37552=CARTESIAN_POINT('Ctrl Pts',(-3.11354142303921,-1.,-2.77668121002545));
#37553=CARTESIAN_POINT('Ctrl Pts',(-3.10602568032564,-1.,-2.77450609123362));
#37554=CARTESIAN_POINT('Ctrl Pts',(-3.0985276127786,-1.,-2.77230064796057));
#37555=CARTESIAN_POINT('Ctrl Pts',(-3.09104745382531,-1.,-2.7700647803451));
#37556=CARTESIAN_POINT('Ctrl Pts',(-3.08358548001504,-1.,-2.76779837829373));
#37557=CARTESIAN_POINT('Ctrl Pts',(-3.07614198408862,-1.,-2.76550131064852));
#37558=CARTESIAN_POINT('Ctrl Pts',(-3.0687172484321,-1.,-2.76317341453493));
#37559=CARTESIAN_POINT('Ctrl Pts',(-3.06131152247454,-1.,-2.76081448759882));
#37560=CARTESIAN_POINT('Ctrl Pts',(-3.05392498749847,-1.,-2.75842427252931));
#37561=CARTESIAN_POINT('Ctrl Pts',(-3.04655777351067,-1.,-2.75600247455925));
#37562=CARTESIAN_POINT('Ctrl Pts',(-3.03921001107977,-1.,-2.75354880060314));
#37563=CARTESIAN_POINT('Ctrl Pts',(-3.03188187589107,-1.,-2.75106299522979));
#37564=CARTESIAN_POINT('Ctrl Pts',(-3.02457362909245,-1.,-2.7485448718414));
#37565=CARTESIAN_POINT('Ctrl Pts',(-3.01728567646611,-1.,-2.74599436193625));
#37566=CARTESIAN_POINT('Ctrl Pts',(-3.01001855960162,-1.,-2.74341150239887));
#37567=CARTESIAN_POINT('Ctrl Pts',(-3.00277284351521,-1.,-2.74079632883931));
#37568=CARTESIAN_POINT('Ctrl Pts',(-2.99554902409778,-1.,-2.73814878711641));
#37569=CARTESIAN_POINT('Ctrl Pts',(-2.9883474369644,-1.,-2.73546864694536));
#37570=CARTESIAN_POINT('Ctrl Pts',(-2.98116814232129,-1.,-2.73275539286497));
#37571=CARTESIAN_POINT('Ctrl Pts',(-2.97401089032677,-1.,-2.73000819218414));
#37572=CARTESIAN_POINT('Ctrl Pts',(-2.96687537842451,-1.,-2.72722614084076));
#37573=CARTESIAN_POINT('Ctrl Pts',(-2.95976146492576,-1.,-2.72440846811729));
#37574=CARTESIAN_POINT('Ctrl Pts',(-2.95266939280621,-1.,-2.72155475123364));
#37575=CARTESIAN_POINT('Ctrl Pts',(-2.94560002559806,-1.,-2.71866514227965));
#37576=CARTESIAN_POINT('Ctrl Pts',(-2.93855503247266,-1.,-2.7157405459259));
#37577=CARTESIAN_POINT('Ctrl Pts',(-2.93153633192595,-1.,-2.71278207520817));
#37578=CARTESIAN_POINT('Ctrl Pts',(-2.92454558914778,-1.,-2.70979055994754));
#37579=CARTESIAN_POINT('Ctrl Pts',(-2.91758367994737,-1.,-2.70676602302518));
#37580=CARTESIAN_POINT('Ctrl Pts',(-2.91065019668329,-1.,-2.70370719782113));
#37581=CARTESIAN_POINT('Ctrl Pts',(-2.90374285605838,-1.,-2.70061095078692));
#37582=CARTESIAN_POINT('Ctrl Pts',(-2.89685866123671,-1.,-2.69747340630625));
#37583=CARTESIAN_POINT('Ctrl Pts',(-2.88999512410309,-1.,-2.69429113011374));
#37584=CARTESIAN_POINT('Ctrl Pts',(-2.88315153980466,-1.,-2.69106236420198));
#37585=CARTESIAN_POINT('Ctrl Pts',(-2.8763300724388,-1.,-2.68778807801686));
#37586=CARTESIAN_POINT('Ctrl Pts',(-2.86953736547238,-1.,-2.68447353139599));
#37587=CARTESIAN_POINT('Ctrl Pts',(-2.86278224277689,-1.,-2.68112602796308));
#37588=CARTESIAN_POINT('Ctrl Pts',(-2.85607274378018,-1.,-2.67775201955724));
#37589=CARTESIAN_POINT('Ctrl Pts',(-2.84941315703092,-1.,-2.67435421039677));
#37590=CARTESIAN_POINT('Ctrl Pts',(-2.84280157191323,-1.,-2.67092916452125));
#37591=CARTESIAN_POINT('Ctrl Pts',(-2.83622586853982,-1.,-2.66746339678107));
#37592=CARTESIAN_POINT('Ctrl Pts',(-2.82966813308998,-1.,-2.6639376472693));
#37593=CARTESIAN_POINT('Ctrl Pts',(-2.82311188135078,-1.,-2.66033388273461));
#37594=CARTESIAN_POINT('Ctrl Pts',(-2.81654896073883,-1.,-2.65664198781344));
#37595=CARTESIAN_POINT('Ctrl Pts',(-2.80998526078165,-1.,-2.65286529532208));
#37596=CARTESIAN_POINT('Ctrl Pts',(-2.80345029781152,-1.,-2.64902988983337));
#37597=CARTESIAN_POINT('Ctrl Pts',(-2.79698910670736,-1.,-2.64517667799319));
#37598=CARTESIAN_POINT('Ctrl Pts',(-2.79064495573224,-1.,-2.64134450532584));
#37599=CARTESIAN_POINT('Ctrl Pts',(-2.78444351041571,-1.,-2.637554714303));
#37600=CARTESIAN_POINT('Ctrl Pts',(-2.77837943466449,-1.,-2.63379800904599));
#37601=CARTESIAN_POINT('Ctrl Pts',(-2.77239433377921,-1.,-2.63001305229625));
#37602=CARTESIAN_POINT('Ctrl Pts',(-2.76639078479021,-1.,-2.62609956506355));
#37603=CARTESIAN_POINT('Ctrl Pts',(-2.76027271596686,-1.,-2.62195665834605));
#37604=CARTESIAN_POINT('Ctrl Pts',(-2.7539802502603,-1.,-2.61751580407667));
#37605=CARTESIAN_POINT('Ctrl Pts',(-2.74752219567252,-1.,-2.61277170105813));
#37606=CARTESIAN_POINT('Ctrl Pts',(-2.7410211099909,-1.,-2.60782480638448));
#37607=CARTESIAN_POINT('Ctrl Pts',(-2.73470730109615,-1.,-2.60287635688728));
#37608=CARTESIAN_POINT('Ctrl Pts',(-2.7288648348152,-1.,-2.59817869034746));
#37609=CARTESIAN_POINT('Ctrl Pts',(-2.72378896977134,-1.,-2.59399625537278));
#37610=CARTESIAN_POINT('Ctrl Pts',(-2.71974308958086,-1.,-2.59056604771971));
#37611=CARTESIAN_POINT('Ctrl Pts',(-2.71711860281815,-1.,-2.58823792682672));
#37612=CARTESIAN_POINT('Ctrl Pts',(-2.71591054189786,-1.,-2.58706285424358));
#37613=CARTESIAN_POINT('Ctrl Pts',(-2.71548946460575,-1.,-2.58656037976753));
#37614=CARTESIAN_POINT('Ctrl Pts',(-2.71540296616024,-1.,-2.58638312917167));
#37615=CARTESIAN_POINT('Ctrl Pts',(-2.71539546306948,-1.,-2.58633475774921));
#37616=CARTESIAN_POINT('',(-2.58633475775051,-1.,-2.71539546306824));
#37617=CARTESIAN_POINT('Origin',(0.,-1.,0.));
#37618=CARTESIAN_POINT('',(-2.78507268004356,-1.,-3.14378277984898));
#37619=CARTESIAN_POINT('Ctrl Pts',(-2.58633475775051,-1.,-2.71539546306824));
#37620=CARTESIAN_POINT('Ctrl Pts',(-2.58638312917291,-1.,-2.71540296615967));
#37621=CARTESIAN_POINT('Ctrl Pts',(-2.58656037976884,-1.,-2.71548946460616));
#37622=CARTESIAN_POINT('Ctrl Pts',(-2.58706285424469,-1.,-2.71591054189884));
#37623=CARTESIAN_POINT('Ctrl Pts',(-2.58823792682724,-1.,-2.7171186028189));
#37624=CARTESIAN_POINT('Ctrl Pts',(-2.59056604771863,-1.,-2.7197430895797));
#37625=CARTESIAN_POINT('Ctrl Pts',(-2.59399625537407,-1.,-2.72378896977273));
#37626=CARTESIAN_POINT('Ctrl Pts',(-2.5981786903501,-1.,-2.72886483481804));
#37627=CARTESIAN_POINT('Ctrl Pts',(-2.60287635689,-1.,-2.73470730109906));
#37628=CARTESIAN_POINT('Ctrl Pts',(-2.60782480638629,-1.,-2.74102110999284));
#37629=CARTESIAN_POINT('Ctrl Pts',(-2.61277170105864,-1.,-2.74752219567307));
#37630=CARTESIAN_POINT('Ctrl Pts',(-2.61751580407608,-1.,-2.75398025025967));
#37631=CARTESIAN_POINT('Ctrl Pts',(-2.62195665834491,-1.,-2.76027271596564));
#37632=CARTESIAN_POINT('Ctrl Pts',(-2.6260995650624,-1.,-2.76639078478898));
#37633=CARTESIAN_POINT('Ctrl Pts',(-2.63001305229548,-1.,-2.77239433377839));
#37634=CARTESIAN_POINT('Ctrl Pts',(-2.63379800904575,-1.,-2.77837943466423));
#37635=CARTESIAN_POINT('Ctrl Pts',(-2.63755471430322,-1.,-2.78444351041594));
#37636=CARTESIAN_POINT('Ctrl Pts',(-2.64134450532632,-1.,-2.79064495573275));
#37637=CARTESIAN_POINT('Ctrl Pts',(-2.6451766779937,-1.,-2.7969891067079));
#37638=CARTESIAN_POINT('Ctrl Pts',(-2.64902988983373,-1.,-2.80345029781191));
#37639=CARTESIAN_POINT('Ctrl Pts',(-2.65286529532221,-1.,-2.80998526078179));
#37640=CARTESIAN_POINT('Ctrl Pts',(-2.65664198781335,-1.,-2.81654896073874));
#37641=CARTESIAN_POINT('Ctrl Pts',(-2.66033388273437,-1.,-2.82311188135053));
#37642=CARTESIAN_POINT('Ctrl Pts',(-2.66393764726902,-1.,-2.82966813308969));
#37643=CARTESIAN_POINT('Ctrl Pts',(-2.66746339678085,-1.,-2.8362258685396));
#37644=CARTESIAN_POINT('Ctrl Pts',(-2.67092916452117,-1.,-2.84280157191314));
#37645=CARTESIAN_POINT('Ctrl Pts',(-2.67435421039682,-1.,-2.84941315703096));
#37646=CARTESIAN_POINT('Ctrl Pts',(-2.67775201955736,-1.,-2.85607274378031));
#37647=CARTESIAN_POINT('Ctrl Pts',(-2.68112602796323,-1.,-2.86278224277705));
#37648=CARTESIAN_POINT('Ctrl Pts',(-2.68447353139611,-1.,-2.8695373654725));
#37649=CARTESIAN_POINT('Ctrl Pts',(-2.68778807801691,-1.,-2.87633007243885));
#37650=CARTESIAN_POINT('Ctrl Pts',(-2.69106236420197,-1.,-2.88315153980464));
#37651=CARTESIAN_POINT('Ctrl Pts',(-2.69429113011369,-1.,-2.88999512410304));
#37652=CARTESIAN_POINT('Ctrl Pts',(-2.69747340630621,-1.,-2.89685866123668));
#37653=CARTESIAN_POINT('Ctrl Pts',(-2.70061095078692,-1.,-2.90374285605839));
#37654=CARTESIAN_POINT('Ctrl Pts',(-2.70370719782114,-1.,-2.91065019668331));
#37655=CARTESIAN_POINT('Ctrl Pts',(-2.70676602302518,-1.,-2.91758367994738));
#37656=CARTESIAN_POINT('Ctrl Pts',(-2.70979055994751,-1.,-2.92454558914774));
#37657=CARTESIAN_POINT('Ctrl Pts',(-2.71278207520807,-1.,-2.93153633192583));
#37658=CARTESIAN_POINT('Ctrl Pts',(-2.71574054592575,-1.,-2.93855503247248));
#37659=CARTESIAN_POINT('Ctrl Pts',(-2.71866514227952,-1.,-2.94560002559789));
#37660=CARTESIAN_POINT('Ctrl Pts',(-2.72155475123361,-1.,-2.95266939280617));
#37661=CARTESIAN_POINT('Ctrl Pts',(-2.72440846811745,-1.,-2.95976146492595));
#37662=CARTESIAN_POINT('Ctrl Pts',(-2.72722614084112,-1.,-2.96687537842492));
#37663=CARTESIAN_POINT('Ctrl Pts',(-2.7300081921846,-1.,-2.97401089032729));
#37664=CARTESIAN_POINT('Ctrl Pts',(-2.73275539286537,-1.,-2.98116814232175));
#37665=CARTESIAN_POINT('Ctrl Pts',(-2.73546864694548,-1.,-2.98834743696455));
#37666=CARTESIAN_POINT('Ctrl Pts',(-2.73814878711609,-1.,-2.99554902409741));
#37667=CARTESIAN_POINT('Ctrl Pts',(-2.74079632883852,-1.,-3.00277284351431));
#37668=CARTESIAN_POINT('Ctrl Pts',(-2.7434115023978,-1.,-3.01001855960041));
#37669=CARTESIAN_POINT('Ctrl Pts',(-2.74599436193528,-1.,-3.01728567646502));
#37670=CARTESIAN_POINT('Ctrl Pts',(-2.74854487184099,-1.,-3.02457362909199));
#37671=CARTESIAN_POINT('Ctrl Pts',(-2.75106299523032,-1.,-3.03188187589168));
#37672=CARTESIAN_POINT('Ctrl Pts',(-2.75354880060473,-1.,-3.03921001108158));
#37673=CARTESIAN_POINT('Ctrl Pts',(-2.7560024745616,-1.,-3.04655777351333));
#37674=CARTESIAN_POINT('Ctrl Pts',(-2.75842427253164,-1.,-3.05392498750112));
#37675=CARTESIAN_POINT('Ctrl Pts',(-2.76081448760011,-1.,-3.06131152247599));
#37676=CARTESIAN_POINT('Ctrl Pts',(-2.76317341453415,-1.,-3.06871724843121));
#37677=CARTESIAN_POINT('Ctrl Pts',(-2.76550131064522,-1.,-3.07614198408488));
#37678=CARTESIAN_POINT('Ctrl Pts',(-2.76779837828843,-1.,-3.08358548000904));
#37679=CARTESIAN_POINT('Ctrl Pts',(-2.77006478033937,-1.,-3.09104745381882));
#37680=CARTESIAN_POINT('Ctrl Pts',(-2.77230064795679,-1.,-3.09852761277432));
#37681=CARTESIAN_POINT('Ctrl Pts',(-2.7745060912343,-1.,-3.10602568032641));
#37682=CARTESIAN_POINT('Ctrl Pts',(-2.77668121003225,-1.,-3.11354142304692));
#37683=CARTESIAN_POINT('Ctrl Pts',(-2.77882610147986,-1.,-3.12107467038623));
#37684=CARTESIAN_POINT('Ctrl Pts',(-2.78094085162947,-1.,-3.12862530320194));
#37685=CARTESIAN_POINT('Ctrl Pts',(-2.78260859420629,-1.,-3.1346796583452));
#37686=CARTESIAN_POINT('Ctrl Pts',(-2.78384588958965,-1.,-3.13922819750185));
#37687=CARTESIAN_POINT('Ctrl Pts',(-2.78466475036183,-1.,-3.14226401019149));
#37688=CARTESIAN_POINT('Ctrl Pts',(-2.78507268004356,-1.,-3.14378277984898));
#37689=CARTESIAN_POINT('',(-2.66939624221984,-1.,-3.24257979115744));
#37690=CARTESIAN_POINT('',(-2.78507268004356,-1.,-3.14378277984898));
#37691=CARTESIAN_POINT('',(-2.27737254473521,-1.,-2.97927412174279));
#37692=CARTESIAN_POINT('Ctrl Pts',(-2.66939624221984,-1.,-3.24257979115744));
#37693=CARTESIAN_POINT('Ctrl Pts',(-2.66795998539579,-1.,-3.24193929584471));
#37694=CARTESIAN_POINT('Ctrl Pts',(-2.66508964663997,-1.,-3.24065561086749));
#37695=CARTESIAN_POINT('Ctrl Pts',(-2.6607906631847,-1.,-3.23872200034785));
#37696=CARTESIAN_POINT('Ctrl Pts',(-2.65507173961555,-1.,-3.236127680639));
#37697=CARTESIAN_POINT('Ctrl Pts',(-2.64794488743038,-1.,-3.23285778737096));
#37698=CARTESIAN_POINT('Ctrl Pts',(-2.64083992181823,-1.,-3.22956084358547));
#37699=CARTESIAN_POINT('Ctrl Pts',(-2.63375697391372,-1.,-3.2262367829246));
#37700=CARTESIAN_POINT('Ctrl Pts',(-2.62669622735912,-1.,-3.2228855361324));
#37701=CARTESIAN_POINT('Ctrl Pts',(-2.61965792832947,-1.,-3.21950704109321));
#37702=CARTESIAN_POINT('Ctrl Pts',(-2.61264236719171,-1.,-3.21610123233082));
#37703=CARTESIAN_POINT('Ctrl Pts',(-2.60564985360017,-1.,-3.21266802609682));
#37704=CARTESIAN_POINT('Ctrl Pts',(-2.59868069194342,-1.,-3.20920730569681));
#37705=CARTESIAN_POINT('Ctrl Pts',(-2.59173516023481,-1.,-3.2057189102873));
#37706=CARTESIAN_POINT('Ctrl Pts',(-2.58481347777729,-1.,-3.20220261408414));
#37707=CARTESIAN_POINT('Ctrl Pts',(-2.57791581908875,-1.,-3.19865814628682));
#37708=CARTESIAN_POINT('Ctrl Pts',(-2.57104235897899,-1.,-3.19508523784363));
#37709=CARTESIAN_POINT('Ctrl Pts',(-2.56419331092858,-1.,-3.19148366395139));
#37710=CARTESIAN_POINT('Ctrl Pts',(-2.55736896206056,-1.,-3.18785328116218));
#37711=CARTESIAN_POINT('Ctrl Pts',(-2.55056972387731,-1.,-3.18419408529594));
#37712=CARTESIAN_POINT('Ctrl Pts',(-2.54379612553051,-1.,-3.1805061975064));
#37713=CARTESIAN_POINT('Ctrl Pts',(-2.53704871950948,-1.,-3.17678974135318));
#37714=CARTESIAN_POINT('Ctrl Pts',(-2.53032800406941,-1.,-3.17304474093612));
#37715=CARTESIAN_POINT('Ctrl Pts',(-2.52363434671788,-1.,-3.16927102130736));
#37716=CARTESIAN_POINT('Ctrl Pts',(-2.51696788755577,-1.,-3.16546808277023));
#37717=CARTESIAN_POINT('Ctrl Pts',(-2.51032851007894,-1.,-3.16163506380157));
#37718=CARTESIAN_POINT('Ctrl Pts',(-2.50371605688252,-1.,-3.15777102413957));
#37719=CARTESIAN_POINT('Ctrl Pts',(-2.49713050858896,-1.,-3.15387518039046));
#37720=CARTESIAN_POINT('Ctrl Pts',(-2.49057217131988,-1.,-3.14994715298907));
#37721=CARTESIAN_POINT('Ctrl Pts',(-2.4840418741839,-1.,-3.14598722723896));
#37722=CARTESIAN_POINT('Ctrl Pts',(-2.47754112428043,-1.,-3.14199655778863));
#37723=CARTESIAN_POINT('Ctrl Pts',(-2.47107164236838,-1.,-3.13797654408943));
#37724=CARTESIAN_POINT('Ctrl Pts',(-2.46463494332374,-1.,-3.13392826623906));
#37725=CARTESIAN_POINT('Ctrl Pts',(-2.45823188859366,-1.,-3.12985188384371));
#37726=CARTESIAN_POINT('Ctrl Pts',(-2.45186227369846,-1.,-3.12574608210847));
#37727=CARTESIAN_POINT('Ctrl Pts',(-2.44552433364715,-1.,-3.12160740887768));
#37728=CARTESIAN_POINT('Ctrl Pts',(-2.43921571477977,-1.,-3.11743156744186));
#37729=CARTESIAN_POINT('Ctrl Pts',(-2.43293449685144,-1.,-3.11321477659018));
#37730=CARTESIAN_POINT('Ctrl Pts',(-2.42668025870015,-1.,-3.10895518969595));
#37731=CARTESIAN_POINT('Ctrl Pts',(-2.42045498612489,-1.,-3.10465410280896));
#37732=CARTESIAN_POINT('Ctrl Pts',(-2.41426441798057,-1.,-3.1003177502767));
#37733=CARTESIAN_POINT('Ctrl Pts',(-2.40811612696369,-1.,-3.09595472616076));
#37734=CARTESIAN_POINT('Ctrl Pts',(-2.40201704423341,-1.,-3.091572660511));
#37735=CARTESIAN_POINT('Ctrl Pts',(-2.39597098250631,-1.,-3.08717489512914));
#37736=CARTESIAN_POINT('Ctrl Pts',(-2.38997659219199,-1.,-3.08275773747093));
#37737=CARTESIAN_POINT('Ctrl Pts',(-2.38402401216126,-1.,-3.07830597244326));
#37738=CARTESIAN_POINT('Ctrl Pts',(-2.37809856205548,-1.,-3.07379777492165));
#37739=CARTESIAN_POINT('Ctrl Pts',(-2.37218678163178,-1.,-3.069212754975));
#37740=CARTESIAN_POINT('Ctrl Pts',(-2.36628220107009,-1.,-3.06453964643162));
#37741=CARTESIAN_POINT('Ctrl Pts',(-2.36039011602072,-1.,-3.0597826624004));
#37742=CARTESIAN_POINT('Ctrl Pts',(-2.35453559889474,-1.,-3.05497218368146));
#37743=CARTESIAN_POINT('Ctrl Pts',(-2.34875673090771,-1.,-3.05015565829918));
#37744=CARTESIAN_POINT('Ctrl Pts',(-2.34309017083977,-1.,-3.04537822217256));
#37745=CARTESIAN_POINT('Ctrl Pts',(-2.33755792953706,-1.,-3.04066496998544));
#37746=CARTESIAN_POINT('Ctrl Pts',(-2.33215619079829,-1.,-3.03600588555793));
#37747=CARTESIAN_POINT('Ctrl Pts',(-2.32683687412097,-1.,-3.03133125185136));
#37748=CARTESIAN_POINT('Ctrl Pts',(-2.32151944306402,-1.,-3.02652678416611));
#37749=CARTESIAN_POINT('Ctrl Pts',(-2.31612479121631,-1.,-3.02147780668161));
#37750=CARTESIAN_POINT('Ctrl Pts',(-2.31060449886629,-1.,-3.01610726819086));
#37751=CARTESIAN_POINT('Ctrl Pts',(-2.30496809486482,-1.,-3.01041131063823));
#37752=CARTESIAN_POINT('Ctrl Pts',(-2.29932091315775,-1.,-3.00450832658613));
#37753=CARTESIAN_POINT('Ctrl Pts',(-2.29385894577754,-1.,-2.99863310339691));
#37754=CARTESIAN_POINT('Ctrl Pts',(-2.28882328690362,-1.,-2.99307930984034));
#37755=CARTESIAN_POINT('Ctrl Pts',(-2.28446419115919,-1.,-2.9881543273478));
#37756=CARTESIAN_POINT('Ctrl Pts',(-2.28100472516679,-1.,-2.98413343613983));
#37757=CARTESIAN_POINT('Ctrl Pts',(-2.27877674853766,-1.,-2.9814234180956));
#37758=CARTESIAN_POINT('Ctrl Pts',(-2.27776738270289,-1.,-2.98007383024207));
#37759=CARTESIAN_POINT('Ctrl Pts',(-2.27743009389684,-1.,-2.9795116710597));
#37760=CARTESIAN_POINT('Ctrl Pts',(-2.27737238849287,-1.,-2.97932307137477));
#37761=CARTESIAN_POINT('Ctrl Pts',(-2.27737254473521,-1.,-2.97927412174279));
#37762=CARTESIAN_POINT('',(-2.12971124846838,-1.,-3.08655633322109));
#37763=CARTESIAN_POINT('Origin',(0.,-1.,0.));
#37764=CARTESIAN_POINT('',(-2.25898783642071,-1.,-3.54075895182139));
#37765=CARTESIAN_POINT('Ctrl Pts',(-2.12971124846838,-1.,-3.08655633322109));
#37766=CARTESIAN_POINT('Ctrl Pts',(-2.1297578506162,-1.,-3.0865713108946));
#37767=CARTESIAN_POINT('Ctrl Pts',(-2.12991938762497,-1.,-3.08668447250383));
#37768=CARTESIAN_POINT('Ctrl Pts',(-2.13034980480519,-1.,-3.08717896996213));
#37769=CARTESIAN_POINT('Ctrl Pts',(-2.13132142793056,-1.,-3.08855597949844));
#37770=CARTESIAN_POINT('Ctrl Pts',(-2.13321032560805,-1.,-3.09151235281832));
#37771=CARTESIAN_POINT('Ctrl Pts',(-2.13596538661154,-1.,-3.09604502421197));
#37772=CARTESIAN_POINT('Ctrl Pts',(-2.13930228863968,-1.,-3.1017126739137));
#37773=CARTESIAN_POINT('Ctrl Pts',(-2.14302815602195,-1.,-3.10821808669189));
#37774=CARTESIAN_POINT('Ctrl Pts',(-2.1469279845768,-1.,-3.11522827017075));
#37775=CARTESIAN_POINT('Ctrl Pts',(-2.15079698090627,-1.,-3.12242318152001));
#37776=CARTESIAN_POINT('Ctrl Pts',(-2.15447241382872,-1.,-3.12954386795575));
#37777=CARTESIAN_POINT('Ctrl Pts',(-2.15787423530583,-1.,-3.136453565629));
#37778=CARTESIAN_POINT('Ctrl Pts',(-2.16100905914341,-1.,-3.14314440426882));
#37779=CARTESIAN_POINT('Ctrl Pts',(-2.16393520288009,-1.,-3.14968624388961));
#37780=CARTESIAN_POINT('Ctrl Pts',(-2.1667372844767,-1.,-3.15618975593627));
#37781=CARTESIAN_POINT('Ctrl Pts',(-2.16949910801237,-1.,-3.16276685102999));
#37782=CARTESIAN_POINT('Ctrl Pts',(-2.17227212063857,-1.,-3.16948480019555));
#37783=CARTESIAN_POINT('Ctrl Pts',(-2.17506466903736,-1.,-3.17635032802584));
#37784=CARTESIAN_POINT('Ctrl Pts',(-2.17785968847172,-1.,-3.18333474627851));
#37785=CARTESIAN_POINT('Ctrl Pts',(-2.18062558031789,-1.,-3.19038924261589));
#37786=CARTESIAN_POINT('Ctrl Pts',(-2.18332898656595,-1.,-3.197462937404));
#37787=CARTESIAN_POINT('Ctrl Pts',(-2.18594876115914,-1.,-3.20452259717947));
#37788=CARTESIAN_POINT('Ctrl Pts',(-2.18848253363878,-1.,-3.21156188355736));
#37789=CARTESIAN_POINT('Ctrl Pts',(-2.1909390194865,-1.,-3.21859043114069));
#37790=CARTESIAN_POINT('Ctrl Pts',(-2.19333345123531,-1.,-3.22562734221636));
#37791=CARTESIAN_POINT('Ctrl Pts',(-2.19568204933172,-1.,-3.23269332296938));
#37792=CARTESIAN_POINT('Ctrl Pts',(-2.19799623693263,-1.,-3.23980245361323));
#37793=CARTESIAN_POINT('Ctrl Pts',(-2.20027910880993,-1.,-3.24695715874356));
#37794=CARTESIAN_POINT('Ctrl Pts',(-2.20252866491554,-1.,-3.25415277957789));
#37795=CARTESIAN_POINT('Ctrl Pts',(-2.20473979048682,-1.,-3.26138036637711));
#37796=CARTESIAN_POINT('Ctrl Pts',(-2.20690665217741,-1.,-3.2686300613678));
#37797=CARTESIAN_POINT('Ctrl Pts',(-2.20902509417425,-1.,-3.27589448005534));
#37798=CARTESIAN_POINT('Ctrl Pts',(-2.21109449750638,-1.,-3.28317133333127));
#37799=CARTESIAN_POINT('Ctrl Pts',(-2.21311648827391,-1.,-3.29046159238344));
#37800=CARTESIAN_POINT('Ctrl Pts',(-2.2150940692337,-1.,-3.29776825193162));
#37801=CARTESIAN_POINT('Ctrl Pts',(-2.21703059947837,-1.,-3.3050948781957));
#37802=CARTESIAN_POINT('Ctrl Pts',(-2.21892881679083,-1.,-3.31244421655662));
#37803=CARTESIAN_POINT('Ctrl Pts',(-2.22078990842768,-1.,-3.31981686778008));
#37804=CARTESIAN_POINT('Ctrl Pts',(-2.22261398879623,-1.,-3.32721196326019));
#37805=CARTESIAN_POINT('Ctrl Pts',(-2.224400498785,-1.,-3.3346277284958));
#37806=CARTESIAN_POINT('Ctrl Pts',(-2.22614863918044,-1.,-3.34206209449371));
#37807=CARTESIAN_POINT('Ctrl Pts',(-2.22785777756588,-1.,-3.34951327111117));
#37808=CARTESIAN_POINT('Ctrl Pts',(-2.22952789881011,-1.,-3.35698038165529));
#37809=CARTESIAN_POINT('Ctrl Pts',(-2.23115945849777,-1.,-3.36446325227908));
#37810=CARTESIAN_POINT('Ctrl Pts',(-2.23275319569253,-1.,-3.37196214349356));
#37811=CARTESIAN_POINT('Ctrl Pts',(-2.23430995599572,-1.,-3.37947749555649));
#37812=CARTESIAN_POINT('Ctrl Pts',(-2.23583052276281,-1.,-3.38700968549522));
#37813=CARTESIAN_POINT('Ctrl Pts',(-2.23731541452727,-1.,-3.39455873448088));
#37814=CARTESIAN_POINT('Ctrl Pts',(-2.23876491124064,-1.,-3.40212434705511));
#37815=CARTESIAN_POINT('Ctrl Pts',(-2.24017914395211,-1.,-3.40970604190205));
#37816=CARTESIAN_POINT('Ctrl Pts',(-2.24155816587811,-1.,-3.41730325539119));
#37817=CARTESIAN_POINT('Ctrl Pts',(-2.24290202531144,-1.,-3.42491544683075));
#37818=CARTESIAN_POINT('Ctrl Pts',(-2.24421085338856,-1.,-3.43254222615007));
#37819=CARTESIAN_POINT('Ctrl Pts',(-2.24548487526212,-1.,-3.44018336460619));
#37820=CARTESIAN_POINT('Ctrl Pts',(-2.24672437070139,-1.,-3.44783872863448));
#37821=CARTESIAN_POINT('Ctrl Pts',(-2.24792964960874,-1.,-3.45550823512213));
#37822=CARTESIAN_POINT('Ctrl Pts',(-2.24910102345977,-1.,-3.46319180177474));
#37823=CARTESIAN_POINT('Ctrl Pts',(-2.25023877475674,-1.,-3.47088928979467));
#37824=CARTESIAN_POINT('Ctrl Pts',(-2.25134314238258,-1.,-3.47860048448015));
#37825=CARTESIAN_POINT('Ctrl Pts',(-2.25241433138231,-1.,-3.48632513240231));
#37826=CARTESIAN_POINT('Ctrl Pts',(-2.25345251709453,-1.,-3.49406296494309));
#37827=CARTESIAN_POINT('Ctrl Pts',(-2.25445785151923,-1.,-3.50181372618058));
#37828=CARTESIAN_POINT('Ctrl Pts',(-2.25543046980351,-1.,-3.50957720118209));
#37829=CARTESIAN_POINT('Ctrl Pts',(-2.25637049456061,-1.,-3.51735323669213));
#37830=CARTESIAN_POINT('Ctrl Pts',(-2.25727802942141,-1.,-3.52514172849666));
#37831=CARTESIAN_POINT('Ctrl Pts',(-2.25797812951166,-1.,-3.53138243689932));
#37832=CARTESIAN_POINT('Ctrl Pts',(-2.25848864344599,-1.,-3.53606853163247));
#37833=CARTESIAN_POINT('Ctrl Pts',(-2.25882251694918,-1.,-3.5391950664771));
#37834=CARTESIAN_POINT('Ctrl Pts',(-2.25898783642071,-1.,-3.54075895182139));
#37835=CARTESIAN_POINT('',(-2.12928030988903,-1.,-3.62024382630768));
#37836=CARTESIAN_POINT('',(-2.25898783642071,-1.,-3.54075895182139));
#37837=CARTESIAN_POINT('',(-1.78327315618341,-1.,-3.29885386921513));
#37838=CARTESIAN_POINT('Ctrl Pts',(-2.12928030988903,-1.,-3.62024382630768));
#37839=CARTESIAN_POINT('Ctrl Pts',(-2.12796193131142,-1.,-3.61938653648716));
#37840=CARTESIAN_POINT('Ctrl Pts',(-2.12532774376144,-1.,-3.61766963589442));
#37841=CARTESIAN_POINT('Ctrl Pts',(-2.12138417125349,-1.,-3.61508732215187));
#37842=CARTESIAN_POINT('Ctrl Pts',(-2.11614149813928,-1.,-3.61163030607452));
#37843=CARTESIAN_POINT('Ctrl Pts',(-2.10961391333497,-1.,-3.60728578530968));
#37844=CARTESIAN_POINT('Ctrl Pts',(-2.10311217727687,-1.,-3.60291797087849));
#37845=CARTESIAN_POINT('Ctrl Pts',(-2.09663642986579,-1.,-3.59852681775396));
#37846=CARTESIAN_POINT('Ctrl Pts',(-2.09018686331706,-1.,-3.5941122862608));
#37847=CARTESIAN_POINT('Ctrl Pts',(-2.08376373049196,-1.,-3.58967435355834));
#37848=CARTESIAN_POINT('Ctrl Pts',(-2.07736732842524,-1.,-3.58521300039988));
#37849=CARTESIAN_POINT('Ctrl Pts',(-2.07099797606,-1.,-3.58072819250872));
#37850=CARTESIAN_POINT('Ctrl Pts',(-2.06465599229234,-1.,-3.57621986224402));
#37851=CARTESIAN_POINT('Ctrl Pts',(-2.05834167687425,-1.,-3.5716878942334));
#37852=CARTESIAN_POINT('Ctrl Pts',(-2.05205528172911,-1.,-3.56713209977904));
#37853=CARTESIAN_POINT('Ctrl Pts',(-2.04579702158876,-1.,-3.56255223871505));
#37854=CARTESIAN_POINT('Ctrl Pts',(-2.03956711119976,-1.,-3.55794807264844));
#37855=CARTESIAN_POINT('Ctrl Pts',(-2.03336579658133,-1.,-3.55331941293949));
#37856=CARTESIAN_POINT('Ctrl Pts',(-2.02719338376175,-1.,-3.54866616282227));
#37857=CARTESIAN_POINT('Ctrl Pts',(-2.02105027983104,-1.,-3.54398838254136));
#37858=CARTESIAN_POINT('Ctrl Pts',(-2.01493698847351,-1.,-3.53928627453642));
#37859=CARTESIAN_POINT('Ctrl Pts',(-2.00885403604746,-1.,-3.53456004727424));
#37860=CARTESIAN_POINT('Ctrl Pts',(-2.00280191090366,-1.,-3.52980980250224));
#37861=CARTESIAN_POINT('Ctrl Pts',(-1.99678100339296,-1.,-3.52503542491728));
#37862=CARTESIAN_POINT('Ctrl Pts',(-1.99079153006112,-1.,-3.52023644289142));
#37863=CARTESIAN_POINT('Ctrl Pts',(-1.9848335106103,-1.,-3.51541198728301));
#37864=CARTESIAN_POINT('Ctrl Pts',(-1.97890693666288,-1.,-3.51056110478287));
#37865=CARTESIAN_POINT('Ctrl Pts',(-1.97301191162968,-1.,-3.5056830186108));
#37866=CARTESIAN_POINT('Ctrl Pts',(-1.96714879724052,-1.,-3.50077740176267));
#37867=CARTESIAN_POINT('Ctrl Pts',(-1.961318367765,-1.,-3.49584466573064));
#37868=CARTESIAN_POINT('Ctrl Pts',(-1.95552193112084,-1.,-3.49088618670987));
#37869=CARTESIAN_POINT('Ctrl Pts',(-1.94976096795911,-1.,-3.48590361610814));
#37870=CARTESIAN_POINT('Ctrl Pts',(-1.94403680554065,-1.,-3.48089825770416));
#37871=CARTESIAN_POINT('Ctrl Pts',(-1.93835026973887,-1.,-3.47587040389915));
#37872=CARTESIAN_POINT('Ctrl Pts',(-1.93270136427081,-1.,-3.47081872409781));
#37873=CARTESIAN_POINT('Ctrl Pts',(-1.92708888591158,-1.,-3.46573953254084));
#37874=CARTESIAN_POINT('Ctrl Pts',(-1.92151118213212,-1.,-3.46062821722485));
#37875=CARTESIAN_POINT('Ctrl Pts',(-1.91596694784064,-1.,-3.4554807430995));
#37876=CARTESIAN_POINT('Ctrl Pts',(-1.91045605593639,-1.,-3.45029522038888));
#37877=CARTESIAN_POINT('Ctrl Pts',(-1.90498026502305,-1.,-3.44507323983367));
#37878=CARTESIAN_POINT('Ctrl Pts',(-1.89954426803384,-1.,-3.4398218567809));
#37879=CARTESIAN_POINT('Ctrl Pts',(-1.89415420002542,-1.,-3.43455074411571));
#37880=CARTESIAN_POINT('Ctrl Pts',(-1.88881571322009,-1.,-3.42926852222158));
#37881=CARTESIAN_POINT('Ctrl Pts',(-1.8835320506206,-1.,-3.42397908819736));
#37882=CARTESIAN_POINT('Ctrl Pts',(-1.87830245689344,-1.,-3.41867858383771));
#37883=CARTESIAN_POINT('Ctrl Pts',(-1.87311957248121,-1.,-3.41335043875209));
#37884=CARTESIAN_POINT('Ctrl Pts',(-1.86797231196654,-1.,-3.40797080000549));
#37885=CARTESIAN_POINT('Ctrl Pts',(-1.86285057051245,-1.,-3.40251742305476));
#37886=CARTESIAN_POINT('Ctrl Pts',(-1.85774972037062,-1.,-3.39697816833067));
#37887=CARTESIAN_POINT('Ctrl Pts',(-1.85267433291769,-1.,-3.39135802549398));
#37888=CARTESIAN_POINT('Ctrl Pts',(-1.84764441927753,-1.,-3.38569092349592));
#37889=CARTESIAN_POINT('Ctrl Pts',(-1.84269016931643,-1.,-3.38002968341157));
#37890=CARTESIAN_POINT('Ctrl Pts',(-1.83784072967077,-1.,-3.37442462015853));
#37891=CARTESIAN_POINT('Ctrl Pts',(-1.83311391452322,-1.,-3.36890396271836));
#37892=CARTESIAN_POINT('Ctrl Pts',(-1.82850752153199,-1.,-3.36345722124158));
#37893=CARTESIAN_POINT('Ctrl Pts',(-1.82398496829301,-1.,-3.35800801557424));
#37894=CARTESIAN_POINT('Ctrl Pts',(-1.81948458796829,-1.,-3.35243086937598));
#37895=CARTESIAN_POINT('Ctrl Pts',(-1.81494618732853,-1.,-3.34660014370673));
#37896=CARTESIAN_POINT('Ctrl Pts',(-1.81033399625352,-1.,-3.34043216147606));
#37897=CARTESIAN_POINT('Ctrl Pts',(-1.80565802981102,-1.,-3.33392460276808));
#37898=CARTESIAN_POINT('Ctrl Pts',(-1.80100380443406,-1.,-3.32721088039578));
#37899=CARTESIAN_POINT('Ctrl Pts',(-1.79652817033251,-1.,-3.3205535510082));
#37900=CARTESIAN_POINT('Ctrl Pts',(-1.79242331349949,-1.,-3.31428038326424));
#37901=CARTESIAN_POINT('Ctrl Pts',(-1.78888832245873,-1.,-3.30873412266788));
#37902=CARTESIAN_POINT('Ctrl Pts',(-1.78610045419846,-1.,-3.30422155559112));
#37903=CARTESIAN_POINT('Ctrl Pts',(-1.78432384788174,-1.,-3.30119637003393));
#37904=CARTESIAN_POINT('Ctrl Pts',(-1.78353803106924,-1.,-3.299705498242));
#37905=CARTESIAN_POINT('Ctrl Pts',(-1.78329283591905,-1.,-3.29909749657808));
#37906=CARTESIAN_POINT('Ctrl Pts',(-1.78326534445518,-1.,-3.29890219175423));
#37907=CARTESIAN_POINT('Ctrl Pts',(-1.78327315618341,-1.,-3.29885386921513));
#37908=CARTESIAN_POINT('',(-1.62064718014256,-1.,-3.38171594275687));
#37909=CARTESIAN_POINT('Origin',(0.,-1.,0.));
#37910=CARTESIAN_POINT('',(-1.67727921511438,-1.,-3.85054988729471));
#37911=CARTESIAN_POINT('Ctrl Pts',(-1.62064718014256,-1.,-3.38171594275687));
#37912=CARTESIAN_POINT('Ctrl Pts',(-1.62069086551626,-1.,-3.38173802621242));
#37913=CARTESIAN_POINT('Ctrl Pts',(-1.62083271136059,-1.,-3.38187506457001));
#37914=CARTESIAN_POINT('Ctrl Pts',(-1.62118047294574,-1.,-3.38243080602536));
#37915=CARTESIAN_POINT('Ctrl Pts',(-1.62192472202795,-1.,-3.3839428576331));
#37916=CARTESIAN_POINT('Ctrl Pts',(-1.62332788556183,-1.,-3.38715832178929));
#37917=CARTESIAN_POINT('Ctrl Pts',(-1.62533996116793,-1.,-3.39206617497078));
#37918=CARTESIAN_POINT('Ctrl Pts',(-1.62774916464571,-1.,-3.39818605298342));
#37919=CARTESIAN_POINT('Ctrl Pts',(-1.63041148964996,-1.,-3.40519422740596));
#37920=CARTESIAN_POINT('Ctrl Pts',(-1.63316667054156,-1.,-3.41272817148719));
#37921=CARTESIAN_POINT('Ctrl Pts',(-1.63586250099804,-1.,-3.4204397459095));
#37922=CARTESIAN_POINT('Ctrl Pts',(-1.6383787624689,-1.,-3.42804772926213));
#37923=CARTESIAN_POINT('Ctrl Pts',(-1.64065778701952,-1.,-3.43540451921397));
#37924=CARTESIAN_POINT('Ctrl Pts',(-1.64270733821042,-1.,-3.44250337701736));
#37925=CARTESIAN_POINT('Ctrl Pts',(-1.64457408708059,-1.,-3.44942242546693));
#37926=CARTESIAN_POINT('Ctrl Pts',(-1.64632429697506,-1.,-3.4562842106239));
#37927=CARTESIAN_POINT('Ctrl Pts',(-1.64802323352752,-1.,-3.46321237515029));
#37928=CARTESIAN_POINT('Ctrl Pts',(-1.64971118698285,-1.,-3.47028140996055));
#37929=CARTESIAN_POINT('Ctrl Pts',(-1.65139534930353,-1.,-3.47749926256543));
#37930=CARTESIAN_POINT('Ctrl Pts',(-1.65306335367762,-1.,-3.48483492840942));
#37931=CARTESIAN_POINT('Ctrl Pts',(-1.65469162644476,-1.,-3.49223525300194));
#37932=CARTESIAN_POINT('Ctrl Pts',(-1.65625517961583,-1.,-3.49964476477929));
#37933=CARTESIAN_POINT('Ctrl Pts',(-1.65773832633617,-1.,-3.5070273314651));
#37934=CARTESIAN_POINT('Ctrl Pts',(-1.65913971687324,-1.,-3.51437632188903));
#37935=CARTESIAN_POINT('Ctrl Pts',(-1.66046645222266,-1.,-3.52170261543787));
#37936=CARTESIAN_POINT('Ctrl Pts',(-1.66173058912365,-1.,-3.52902746211081));
#37937=CARTESIAN_POINT('Ctrl Pts',(-1.66294490916113,-1.,-3.53637385060225));
#37938=CARTESIAN_POINT('Ctrl Pts',(-1.66411849222334,-1.,-3.5437574747503));
#37939=CARTESIAN_POINT('Ctrl Pts',(-1.66525401569004,-1.,-3.5511812134288));
#37940=CARTESIAN_POINT('Ctrl Pts',(-1.66635023293121,-1.,-3.55864015233617));
#37941=CARTESIAN_POINT('Ctrl Pts',(-1.66740349220308,-1.,-3.56612465179429));
#37942=CARTESIAN_POINT('Ctrl Pts',(-1.66840957407299,-1.,-3.57362406285884));
#37943=CARTESIAN_POINT('Ctrl Pts',(-1.66936552908228,-1.,-3.58113044183823));
#37944=CARTESIAN_POINT('Ctrl Pts',(-1.67027110397601,-1.,-3.5886414309783));
#37945=CARTESIAN_POINT('Ctrl Pts',(-1.67112775290706,-1.,-3.59615824388808));
#37946=CARTESIAN_POINT('Ctrl Pts',(-1.67193797318598,-1.,-3.60368430815203));
#37947=CARTESIAN_POINT('Ctrl Pts',(-1.67270452466968,-1.,-3.61122367156182));
#37948=CARTESIAN_POINT('Ctrl Pts',(-1.67342968196223,-1.,-3.61877947398179));
#37949=CARTESIAN_POINT('Ctrl Pts',(-1.67411452372265,-1.,-3.62635249450908));
#37950=CARTESIAN_POINT('Ctrl Pts',(-1.67475929882962,-1.,-3.63394189312902));
#37951=CARTESIAN_POINT('Ctrl Pts',(-1.67536373264839,-1.,-3.6415458297232));
#37952=CARTESIAN_POINT('Ctrl Pts',(-1.6759273594669,-1.,-3.64916213574663));
#37953=CARTESIAN_POINT('Ctrl Pts',(-1.67644983469459,-1.,-3.65678894416442));
#37954=CARTESIAN_POINT('Ctrl Pts',(-1.67693128053153,-1.,-3.66442538671018));
#37955=CARTESIAN_POINT('Ctrl Pts',(-1.67737217414901,-1.,-3.67207136294639));
#37956=CARTESIAN_POINT('Ctrl Pts',(-1.67777320475872,-1.,-3.6797272457918));
#37957=CARTESIAN_POINT('Ctrl Pts',(-1.67813513867973,-1.,-3.68739360236505));
#37958=CARTESIAN_POINT('Ctrl Pts',(-1.67845869064304,-1.,-3.69507092759545));
#37959=CARTESIAN_POINT('Ctrl Pts',(-1.6787443694862,-1.,-3.70275932350998));
#37960=CARTESIAN_POINT('Ctrl Pts',(-1.67899249793398,-1.,-3.71045854208195));
#37961=CARTESIAN_POINT('Ctrl Pts',(-1.6792032807165,-1.,-3.71816812842188));
#37962=CARTESIAN_POINT('Ctrl Pts',(-1.67937685856627,-1.,-3.72588753416339));
#37963=CARTESIAN_POINT('Ctrl Pts',(-1.67951336376434,-1.,-3.73361623282617));
#37964=CARTESIAN_POINT('Ctrl Pts',(-1.67961298685316,-1.,-3.74135385965622));
#37965=CARTESIAN_POINT('Ctrl Pts',(-1.67967598599665,-1.,-3.74910022394845));
#37966=CARTESIAN_POINT('Ctrl Pts',(-1.67970265841379,-1.,-3.75685523754816));
#37967=CARTESIAN_POINT('Ctrl Pts',(-1.67969332319322,-1.,-3.76461886684523));
#37968=CARTESIAN_POINT('Ctrl Pts',(-1.67964830084946,-1.,-3.77239107928394));
#37969=CARTESIAN_POINT('Ctrl Pts',(-1.67956789211943,-1.,-3.78017178196859));
#37970=CARTESIAN_POINT('Ctrl Pts',(-1.67945236653175,-1.,-3.78796080021026));
#37971=CARTESIAN_POINT('Ctrl Pts',(-1.67930196625203,-1.,-3.7957579157763));
#37972=CARTESIAN_POINT('Ctrl Pts',(-1.67911690648128,-1.,-3.80356289078481));
#37973=CARTESIAN_POINT('Ctrl Pts',(-1.67889737738311,-1.,-3.81137549624273));
#37974=CARTESIAN_POINT('Ctrl Pts',(-1.67864354606363,-1.,-3.81919554100522));
#37975=CARTESIAN_POINT('Ctrl Pts',(-1.67835555760094,-1.,-3.82702289288453));
#37976=CARTESIAN_POINT('Ctrl Pts',(-1.67803353065273,-1.,-3.83485746516115));
#37977=CARTESIAN_POINT('Ctrl Pts',(-1.67774874946867,-1.,-3.8411308598706));
#37978=CARTESIAN_POINT('Ctrl Pts',(-1.67751991140661,-1.,-3.84583912297567));
#37979=CARTESIAN_POINT('Ctrl Pts',(-1.6773605765671,-1.,-3.84897939431104));
#37980=CARTESIAN_POINT('Ctrl Pts',(-1.67727921511438,-1.,-3.85054988729471));
#37981=CARTESIAN_POINT('',(-1.53673442965255,-1.,-3.90876544355381));
#37982=CARTESIAN_POINT('',(-1.67727921511438,-1.,-3.85054988729471));
#37983=CARTESIAN_POINT('',(-1.24526366418208,-1.,-3.5372048861591));
#37984=CARTESIAN_POINT('Ctrl Pts',(-1.53673442965255,-1.,-3.90876544355381));
#37985=CARTESIAN_POINT('Ctrl Pts',(-1.53556639217742,-1.,-3.90771246854607));
#37986=CARTESIAN_POINT('Ctrl Pts',(-1.53323321827311,-1.,-3.90560462812846));
#37987=CARTESIAN_POINT('Ctrl Pts',(-1.5297421605556,-1.,-3.90243719629755));
#37988=CARTESIAN_POINT('Ctrl Pts',(-1.52510482990784,-1.,-3.8982026070607));
#37989=CARTESIAN_POINT('Ctrl Pts',(-1.51933724328609,-1.,-3.89289043531893));
#37990=CARTESIAN_POINT('Ctrl Pts',(-1.51359883110181,-1.,-3.88755930032927));
#37991=CARTESIAN_POINT('Ctrl Pts',(-1.50788973857719,-1.,-3.88220917950443));
#37992=CARTESIAN_POINT('Ctrl Pts',(-1.50221016176766,-1.,-3.87684006372665));
#37993=CARTESIAN_POINT('Ctrl Pts',(-1.4965603539944,-1.,-3.8714519699927));
#37994=CARTESIAN_POINT('Ctrl Pts',(-1.49094061164604,-1.,-3.86604492575933));
#37995=CARTESIAN_POINT('Ctrl Pts',(-1.48535125510102,-1.,-3.86061894706551));
#37996=CARTESIAN_POINT('Ctrl Pts',(-1.47979260991063,-1.,-3.85517401698952));
#37997=CARTESIAN_POINT('Ctrl Pts',(-1.47426499018467,-1.,-3.84971006847096));
#37998=CARTESIAN_POINT('Ctrl Pts',(-1.46876867426375,-1.,-3.84422695454469));
#37999=CARTESIAN_POINT('Ctrl Pts',(-1.46330391180621,-1.,-3.83872447159309));
#38000=CARTESIAN_POINT('Ctrl Pts',(-1.45787095220763,-1.,-3.83320241775199));
#38001=CARTESIAN_POINT('Ctrl Pts',(-1.45247006796807,-1.,-3.82766064519));
#38002=CARTESIAN_POINT('Ctrl Pts',(-1.44710157648562,-1.,-3.82209910620591));
#38003=CARTESIAN_POINT('Ctrl Pts',(-1.44176587041401,-1.,-3.8165179239855));
#38004=CARTESIAN_POINT('Ctrl Pts',(-1.43646341556783,-1.,-3.81091737726965));
#38005=CARTESIAN_POINT('Ctrl Pts',(-1.43119469921364,-1.,-3.80529775429916));
#38006=CARTESIAN_POINT('Ctrl Pts',(-1.42596018777301,-1.,-3.79965923196365));
#38007=CARTESIAN_POINT('Ctrl Pts',(-1.42076028482828,-1.,-3.7940017574439));
#38008=CARTESIAN_POINT('Ctrl Pts',(-1.41559527803808,-1.,-3.78832489879369));
#38009=CARTESIAN_POINT('Ctrl Pts',(-1.41046532282567,-1.,-3.78262780065406));
#38010=CARTESIAN_POINT('Ctrl Pts',(-1.40537056004702,-1.,-3.77690952014209));
#38011=CARTESIAN_POINT('Ctrl Pts',(-1.40031121335495,-1.,-3.77116930621804));
#38012=CARTESIAN_POINT('Ctrl Pts',(-1.39528769118054,-1.,-3.76540689249078));
#38013=CARTESIAN_POINT('Ctrl Pts',(-1.39030069388926,-1.,-3.75962280650875));
#38014=CARTESIAN_POINT('Ctrl Pts',(-1.38535129801185,-1.,-3.75381861212728));
#38015=CARTESIAN_POINT('Ctrl Pts',(-1.38044070763302,-1.,-3.74799617204744));
#38016=CARTESIAN_POINT('Ctrl Pts',(-1.3755700297169,-1.,-3.7421569816256));
#38017=CARTESIAN_POINT('Ctrl Pts',(-1.37074003422739,-1.,-3.73630145885809));
#38018=CARTESIAN_POINT('Ctrl Pts',(-1.36595093298674,-1.,-3.73042829011293));
#38019=CARTESIAN_POINT('Ctrl Pts',(-1.36120211416353,-1.,-3.72453364678279));
#38020=CARTESIAN_POINT('Ctrl Pts',(-1.35649266705038,-1.,-3.71861271513318));
#38021=CARTESIAN_POINT('Ctrl Pts',(-1.35182193384426,-1.,-3.71266130563061));
#38022=CARTESIAN_POINT('Ctrl Pts',(-1.34719008463535,-1.,-3.7066775318825));
#38023=CARTESIAN_POINT('Ctrl Pts',(-1.3425986075293,-1.,-3.70066324015112));
#38024=CARTESIAN_POINT('Ctrl Pts',(-1.33805103398214,-1.,-3.69462613305692));
#38025=CARTESIAN_POINT('Ctrl Pts',(-1.33355191034515,-1.,-3.68857672413013));
#38026=CARTESIAN_POINT('Ctrl Pts',(-1.32910547072734,-1.,-3.68252441182534));
#38027=CARTESIAN_POINT('Ctrl Pts',(-1.32471430856413,-1.,-3.67647355257906));
#38028=CARTESIAN_POINT('Ctrl Pts',(-1.3203782813777,-1.,-3.67042021752668));
#38029=CARTESIAN_POINT('Ctrl Pts',(-1.31609271239922,-1.,-3.66434688899822));
#38030=CARTESIAN_POINT('Ctrl Pts',(-1.31185038411231,-1.,-3.65822827358655));
#38031=CARTESIAN_POINT('Ctrl Pts',(-1.30764479590051,-1.,-3.65204081987101));
#38032=CARTESIAN_POINT('Ctrl Pts',(-1.30347327603778,-1.,-3.64577181380125));
#38033=CARTESIAN_POINT('Ctrl Pts',(-1.29933955906463,-1.,-3.6394268987279));
#38034=CARTESIAN_POINT('Ctrl Pts',(-1.29525810207744,-1.,-3.63304271630995));
#38035=CARTESIAN_POINT('Ctrl Pts',(-1.29125046021853,-1.,-3.62667616004299));
#38036=CARTESIAN_POINT('Ctrl Pts',(-1.2873375502936,-1.,-3.62038148492295));
#38037=CARTESIAN_POINT('Ctrl Pts',(-1.28353255117754,-1.,-3.61418935913793));
#38038=CARTESIAN_POINT('Ctrl Pts',(-1.27983492861703,-1.,-3.60808907746372));
#38039=CARTESIAN_POINT('Ctrl Pts',(-1.27622049908664,-1.,-3.60199947736404));
#38040=CARTESIAN_POINT('Ctrl Pts',(-1.27264798379365,-1.,-3.59578698050164));
#38041=CARTESIAN_POINT('Ctrl Pts',(-1.26907758484766,-1.,-3.5893180784647));
#38042=CARTESIAN_POINT('Ctrl Pts',(-1.26548706249891,-1.,-3.58250452868699));
#38043=CARTESIAN_POINT('Ctrl Pts',(-1.26188667142784,-1.,-3.5753456065164));
#38044=CARTESIAN_POINT('Ctrl Pts',(-1.25834000485626,-1.,-3.56798645995025));
#38045=CARTESIAN_POINT('Ctrl Pts',(-1.25496090899873,-1.,-3.56071094990825));
#38046=CARTESIAN_POINT('Ctrl Pts',(-1.25188792940508,-1.,-3.5538728741862));
#38047=CARTESIAN_POINT('Ctrl Pts',(-1.24926408627938,-1.,-3.54784190282889));
#38048=CARTESIAN_POINT('Ctrl Pts',(-1.2472164623202,-1.,-3.54294877426113));
#38049=CARTESIAN_POINT('Ctrl Pts',(-1.24593497225964,-1.,-3.53968291129942));
#38050=CARTESIAN_POINT('Ctrl Pts',(-1.2453920538873,-1.,-3.53808746578052));
#38051=CARTESIAN_POINT('Ctrl Pts',(-1.24524498991133,-1.,-3.53744859265385));
#38052=CARTESIAN_POINT('Ctrl Pts',(-1.24524838931864,-1.,-3.53725139174402));
#38053=CARTESIAN_POINT('Ctrl Pts',(-1.24526366418208,-1.,-3.5372048861591));
#38054=CARTESIAN_POINT('',(-1.071677399622,-1.,-3.59360648251021));
#38055=CARTESIAN_POINT('Origin',(0.,-1.,0.));
#38056=CARTESIAN_POINT('',(-1.05427041296137,-1.,-4.06552750530042));
#38057=CARTESIAN_POINT('Ctrl Pts',(-1.071677399622,-1.,-3.59360648251021));
#38058=CARTESIAN_POINT('Ctrl Pts',(-1.07171709254271,-1.,-3.59363512797985));
#38059=CARTESIAN_POINT('Ctrl Pts',(-1.07183575450716,-1.,-3.59379266874663));
#38060=CARTESIAN_POINT('Ctrl Pts',(-1.07209229745284,-1.,-3.59439597));
#38061=CARTESIAN_POINT('Ctrl Pts',(-1.07259084660947,-1.,-3.59600583195037));
#38062=CARTESIAN_POINT('Ctrl Pts',(-1.0734737254567,-1.,-3.59940121154383));
#38063=CARTESIAN_POINT('Ctrl Pts',(-1.0746932716863,-1.,-3.6045633988796));
#38064=CARTESIAN_POINT('Ctrl Pts',(-1.07611545402841,-1.,-3.61098481349577));
#38065=CARTESIAN_POINT('Ctrl Pts',(-1.07764868137729,-1.,-3.61832318504957));
#38066=CARTESIAN_POINT('Ctrl Pts',(-1.07919137290815,-1.,-3.62619537902616));
#38067=CARTESIAN_POINT('Ctrl Pts',(-1.08064765719887,-1.,-3.63423373196602));
#38068=CARTESIAN_POINT('Ctrl Pts',(-1.08194278850972,-1.,-3.64214167843595));
#38069=CARTESIAN_POINT('Ctrl Pts',(-1.08304289898577,-1.,-3.64976441208197));
#38070=CARTESIAN_POINT('Ctrl Pts',(-1.08395671077761,-1.,-3.65709649161004));
#38071=CARTESIAN_POINT('Ctrl Pts',(-1.0847180992287,-1.,-3.66422237895256));
#38072=CARTESIAN_POINT('Ctrl Pts',(-1.0853733414448,-1.,-3.67127347729632));
#38073=CARTESIAN_POINT('Ctrl Pts',(-1.08596755755768,-1.,-3.67838211685148));
#38074=CARTESIAN_POINT('Ctrl Pts',(-1.08652888882609,-1.,-3.68562817420864));
#38075=CARTESIAN_POINT('Ctrl Pts',(-1.08706319540292,-1.,-3.69302062410229));
#38076=CARTESIAN_POINT('Ctrl Pts',(-1.08756311291324,-1.,-3.70052690909884));
#38077=CARTESIAN_POINT('Ctrl Pts',(-1.0880136731219,-1.,-3.70809084139476));
#38078=CARTESIAN_POINT('Ctrl Pts',(-1.08839887334777,-1.,-3.71565372339063));
#38079=CARTESIAN_POINT('Ctrl Pts',(-1.08870887220072,-1.,-3.72317741369364));
#38080=CARTESIAN_POINT('Ctrl Pts',(-1.08894337390925,-1.,-3.73065515162949));
#38081=CARTESIAN_POINT('Ctrl Pts',(-1.08910769013288,-1.,-3.73809879348209));
#38082=CARTESIAN_POINT('Ctrl Pts',(-1.08921040494013,-1.,-3.74553121371745));
#38083=CARTESIAN_POINT('Ctrl Pts',(-1.08926054632927,-1.,-3.75297711748138));
#38084=CARTESIAN_POINT('Ctrl Pts',(-1.08926462734287,-1.,-3.76045342580226));
#38085=CARTESIAN_POINT('Ctrl Pts',(-1.08922484204263,-1.,-3.76796340094469));
#38086=CARTESIAN_POINT('Ctrl Pts',(-1.08914072791275,-1.,-3.7755019940944));
#38087=CARTESIAN_POINT('Ctrl Pts',(-1.08901018614638,-1.,-3.78305911299511));
#38088=CARTESIAN_POINT('Ctrl Pts',(-1.08883071512097,-1.,-3.79062357974401));
#38089=CARTESIAN_POINT('Ctrl Pts',(-1.08860064435776,-1.,-3.79818708705252));
#38090=CARTESIAN_POINT('Ctrl Pts',(-1.08832009255378,-1.,-3.80574726657656));
#38091=CARTESIAN_POINT('Ctrl Pts',(-1.08799030610861,-1.,-3.81330554446324));
#38092=CARTESIAN_POINT('Ctrl Pts',(-1.08761321539442,-1.,-3.82086569676321));
#38093=CARTESIAN_POINT('Ctrl Pts',(-1.08719091307558,-1.,-3.82843215316985));
#38094=CARTESIAN_POINT('Ctrl Pts',(-1.08672515456901,-1.,-3.83600837071702));
#38095=CARTESIAN_POINT('Ctrl Pts',(-1.08621688337601,-1.,-3.84359528764934));
#38096=CARTESIAN_POINT('Ctrl Pts',(-1.08566647671838,-1.,-3.85119211322732));
#38097=CARTESIAN_POINT('Ctrl Pts',(-1.08507395120054,-1.,-3.85879698702511));
#38098=CARTESIAN_POINT('Ctrl Pts',(-1.08443918607926,-1.,-3.86640769434269));
#38099=CARTESIAN_POINT('Ctrl Pts',(-1.0837621330751,-1.,-3.87402233722563));
#38100=CARTESIAN_POINT('Ctrl Pts',(-1.08304304871042,-1.,-3.88164007721365));
#38101=CARTESIAN_POINT('Ctrl Pts',(-1.08228241999363,-1.,-3.88926088975182));
#38102=CARTESIAN_POINT('Ctrl Pts',(-1.08148086931373,-1.,-3.89688525098408));
#38103=CARTESIAN_POINT('Ctrl Pts',(-1.08063906483822,-1.,-3.90451384092564));
#38104=CARTESIAN_POINT('Ctrl Pts',(-1.0797576350746,-1.,-3.91214726022096));
#38105=CARTESIAN_POINT('Ctrl Pts',(-1.07883706663524,-1.,-3.91978568924062));
#38106=CARTESIAN_POINT('Ctrl Pts',(-1.07787771707155,-1.,-3.92742893349684));
#38107=CARTESIAN_POINT('Ctrl Pts',(-1.07687985975348,-1.,-3.93507657572743));
#38108=CARTESIAN_POINT('Ctrl Pts',(-1.07584371946428,-1.,-3.94272809633271));
#38109=CARTESIAN_POINT('Ctrl Pts',(-1.07476950921607,-1.,-3.95038299600754));
#38110=CARTESIAN_POINT('Ctrl Pts',(-1.07365747426551,-1.,-3.95804094429606));
#38111=CARTESIAN_POINT('Ctrl Pts',(-1.07250789943095,-1.,-3.96570179322681));
#38112=CARTESIAN_POINT('Ctrl Pts',(-1.07132109206252,-1.,-3.97336550222571));
#38113=CARTESIAN_POINT('Ctrl Pts',(-1.07009737257815,-1.,-3.98103208801289));
#38114=CARTESIAN_POINT('Ctrl Pts',(-1.06883706263912,-1.,-3.98870156857298));
#38115=CARTESIAN_POINT('Ctrl Pts',(-1.06754047381188,-1.,-3.99637389919958));
#38116=CARTESIAN_POINT('Ctrl Pts',(-1.06620789963406,-1.,-4.00404894951804));
#38117=CARTESIAN_POINT('Ctrl Pts',(-1.06483961342894,-1.,-4.0117265418656));
#38118=CARTESIAN_POINT('Ctrl Pts',(-1.06343586496094,-1.,-4.0194064749539));
#38119=CARTESIAN_POINT('Ctrl Pts',(-1.06199687787488,-1.,-4.02708855235732));
#38120=CARTESIAN_POINT('Ctrl Pts',(-1.06052284712114,-1.,-4.03477261142549));
#38121=CARTESIAN_POINT('Ctrl Pts',(-1.05901393667039,-1.,-4.04245854429333));
#38122=CARTESIAN_POINT('Ctrl Pts',(-1.05747027728537,-1.,-4.05014628387112));
#38123=CARTESIAN_POINT('Ctrl Pts',(-1.0562076270849,-1.,-4.05629789308941));
#38124=CARTESIAN_POINT('Ctrl Pts',(-1.05524507177901,-1.,-4.06091239150293));
#38125=CARTESIAN_POINT('Ctrl Pts',(-1.05459645194934,-1.,-4.06398907542679));
#38126=CARTESIAN_POINT('Ctrl Pts',(-1.05427041296137,-1.,-4.06552750530042));
#38127=CARTESIAN_POINT('',(-0.906349047628866,-1.,-4.10104028313088));
#38128=CARTESIAN_POINT('',(-1.05427041296137,-1.,-4.06552750530042));
#38129=CARTESIAN_POINT('',(-0.676591647975429,-1.,-3.68845817949586));
#38130=CARTESIAN_POINT('Ctrl Pts',(-0.906349047628866,-1.,-4.10104028313088));
#38131=CARTESIAN_POINT('Ctrl Pts',(-0.905360112215337,-1.,-4.09981755067523));
#38132=CARTESIAN_POINT('Ctrl Pts',(-0.903385402441587,-1.,-4.09737067245935));
#38133=CARTESIAN_POINT('Ctrl Pts',(-0.900432820941675,-1.,-4.09369611522387));
#38134=CARTESIAN_POINT('Ctrl Pts',(-0.896515019231333,-1.,-4.08878822246833));
#38135=CARTESIAN_POINT('Ctrl Pts',(-0.891649447916278,-1.,-4.08263920304799));
#38136=CARTESIAN_POINT('Ctrl Pts',(-0.886815658358501,-1.,-4.07647601773635));
#38137=CARTESIAN_POINT('Ctrl Pts',(-0.882013797525692,-1.,-4.07029866694192));
#38138=CARTESIAN_POINT('Ctrl Pts',(-0.877244060485837,-1.,-4.06410717232905));
#38139=CARTESIAN_POINT('Ctrl Pts',(-0.872506694782446,-1.,-4.0579015903134));
#38140=CARTESIAN_POINT('Ctrl Pts',(-0.867801988859917,-1.,-4.05168199437909));
#38141=CARTESIAN_POINT('Ctrl Pts',(-0.863130256643259,-1.,-4.04544845048584));
#38142=CARTESIAN_POINT('Ctrl Pts',(-0.858491822322827,-1.,-4.03920099284773));
#38143=CARTESIAN_POINT('Ctrl Pts',(-0.853887006631755,-1.,-4.03293960436756));
#38144=CARTESIAN_POINT('Ctrl Pts',(-0.849316107474245,-1.,-4.02666418343164));
#38145=CARTESIAN_POINT('Ctrl Pts',(-0.844779403287745,-1.,-4.02037456798441));
#38146=CARTESIAN_POINT('Ctrl Pts',(-0.840277171975855,-1.,-4.01407059766103));
#38147=CARTESIAN_POINT('Ctrl Pts',(-0.835809705809646,-1.,-4.00775216907856));
#38148=CARTESIAN_POINT('Ctrl Pts',(-0.831377325741622,-1.,-4.00141928477507));
#38149=CARTESIAN_POINT('Ctrl Pts',(-0.826980400320789,-1.,-3.99507212784431));
#38150=CARTESIAN_POINT('Ctrl Pts',(-0.822619346022119,-1.,-3.98871104646485));
#38151=CARTESIAN_POINT('Ctrl Pts',(-0.818294599022293,-1.,-3.98233640155404));
#38152=CARTESIAN_POINT('Ctrl Pts',(-0.814006592328844,-1.,-3.97594844078811));
#38153=CARTESIAN_POINT('Ctrl Pts',(-0.809755732818091,-1.,-3.96954717513232));
#38154=CARTESIAN_POINT('Ctrl Pts',(-0.805542372178361,-1.,-3.96313222295815));
#38155=CARTESIAN_POINT('Ctrl Pts',(-0.801366797727049,-1.,-3.95670276375108));
#38156=CARTESIAN_POINT('Ctrl Pts',(-0.797229296085316,-1.,-3.95025788827136));
#38157=CARTESIAN_POINT('Ctrl Pts',(-0.793130205640961,-1.,-3.94379688971283));
#38158=CARTESIAN_POINT('Ctrl Pts',(-0.789069971469333,-1.,-3.93731956885676));
#38159=CARTESIAN_POINT('Ctrl Pts',(-0.785049202786507,-1.,-3.93082655631789));
#38160=CARTESIAN_POINT('Ctrl Pts',(-0.781068718228451,-1.,-3.92431956510441));
#38161=CARTESIAN_POINT('Ctrl Pts',(-0.777129415664956,-1.,-3.9178006233448));
#38162=CARTESIAN_POINT('Ctrl Pts',(-0.773232154506321,-1.,-3.91127138115243));
#38163=CARTESIAN_POINT('Ctrl Pts',(-0.769377629847874,-1.,-3.90473237182633));
#38164=CARTESIAN_POINT('Ctrl Pts',(-0.765566256401295,-1.,-3.89818233104378));
#38165=CARTESIAN_POINT('Ctrl Pts',(-0.76179802879397,-1.,-3.89161738162245));
#38166=CARTESIAN_POINT('Ctrl Pts',(-0.758072800564801,-1.,-3.88503262662689));
#38167=CARTESIAN_POINT('Ctrl Pts',(-0.754390577396856,-1.,-3.87842382520065));
#38168=CARTESIAN_POINT('Ctrl Pts',(-0.750751822383028,-1.,-3.87178914078374));
#38169=CARTESIAN_POINT('Ctrl Pts',(-0.747157716488871,-1.,-3.86513062969889));
#38170=CARTESIAN_POINT('Ctrl Pts',(-0.743610542737012,-1.,-3.85845645217594));
#38171=CARTESIAN_POINT('Ctrl Pts',(-0.740113146827137,-1.,-3.85177770351215));
#38172=CARTESIAN_POINT('Ctrl Pts',(-0.736668240497117,-1.,-3.84510432881213));
#38173=CARTESIAN_POINT('Ctrl Pts',(-0.733277703756078,-1.,-3.83844103658009));
#38174=CARTESIAN_POINT('Ctrl Pts',(-0.729942010490168,-1.,-3.83178392403383));
#38175=CARTESIAN_POINT('Ctrl Pts',(-0.726659281876664,-1.,-3.82511495756713));
#38176=CARTESIAN_POINT('Ctrl Pts',(-0.723426346019423,-1.,-3.81840802610835));
#38177=CARTESIAN_POINT('Ctrl Pts',(-0.720240466589236,-1.,-3.81163885127344));
#38178=CARTESIAN_POINT('Ctrl Pts',(-0.717100993669114,-1.,-3.80479445759309));
#38179=CARTESIAN_POINT('Ctrl Pts',(-0.714010733006641,-1.,-3.79788100314975));
#38180=CARTESIAN_POINT('Ctrl Pts',(-0.710978231689017,-1.,-3.79093694007094));
#38181=CARTESIAN_POINT('Ctrl Pts',(-0.708015879375459,-1.,-3.78402183336605));
#38182=CARTESIAN_POINT('Ctrl Pts',(-0.705135847999817,-1.,-3.77719254217129));
#38183=CARTESIAN_POINT('Ctrl Pts',(-0.702346356621552,-1.,-3.77048141872872));
#38184=CARTESIAN_POINT('Ctrl Pts',(-0.699648552230917,-1.,-3.76387780603759));
#38185=CARTESIAN_POINT('Ctrl Pts',(-0.697031245659744,-1.,-3.75729775767023));
#38186=CARTESIAN_POINT('Ctrl Pts',(-0.694474562581493,-1.,-3.75060288243455));
#38187=CARTESIAN_POINT('Ctrl Pts',(-0.69196008040082,-1.,-3.74365508986712));
#38188=CARTESIAN_POINT('Ctrl Pts',(-0.689479637354814,-1.,-3.73636374475077));
#38189=CARTESIAN_POINT('Ctrl Pts',(-0.687043475232355,-1.,-3.72872973554051));
#38190=CARTESIAN_POINT('Ctrl Pts',(-0.684691698167848,-1.,-3.7209063713926));
#38191=CARTESIAN_POINT('Ctrl Pts',(-0.68249234510893,-1.,-3.71319182789943));
#38192=CARTESIAN_POINT('Ctrl Pts',(-0.680526909710877,-1.,-3.70595722031785));
#38193=CARTESIAN_POINT('Ctrl Pts',(-0.678878822226026,-1.,-3.69959004073005));
#38194=CARTESIAN_POINT('Ctrl Pts',(-0.677621861865498,-1.,-3.69443683573598));
#38195=CARTESIAN_POINT('Ctrl Pts',(-0.676867042599401,-1.,-3.69101071175464));
#38196=CARTESIAN_POINT('Ctrl Pts',(-0.676580391119396,-1.,-3.68934997767243));
#38197=CARTESIAN_POINT('Ctrl Pts',(-0.676535079520807,-1.,-3.68869596425969));
#38198=CARTESIAN_POINT('Ctrl Pts',(-0.676569286094606,-1.,-3.68850172300477));
#38199=CARTESIAN_POINT('Ctrl Pts',(-0.676591647975429,-1.,-3.68845817949586));
#38200=CARTESIAN_POINT('',(-0.496319364829374,-1.,-3.71701050416802));
#38201=CARTESIAN_POINT('Origin',(0.,-1.,0.));
#38202=CARTESIAN_POINT('',(-0.405301974318349,-1.,-4.18039834341342));
#38203=CARTESIAN_POINT('Ctrl Pts',(-0.496319364829374,-1.,-3.71701050416802));
#38204=CARTESIAN_POINT('Ctrl Pts',(-0.496354087925646,-1.,-3.71704500630521));
#38205=CARTESIAN_POINT('Ctrl Pts',(-0.496446644158827,-1.,-3.71721917030465));
#38206=CARTESIAN_POINT('Ctrl Pts',(-0.496605651526314,-1.,-3.71785517607694));
#38207=CARTESIAN_POINT('Ctrl Pts',(-0.496846224822535,-1.,-3.7195232082259));
#38208=CARTESIAN_POINT('Ctrl Pts',(-0.497187079575794,-1.,-3.72301489774241));
#38209=CARTESIAN_POINT('Ctrl Pts',(-0.497584067153279,-1.,-3.72830430904794));
#38210=CARTESIAN_POINT('Ctrl Pts',(-0.497984209510495,-1.,-3.73486914372834));
#38211=CARTESIAN_POINT('Ctrl Pts',(-0.498350586058176,-1.,-3.74235701735109));
#38212=CARTESIAN_POINT('Ctrl Pts',(-0.498642802042929,-1.,-3.75037362168103));
#38213=CARTESIAN_POINT('Ctrl Pts',(-0.498823681615513,-1.,-3.75854082221127));
#38214=CARTESIAN_POINT('Ctrl Pts',(-0.498865792335185,-1.,-3.76655401191144));
#38215=CARTESIAN_POINT('Ctrl Pts',(-0.498759900365687,-1.,-3.77425499225089));
#38216=CARTESIAN_POINT('Ctrl Pts',(-0.498515471679378,-1.,-3.78163975337189));
#38217=CARTESIAN_POINT('Ctrl Pts',(-0.498152751800819,-1.,-3.78879701661152));
#38218=CARTESIAN_POINT('Ctrl Pts',(-0.49769689210058,-1.,-3.79586380669959));
#38219=CARTESIAN_POINT('Ctrl Pts',(-0.497171756201091,-1.,-3.80297788298545));
#38220=CARTESIAN_POINT('Ctrl Pts',(-0.496592643443789,-1.,-3.81022254090909));
#38221=CARTESIAN_POINT('Ctrl Pts',(-0.495963937875572,-1.,-3.81760756144099));
#38222=CARTESIAN_POINT('Ctrl Pts',(-0.495283458893903,-1.,-3.82509963594156));
#38223=CARTESIAN_POINT('Ctrl Pts',(-0.494545212256425,-1.,-3.8326409268245));
#38224=CARTESIAN_POINT('Ctrl Pts',(-0.493742574629117,-1.,-3.84017095578438));
#38225=CARTESIAN_POINT('Ctrl Pts',(-0.492871792414095,-1.,-3.84765051147965));
#38226=CARTESIAN_POINT('Ctrl Pts',(-0.49193363108376,-1.,-3.85507287020223));
#38227=CARTESIAN_POINT('Ctrl Pts',(-0.490931482170849,-1.,-3.86245057319215));
#38228=CARTESIAN_POINT('Ctrl Pts',(-0.489870245704899,-1.,-3.86980755613694));
#38229=CARTESIAN_POINT('Ctrl Pts',(-0.488754973798281,-1.,-3.87716963231115));
#38230=CARTESIAN_POINT('Ctrl Pts',(-0.487589452275179,-1.,-3.88455453328156));
#38231=CARTESIAN_POINT('Ctrl Pts',(-0.486375337854133,-1.,-3.89196582437574));
#38232=CARTESIAN_POINT('Ctrl Pts',(-0.485112963522246,-1.,-3.89939844658529));
#38233=CARTESIAN_POINT('Ctrl Pts',(-0.483801835089161,-1.,-3.90684210358063));
#38234=CARTESIAN_POINT('Ctrl Pts',(-0.482441230340709,-1.,-3.91428536373749));
#38235=CARTESIAN_POINT('Ctrl Pts',(-0.481030798910735,-1.,-3.92171976072334));
#38236=CARTESIAN_POINT('Ctrl Pts',(-0.479571028525566,-1.,-3.92914297392067));
#38237=CARTESIAN_POINT('Ctrl Pts',(-0.478062927140957,-1.,-3.93655660689819));
#38238=CARTESIAN_POINT('Ctrl Pts',(-0.476507810658535,-1.,-3.94396469119385));
#38239=CARTESIAN_POINT('Ctrl Pts',(-0.47490705302179,-1.,-3.95137192932898));
#38240=CARTESIAN_POINT('Ctrl Pts',(-0.473261847236296,-1.,-3.95878201038332));
#38241=CARTESIAN_POINT('Ctrl Pts',(-0.471572978413493,-1.,-3.96619600864626));
#38242=CARTESIAN_POINT('Ctrl Pts',(-0.469840942829878,-1.,-3.97361320212413));
#38243=CARTESIAN_POINT('Ctrl Pts',(-0.46806604792014,-1.,-3.98103175589349));
#38244=CARTESIAN_POINT('Ctrl Pts',(-0.466248520883034,-1.,-3.98844946363258));
#38245=CARTESIAN_POINT('Ctrl Pts',(-0.464388610938995,-1.,-3.99586444320134));
#38246=CARTESIAN_POINT('Ctrl Pts',(-0.462486702616252,-1.,-4.00327590659129));
#38247=CARTESIAN_POINT('Ctrl Pts',(-0.460543280768577,-1.,-4.01068390573469));
#38248=CARTESIAN_POINT('Ctrl Pts',(-0.458558885637001,-1.,-4.01808900827647));
#38249=CARTESIAN_POINT('Ctrl Pts',(-0.456534070784968,-1.,-4.02549199038414));
#38250=CARTESIAN_POINT('Ctrl Pts',(-0.454469363020495,-1.,-4.03289354362745));
#38251=CARTESIAN_POINT('Ctrl Pts',(-0.452365214748779,-1.,-4.0402939222793));
#38252=CARTESIAN_POINT('Ctrl Pts',(-0.450222009543774,-1.,-4.0476929901797));
#38253=CARTESIAN_POINT('Ctrl Pts',(-0.448040082683976,-1.,-4.05509037796815));
#38254=CARTESIAN_POINT('Ctrl Pts',(-0.445819737468478,-1.,-4.06248560760596));
#38255=CARTESIAN_POINT('Ctrl Pts',(-0.443561262395408,-1.,-4.0698782192577));
#38256=CARTESIAN_POINT('Ctrl Pts',(-0.441264951396587,-1.,-4.07726792490256));
#38257=CARTESIAN_POINT('Ctrl Pts',(-0.438931108931613,-1.,-4.08465462294625));
#38258=CARTESIAN_POINT('Ctrl Pts',(-0.436560044913814,-1.,-4.09203832139439));
#38259=CARTESIAN_POINT('Ctrl Pts',(-0.434152073200643,-1.,-4.09941908688567));
#38260=CARTESIAN_POINT('Ctrl Pts',(-0.431707508679772,-1.,-4.10679698750219));
#38261=CARTESIAN_POINT('Ctrl Pts',(-0.429226666075372,-1.,-4.1141720278277));
#38262=CARTESIAN_POINT('Ctrl Pts',(-0.426709855706243,-1.,-4.1215441250121));
#38263=CARTESIAN_POINT('Ctrl Pts',(-0.424157375323155,-1.,-4.1289131463371));
#38264=CARTESIAN_POINT('Ctrl Pts',(-0.421569503103971,-1.,-4.13627893206433));
#38265=CARTESIAN_POINT('Ctrl Pts',(-0.4189464906678,-1.,-4.14364132317223));
#38266=CARTESIAN_POINT('Ctrl Pts',(-0.416288556008986,-1.,-4.15100018950989));
#38267=CARTESIAN_POINT('Ctrl Pts',(-0.413595877953269,-1.,-4.1583554501909));
#38268=CARTESIAN_POINT('Ctrl Pts',(-0.410868596148614,-1.,-4.16570705940731));
#38269=CARTESIAN_POINT('Ctrl Pts',(-0.408659167570153,-1.,-4.17158541009947));
#38270=CARTESIAN_POINT('Ctrl Pts',(-0.406986596326602,-1.,-4.17599251955585));
#38271=CARTESIAN_POINT('Ctrl Pts',(-0.405864662679631,-1.,-4.17892985789908));
#38272=CARTESIAN_POINT('Ctrl Pts',(-0.405301974318349,-1.,-4.18039834341342));
#38273=CARTESIAN_POINT('',(-0.253646344052521,-1.,-4.1923339003649));
#38274=CARTESIAN_POINT('',(-0.405301974318349,-1.,-4.18039834341342));
#38275=CARTESIAN_POINT('',(-0.0912596999166825,-1.,-3.74888939116255));
#38276=CARTESIAN_POINT('Ctrl Pts',(-0.253646344052521,-1.,-4.1923339003649));
#38277=CARTESIAN_POINT('Ctrl Pts',(-0.252860861572565,-1.,-4.19097151819241));
#38278=CARTESIAN_POINT('Ctrl Pts',(-0.251293239837693,-1.,-4.18824585244066));
#38279=CARTESIAN_POINT('Ctrl Pts',(-0.248951836910964,-1.,-4.18415464959491));
#38280=CARTESIAN_POINT('Ctrl Pts',(-0.245850033418583,-1.,-4.17869430192868));
#38281=CARTESIAN_POINT('Ctrl Pts',(-0.242006283923912,-1.,-4.17185984409533));
#38282=CARTESIAN_POINT('Ctrl Pts',(-0.238196140933977,-1.,-4.1650163665385));
#38283=CARTESIAN_POINT('Ctrl Pts',(-0.234419749543143,-1.,-4.1581638926525));
#38284=CARTESIAN_POINT('Ctrl Pts',(-0.230677299028738,-1.,-4.15130247435029));
#38285=CARTESIAN_POINT('Ctrl Pts',(-0.226969025061243,-1.,-4.14443220607733));
#38286=CARTESIAN_POINT('Ctrl Pts',(-0.223295201038383,-1.,-4.13755320553563));
#38287=CARTESIAN_POINT('Ctrl Pts',(-0.219656126701852,-1.,-4.13066558698156));
#38288=CARTESIAN_POINT('Ctrl Pts',(-0.216052116898425,-1.,-4.12376943492249));
#38289=CARTESIAN_POINT('Ctrl Pts',(-0.212483491087068,-1.,-4.11686478264545));
#38290=CARTESIAN_POINT('Ctrl Pts',(-0.208950559400172,-1.,-4.10995157639026));
#38291=CARTESIAN_POINT('Ctrl Pts',(-0.205453622198233,-1.,-4.10302969965374));
#38292=CARTESIAN_POINT('Ctrl Pts',(-0.201992979049984,-1.,-4.09609903751912));
#38293=CARTESIAN_POINT('Ctrl Pts',(-0.198568934800811,-1.,-4.08915953359753));
#38294=CARTESIAN_POINT('Ctrl Pts',(-0.195181806054714,-1.,-4.08221124060385));
#38295=CARTESIAN_POINT('Ctrl Pts',(-0.191831928181081,-1.,-4.07525439703137));
#38296=CARTESIAN_POINT('Ctrl Pts',(-0.188519658060255,-1.,-4.06828941192308));
#38297=CARTESIAN_POINT('Ctrl Pts',(-0.185245370038948,-1.,-4.06131670998589));
#38298=CARTESIAN_POINT('Ctrl Pts',(-0.18200945304855,-1.,-4.05433660358402));
#38299=CARTESIAN_POINT('Ctrl Pts',(-0.178812307240716,-1.,-4.04734916719722));
#38300=CARTESIAN_POINT('Ctrl Pts',(-0.175654339673757,-1.,-4.04035407891161));
#38301=CARTESIAN_POINT('Ctrl Pts',(-0.172535962484466,-1.,-4.03335057326093));
#38302=CARTESIAN_POINT('Ctrl Pts',(-0.169457601001653,-1.,-4.0263377970371));
#38303=CARTESIAN_POINT('Ctrl Pts',(-0.166419700015847,-1.,-4.01931510507143));
#38304=CARTESIAN_POINT('Ctrl Pts',(-0.163422730287459,-1.,-4.01228237022301));
#38305=CARTESIAN_POINT('Ctrl Pts',(-0.160467194882219,-1.,-4.00524031064509));
#38306=CARTESIAN_POINT('Ctrl Pts',(-0.15755363438381,-1.,-3.99819074631874));
#38307=CARTESIAN_POINT('Ctrl Pts',(-0.154682618338563,-1.,-3.99113582086059));
#38308=CARTESIAN_POINT('Ctrl Pts',(-0.151854737441405,-1.,-3.9840772985098));
#38309=CARTESIAN_POINT('Ctrl Pts',(-0.149070594803544,-1.,-3.97701581473643));
#38310=CARTESIAN_POINT('Ctrl Pts',(-0.146330797814513,-1.,-3.96995018565891));
#38311=CARTESIAN_POINT('Ctrl Pts',(-0.143635947692791,-1.,-3.96287658098896));
#38312=CARTESIAN_POINT('Ctrl Pts',(-0.140986665829937,-1.,-3.95579014116899));
#38313=CARTESIAN_POINT('Ctrl Pts',(-0.138383621255159,-1.,-3.94868667844355));
#38314=CARTESIAN_POINT('Ctrl Pts',(-0.135827558661188,-1.,-3.94156445130744));
#38315=CARTESIAN_POINT('Ctrl Pts',(-0.13331932279419,-1.,-3.93442567551035));
#38316=CARTESIAN_POINT('Ctrl Pts',(-0.130859892027799,-1.,-3.9272787679596));
#38317=CARTESIAN_POINT('Ctrl Pts',(-0.128450341339528,-1.,-3.92013513251642));
#38318=CARTESIAN_POINT('Ctrl Pts',(-0.126091793324137,-1.,-3.91300501605392));
#38319=CARTESIAN_POINT('Ctrl Pts',(-0.123785368272377,-1.,-3.90589336320508));
#38320=CARTESIAN_POINT('Ctrl Pts',(-0.121532144765723,-1.,-3.89879639336952));
#38321=CARTESIAN_POINT('Ctrl Pts',(-0.119333088190417,-1.,-3.89169600105201));
#38322=CARTESIAN_POINT('Ctrl Pts',(-0.117189150373144,-1.,-3.88456590045767));
#38323=CARTESIAN_POINT('Ctrl Pts',(-0.11510142664947,-1.,-3.87738168405343));
#38324=CARTESIAN_POINT('Ctrl Pts',(-0.113071304914562,-1.,-3.87013043445014));
#38325=CARTESIAN_POINT('Ctrl Pts',(-0.11110059303626,-1.,-3.86281867282965));
#38326=CARTESIAN_POINT('Ctrl Pts',(-0.109191717634944,-1.,-3.855485714969));
#38327=CARTESIAN_POINT('Ctrl Pts',(-0.107347597812184,-1.,-3.84819233070317));
#38328=CARTESIAN_POINT('Ctrl Pts',(-0.105571360916569,-1.,-3.84099658324803));
#38329=CARTESIAN_POINT('Ctrl Pts',(-0.103866063811623,-1.,-3.83393171228002));
#38330=CARTESIAN_POINT('Ctrl Pts',(-0.102234506488456,-1.,-3.82698737143255));
#38331=CARTESIAN_POINT('Ctrl Pts',(-0.100678769650632,-1.,-3.82007889742625));
#38332=CARTESIAN_POINT('Ctrl Pts',(-0.0992008728096516,-1.,-3.81306649386461));
#38333=CARTESIAN_POINT('Ctrl Pts',(-0.0978042222906645,-1.,-3.80581088847809));
#38334=CARTESIAN_POINT('Ctrl Pts',(-0.0964949352873133,-1.,-3.79822128513845));
#38335=CARTESIAN_POINT('Ctrl Pts',(-0.0952829885100802,-1.,-3.79030016353111));
#38336=CARTESIAN_POINT('Ctrl Pts',(-0.0941840095090815,-1.,-3.782205218991));
#38337=CARTESIAN_POINT('Ctrl Pts',(-0.093218554620318,-1.,-3.77424159971059));
#38338=CARTESIAN_POINT('Ctrl Pts',(-0.0924090589602692,-1.,-3.76678860031841));
#38339=CARTESIAN_POINT('Ctrl Pts',(-0.0917773084998337,-1.,-3.76024199359303));
#38340=CARTESIAN_POINT('Ctrl Pts',(-0.09134196227364,-1.,-3.75495560118212));
#38341=CARTESIAN_POINT('Ctrl Pts',(-0.0911323999574428,-1.,-3.75145357872422));
#38342=CARTESIAN_POINT('Ctrl Pts',(-0.0911090736805512,-1.,-3.74976844886346));
#38343=CARTESIAN_POINT('Ctrl Pts',(-0.0911666301812819,-1.,-3.74911539914542));
#38344=CARTESIAN_POINT('Ctrl Pts',(-0.0912308016421982,-1.,-3.74892890040974));
#38345=CARTESIAN_POINT('Ctrl Pts',(-0.0912596999166825,-1.,-3.74888939116255));
#38346=CARTESIAN_POINT('',(0.0912596999148854,-1.,-3.74888939116259));
#38347=CARTESIAN_POINT('Origin',(0.,-1.,0.));
#38348=CARTESIAN_POINT('',(0.253646344052522,-1.,-4.1923339003649));
#38349=CARTESIAN_POINT('Ctrl Pts',(0.0912596999148854,-1.,-3.74888939116259));
#38350=CARTESIAN_POINT('Ctrl Pts',(0.0912308016409229,-1.,-3.74892890041021));
#38351=CARTESIAN_POINT('Ctrl Pts',(0.0911666301806421,-1.,-3.74911539914664));
#38352=CARTESIAN_POINT('Ctrl Pts',(0.0911090736804568,-1.,-3.74976844886495));
#38353=CARTESIAN_POINT('Ctrl Pts',(0.0911323999576141,-1.,-3.75145357872511));
#38354=CARTESIAN_POINT('Ctrl Pts',(0.0913419622735849,-1.,-3.75495560118053));
#38355=CARTESIAN_POINT('Ctrl Pts',(0.0917773084999005,-1.,-3.76024199359493));
#38356=CARTESIAN_POINT('Ctrl Pts',(0.0924090589604052,-1.,-3.76678860032228));
#38357=CARTESIAN_POINT('Ctrl Pts',(0.0932185546204571,-1.,-3.77424159971456));
#38358=CARTESIAN_POINT('Ctrl Pts',(0.094184009509174,-1.,-3.78220521899366));
#38359=CARTESIAN_POINT('Ctrl Pts',(0.0952829885101065,-1.,-3.79030016353186));
#38360=CARTESIAN_POINT('Ctrl Pts',(0.0964949352872842,-1.,-3.7982212851376));
#38361=CARTESIAN_POINT('Ctrl Pts',(0.0978042222906071,-1.,-3.80581088847642));
#38362=CARTESIAN_POINT('Ctrl Pts',(0.099200872809594,-1.,-3.81306649386293));
#38363=CARTESIAN_POINT('Ctrl Pts',(0.100678769650594,-1.,-3.82007889742512));
#38364=CARTESIAN_POINT('Ctrl Pts',(0.102234506488445,-1.,-3.8269873714322));
#38365=CARTESIAN_POINT('Ctrl Pts',(0.103866063811634,-1.,-3.83393171228034));
#38366=CARTESIAN_POINT('Ctrl Pts',(0.105571360916593,-1.,-3.84099658324873));
#38367=CARTESIAN_POINT('Ctrl Pts',(0.107347597812208,-1.,-3.84819233070391));
#38368=CARTESIAN_POINT('Ctrl Pts',(0.10919171763496,-1.,-3.85548571496953));
#38369=CARTESIAN_POINT('Ctrl Pts',(0.111100593036266,-1.,-3.86281867282984));
#38370=CARTESIAN_POINT('Ctrl Pts',(0.113071304914558,-1.,-3.87013043445001));
#38371=CARTESIAN_POINT('Ctrl Pts',(0.11510142664946,-1.,-3.87738168405308));
#38372=CARTESIAN_POINT('Ctrl Pts',(0.117189150373134,-1.,-3.88456590045726));
#38373=CARTESIAN_POINT('Ctrl Pts',(0.11933308819041,-1.,-3.8916960010517));
#38374=CARTESIAN_POINT('Ctrl Pts',(0.121532144765721,-1.,-3.89879639336939));
#38375=CARTESIAN_POINT('Ctrl Pts',(0.123785368272379,-1.,-3.90589336320515));
#38376=CARTESIAN_POINT('Ctrl Pts',(0.126091793324141,-1.,-3.91300501605411));
#38377=CARTESIAN_POINT('Ctrl Pts',(0.128450341339532,-1.,-3.92013513251664));
#38378=CARTESIAN_POINT('Ctrl Pts',(0.130859892027801,-1.,-3.92727876795977));
#38379=CARTESIAN_POINT('Ctrl Pts',(0.13331932279419,-1.,-3.93442567551042));
#38380=CARTESIAN_POINT('Ctrl Pts',(0.135827558661188,-1.,-3.94156445130741));
#38381=CARTESIAN_POINT('Ctrl Pts',(0.138383621255161,-1.,-3.94868667844347));
#38382=CARTESIAN_POINT('Ctrl Pts',(0.140986665829942,-1.,-3.95579014116894));
#38383=CARTESIAN_POINT('Ctrl Pts',(0.143635947692798,-1.,-3.96287658098896));
#38384=CARTESIAN_POINT('Ctrl Pts',(0.14633079781452,-1.,-3.96995018565893));
#38385=CARTESIAN_POINT('Ctrl Pts',(0.149070594803544,-1.,-3.97701581473644));
#38386=CARTESIAN_POINT('Ctrl Pts',(0.151854737441398,-1.,-3.98407729850975));
#38387=CARTESIAN_POINT('Ctrl Pts',(0.154682618338547,-1.,-3.99113582086043));
#38388=CARTESIAN_POINT('Ctrl Pts',(0.15755363438379,-1.,-3.9981907463185));
#38389=CARTESIAN_POINT('Ctrl Pts',(0.160467194882202,-1.,-4.00524031064487));
#38390=CARTESIAN_POINT('Ctrl Pts',(0.163422730287456,-1.,-4.01228237022296));
#38391=CARTESIAN_POINT('Ctrl Pts',(0.166419700015865,-1.,-4.01931510507167));
#38392=CARTESIAN_POINT('Ctrl Pts',(0.169457601001691,-1.,-4.02633779703764));
#38393=CARTESIAN_POINT('Ctrl Pts',(0.172535962484514,-1.,-4.03335057326163));
#38394=CARTESIAN_POINT('Ctrl Pts',(0.175654339673797,-1.,-4.04035407891222));
#38395=CARTESIAN_POINT('Ctrl Pts',(0.178812307240728,-1.,-4.04734916719741));
#38396=CARTESIAN_POINT('Ctrl Pts',(0.182009453048519,-1.,-4.05433660358353));
#38397=CARTESIAN_POINT('Ctrl Pts',(0.185245370038873,-1.,-4.06131670998469));
#38398=CARTESIAN_POINT('Ctrl Pts',(0.188519658060155,-1.,-4.06828941192147));
#38399=CARTESIAN_POINT('Ctrl Pts',(0.19183192818099,-1.,-4.07525439702992));
#38400=CARTESIAN_POINT('Ctrl Pts',(0.195181806054675,-1.,-4.08221124060322));
#38401=CARTESIAN_POINT('Ctrl Pts',(0.198568934800861,-1.,-4.08915953359833));
#38402=CARTESIAN_POINT('Ctrl Pts',(0.201992979050135,-1.,-4.09609903752152));
#38403=CARTESIAN_POINT('Ctrl Pts',(0.205453622198454,-1.,-4.10302969965728));
#38404=CARTESIAN_POINT('Ctrl Pts',(0.208950559400392,-1.,-4.10995157639377));
#38405=CARTESIAN_POINT('Ctrl Pts',(0.212483491087189,-1.,-4.11686478264739));
#38406=CARTESIAN_POINT('Ctrl Pts',(0.216052116898351,-1.,-4.12376943492132));
#38407=CARTESIAN_POINT('Ctrl Pts',(0.219656126701541,-1.,-4.13066558697658));
#38408=CARTESIAN_POINT('Ctrl Pts',(0.223295201037885,-1.,-4.13755320552764));
#38409=CARTESIAN_POINT('Ctrl Pts',(0.226969025060705,-1.,-4.14443220606869));
#38410=CARTESIAN_POINT('Ctrl Pts',(0.230677299028383,-1.,-4.15130247434459));
#38411=CARTESIAN_POINT('Ctrl Pts',(0.234419749543207,-1.,-4.15816389265352));
#38412=CARTESIAN_POINT('Ctrl Pts',(0.238196140934616,-1.,-4.16501636654877));
#38413=CARTESIAN_POINT('Ctrl Pts',(0.242006283925088,-1.,-4.17185984411426));
#38414=CARTESIAN_POINT('Ctrl Pts',(0.245850033420019,-1.,-4.1786943019518));
#38415=CARTESIAN_POINT('Ctrl Pts',(0.248951836912189,-1.,-4.18415464961466));
#38416=CARTESIAN_POINT('Ctrl Pts',(0.25129323983844,-1.,-4.18824585245272));
#38417=CARTESIAN_POINT('Ctrl Pts',(0.25286086157284,-1.,-4.19097151819684));
#38418=CARTESIAN_POINT('Ctrl Pts',(0.253646344052522,-1.,-4.1923339003649));
#38419=CARTESIAN_POINT('',(0.40530197431835,-1.,-4.18039834341342));
#38420=CARTESIAN_POINT('',(0.253646344052522,-1.,-4.1923339003649));
#38421=CARTESIAN_POINT('',(0.496319364827592,-1.,-3.71701050416825));
#38422=CARTESIAN_POINT('Ctrl Pts',(0.40530197431835,-1.,-4.18039834341342));
#38423=CARTESIAN_POINT('Ctrl Pts',(0.405864662679209,-1.,-4.17892985789466));
#38424=CARTESIAN_POINT('Ctrl Pts',(0.406986596325454,-1.,-4.17599251954382));
#38425=CARTESIAN_POINT('Ctrl Pts',(0.408659167568273,-1.,-4.17158541007977));
#38426=CARTESIAN_POINT('Ctrl Pts',(0.410868596146414,-1.,-4.16570705938425));
#38427=CARTESIAN_POINT('Ctrl Pts',(0.41359587795147,-1.,-4.15835545017202));
#38428=CARTESIAN_POINT('Ctrl Pts',(0.416288556008011,-1.,-4.15100018949965));
#38429=CARTESIAN_POINT('Ctrl Pts',(0.418946490667702,-1.,-4.14364132317121));
#38430=CARTESIAN_POINT('Ctrl Pts',(0.421569503104512,-1.,-4.13627893207002));
#38431=CARTESIAN_POINT('Ctrl Pts',(0.424157375323975,-1.,-4.12891314634572));
#38432=CARTESIAN_POINT('Ctrl Pts',(0.426709855707,-1.,-4.12154412502007));
#38433=CARTESIAN_POINT('Ctrl Pts',(0.429226666075844,-1.,-4.11417202783267));
#38434=CARTESIAN_POINT('Ctrl Pts',(0.431707508679883,-1.,-4.10679698750336));
#38435=CARTESIAN_POINT('Ctrl Pts',(0.43415207320046,-1.,-4.09941908688373));
#38436=CARTESIAN_POINT('Ctrl Pts',(0.436560044913482,-1.,-4.09203832139089));
#38437=CARTESIAN_POINT('Ctrl Pts',(0.438931108931279,-1.,-4.08465462294273));
#38438=CARTESIAN_POINT('Ctrl Pts',(0.44126495139636,-1.,-4.07726792490016));
#38439=CARTESIAN_POINT('Ctrl Pts',(0.443561262395332,-1.,-4.0698782192569));
#38440=CARTESIAN_POINT('Ctrl Pts',(0.445819737468537,-1.,-4.06248560760659));
#38441=CARTESIAN_POINT('Ctrl Pts',(0.448040082684114,-1.,-4.0550903779696));
#38442=CARTESIAN_POINT('Ctrl Pts',(0.450222009543926,-1.,-4.0476929901813));
#38443=CARTESIAN_POINT('Ctrl Pts',(0.452365214748892,-1.,-4.04029392228049));
#38444=CARTESIAN_POINT('Ctrl Pts',(0.454469363020541,-1.,-4.03289354362794));
#38445=CARTESIAN_POINT('Ctrl Pts',(0.45653407078495,-1.,-4.02549199038394));
#38446=CARTESIAN_POINT('Ctrl Pts',(0.458558885636945,-1.,-4.01808900827587));
#38447=CARTESIAN_POINT('Ctrl Pts',(0.460543280768514,-1.,-4.01068390573399));
#38448=CARTESIAN_POINT('Ctrl Pts',(0.462486702616204,-1.,-4.00327590659075));
#38449=CARTESIAN_POINT('Ctrl Pts',(0.464388610938975,-1.,-3.9958644432011));
#38450=CARTESIAN_POINT('Ctrl Pts',(0.466248520883039,-1.,-3.98844946363262));
#38451=CARTESIAN_POINT('Ctrl Pts',(0.468066047920157,-1.,-3.98103175589371));
#38452=CARTESIAN_POINT('Ctrl Pts',(0.469840942829895,-1.,-3.97361320212436));
#38453=CARTESIAN_POINT('Ctrl Pts',(0.471572978413503,-1.,-3.96619600864643));
#38454=CARTESIAN_POINT('Ctrl Pts',(0.473261847236297,-1.,-3.95878201038338));
#38455=CARTESIAN_POINT('Ctrl Pts',(0.47490705302179,-1.,-3.95137192932897));
#38456=CARTESIAN_POINT('Ctrl Pts',(0.476507810658537,-1.,-3.94396469119383));
#38457=CARTESIAN_POINT('Ctrl Pts',(0.478062927140964,-1.,-3.93655660689819));
#38458=CARTESIAN_POINT('Ctrl Pts',(0.479571028525578,-1.,-3.92914297392071));
#38459=CARTESIAN_POINT('Ctrl Pts',(0.481030798910748,-1.,-3.92171976072341));
#38460=CARTESIAN_POINT('Ctrl Pts',(0.482441230340713,-1.,-3.91428536373751));
#38461=CARTESIAN_POINT('Ctrl Pts',(0.48380183508915,-1.,-3.90684210358056));
#38462=CARTESIAN_POINT('Ctrl Pts',(0.485112963522222,-1.,-3.89939844658513));
#38463=CARTESIAN_POINT('Ctrl Pts',(0.486375337854103,-1.,-3.89196582437552));
#38464=CARTESIAN_POINT('Ctrl Pts',(0.487589452275154,-1.,-3.88455453328138));
#38465=CARTESIAN_POINT('Ctrl Pts',(0.488754973798273,-1.,-3.87716963231109));
#38466=CARTESIAN_POINT('Ctrl Pts',(0.489870245704917,-1.,-3.86980755613707));
#38467=CARTESIAN_POINT('Ctrl Pts',(0.490931482170891,-1.,-3.86245057319246));
#38468=CARTESIAN_POINT('Ctrl Pts',(0.491933631083813,-1.,-3.85507287020263));
#38469=CARTESIAN_POINT('Ctrl Pts',(0.49287179241414,-1.,-3.84765051147999));
#38470=CARTESIAN_POINT('Ctrl Pts',(0.493742574629134,-1.,-3.84017095578451));
#38471=CARTESIAN_POINT('Ctrl Pts',(0.494545212256401,-1.,-3.83264092682431));
#38472=CARTESIAN_POINT('Ctrl Pts',(0.495283458893837,-1.,-3.82509963594103));
#38473=CARTESIAN_POINT('Ctrl Pts',(0.495963937875479,-1.,-3.81760756144025));
#38474=CARTESIAN_POINT('Ctrl Pts',(0.496592643443704,-1.,-3.81022254090839));
#38475=CARTESIAN_POINT('Ctrl Pts',(0.497171756201051,-1.,-3.80297788298514));
#38476=CARTESIAN_POINT('Ctrl Pts',(0.497696892100624,-1.,-3.79586380669994));
#38477=CARTESIAN_POINT('Ctrl Pts',(0.498152751800958,-1.,-3.78879701661264));
#38478=CARTESIAN_POINT('Ctrl Pts',(0.498515471679584,-1.,-3.78163975337356));
#38479=CARTESIAN_POINT('Ctrl Pts',(0.498759900365891,-1.,-3.77425499225255));
#38480=CARTESIAN_POINT('Ctrl Pts',(0.49886579233529,-1.,-3.76655401191229));
#38481=CARTESIAN_POINT('Ctrl Pts',(0.498823681615421,-1.,-3.75854082221052));
#38482=CARTESIAN_POINT('Ctrl Pts',(0.498642802042605,-1.,-3.75037362167839));
#38483=CARTESIAN_POINT('Ctrl Pts',(0.498350586057692,-1.,-3.74235701734714));
#38484=CARTESIAN_POINT('Ctrl Pts',(0.497984209510024,-1.,-3.73486914372449));
#38485=CARTESIAN_POINT('Ctrl Pts',(0.497584067153049,-1.,-3.72830430904606));
#38486=CARTESIAN_POINT('Ctrl Pts',(0.497187079575988,-1.,-3.72301489774398));
#38487=CARTESIAN_POINT('Ctrl Pts',(0.496846224822563,-1.,-3.71952320822499));
#38488=CARTESIAN_POINT('Ctrl Pts',(0.496605651525989,-1.,-3.71785517607549));
#38489=CARTESIAN_POINT('Ctrl Pts',(0.496446644158005,-1.,-3.71721917030355));
#38490=CARTESIAN_POINT('Ctrl Pts',(0.496354087924312,-1.,-3.71704500630495));
#38491=CARTESIAN_POINT('Ctrl Pts',(0.496319364827592,-1.,-3.71701050416825));
#38492=CARTESIAN_POINT('',(0.676591647973661,-1.,-3.68845817949618));
#38493=CARTESIAN_POINT('Origin',(0.,-1.,0.));
#38494=CARTESIAN_POINT('',(0.906349047628866,-1.,-4.10104028313088));
#38495=CARTESIAN_POINT('Ctrl Pts',(0.676591647973661,-1.,-3.68845817949618));
#38496=CARTESIAN_POINT('Ctrl Pts',(0.67656928609342,-1.,-3.68850172300543));
#38497=CARTESIAN_POINT('Ctrl Pts',(0.676535079520365,-1.,-3.68869596426099));
#38498=CARTESIAN_POINT('Ctrl Pts',(0.676580391119535,-1.,-3.68934997767391));
#38499=CARTESIAN_POINT('Ctrl Pts',(0.676867042599711,-1.,-3.6910107117555));
#38500=CARTESIAN_POINT('Ctrl Pts',(0.677621861865196,-1.,-3.69443683573443));
#38501=CARTESIAN_POINT('Ctrl Pts',(0.678878822226389,-1.,-3.69959004073192));
#38502=CARTESIAN_POINT('Ctrl Pts',(0.680526909711617,-1.,-3.70595722032165));
#38503=CARTESIAN_POINT('Ctrl Pts',(0.682492345109689,-1.,-3.71319182790334));
#38504=CARTESIAN_POINT('Ctrl Pts',(0.684691698168355,-1.,-3.7209063713952));
#38505=CARTESIAN_POINT('Ctrl Pts',(0.687043475232499,-1.,-3.72872973554125));
#38506=CARTESIAN_POINT('Ctrl Pts',(0.689479637354651,-1.,-3.73636374474993));
#38507=CARTESIAN_POINT('Ctrl Pts',(0.691960080400503,-1.,-3.74365508986548));
#38508=CARTESIAN_POINT('Ctrl Pts',(0.694474562581173,-1.,-3.7506028824329));
#38509=CARTESIAN_POINT('Ctrl Pts',(0.69703124565953,-1.,-3.75729775766913));
#38510=CARTESIAN_POINT('Ctrl Pts',(0.699648552230851,-1.,-3.76387780603725));
#38511=CARTESIAN_POINT('Ctrl Pts',(0.702346356621613,-1.,-3.77048141872904));
#38512=CARTESIAN_POINT('Ctrl Pts',(0.705135847999949,-1.,-3.77719254217197));
#38513=CARTESIAN_POINT('Ctrl Pts',(0.7080158793756,-1.,-3.78402183336678));
#38514=CARTESIAN_POINT('Ctrl Pts',(0.710978231689117,-1.,-3.79093694007146));
#38515=CARTESIAN_POINT('Ctrl Pts',(0.714010733006677,-1.,-3.79788100314994));
#38516=CARTESIAN_POINT('Ctrl Pts',(0.717100993669091,-1.,-3.80479445759296));
#38517=CARTESIAN_POINT('Ctrl Pts',(0.720240466589172,-1.,-3.81163885127309));
#38518=CARTESIAN_POINT('Ctrl Pts',(0.723426346019349,-1.,-3.81840802610795));
#38519=CARTESIAN_POINT('Ctrl Pts',(0.726659281876608,-1.,-3.82511495756682));
#38520=CARTESIAN_POINT('Ctrl Pts',(0.729942010490145,-1.,-3.83178392403371));
#38521=CARTESIAN_POINT('Ctrl Pts',(0.73327770375609,-1.,-3.83844103658016));
#38522=CARTESIAN_POINT('Ctrl Pts',(0.736668240497151,-1.,-3.84510432881231));
#38523=CARTESIAN_POINT('Ctrl Pts',(0.740113146827176,-1.,-3.85177770351237));
#38524=CARTESIAN_POINT('Ctrl Pts',(0.743610542737041,-1.,-3.85845645217611));
#38525=CARTESIAN_POINT('Ctrl Pts',(0.747157716488884,-1.,-3.86513062969896));
#38526=CARTESIAN_POINT('Ctrl Pts',(0.750751822383023,-1.,-3.87178914078372));
#38527=CARTESIAN_POINT('Ctrl Pts',(0.754390577396846,-1.,-3.87842382520058));
#38528=CARTESIAN_POINT('Ctrl Pts',(0.758072800564798,-1.,-3.88503262662684));
#38529=CARTESIAN_POINT('Ctrl Pts',(0.761798028793978,-1.,-3.89161738162245));
#38530=CARTESIAN_POINT('Ctrl Pts',(0.765566256401306,-1.,-3.89818233104381));
#38531=CARTESIAN_POINT('Ctrl Pts',(0.769377629847876,-1.,-3.90473237182634));
#38532=CARTESIAN_POINT('Ctrl Pts',(0.773232154506305,-1.,-3.91127138115238));
#38533=CARTESIAN_POINT('Ctrl Pts',(0.777129415664915,-1.,-3.91780062334464));
#38534=CARTESIAN_POINT('Ctrl Pts',(0.781068718228395,-1.,-3.92431956510418));
#38535=CARTESIAN_POINT('Ctrl Pts',(0.785049202786458,-1.,-3.93082655631769));
#38536=CARTESIAN_POINT('Ctrl Pts',(0.789069971469323,-1.,-3.93731956885671));
#38537=CARTESIAN_POINT('Ctrl Pts',(0.793130205641017,-1.,-3.94379688971307));
#38538=CARTESIAN_POINT('Ctrl Pts',(0.797229296085438,-1.,-3.95025788827189));
#38539=CARTESIAN_POINT('Ctrl Pts',(0.801366797727206,-1.,-3.95670276375176));
#38540=CARTESIAN_POINT('Ctrl Pts',(0.805542372178495,-1.,-3.96313222295874));
#38541=CARTESIAN_POINT('Ctrl Pts',(0.809755732818134,-1.,-3.96954717513251));
#38542=CARTESIAN_POINT('Ctrl Pts',(0.814006592328737,-1.,-3.97594844078763));
#38543=CARTESIAN_POINT('Ctrl Pts',(0.818294599022033,-1.,-3.98233640155287));
#38544=CARTESIAN_POINT('Ctrl Pts',(0.822619346021769,-1.,-3.98871104646328));
#38545=CARTESIAN_POINT('Ctrl Pts',(0.826980400320473,-1.,-3.99507212784289));
#38546=CARTESIAN_POINT('Ctrl Pts',(0.831377325741487,-1.,-4.00141928477447));
#38547=CARTESIAN_POINT('Ctrl Pts',(0.835809705809821,-1.,-4.00775216907934));
#38548=CARTESIAN_POINT('Ctrl Pts',(0.84027717197638,-1.,-4.01407059766338));
#38549=CARTESIAN_POINT('Ctrl Pts',(0.844779403288517,-1.,-4.02037456798787));
#38550=CARTESIAN_POINT('Ctrl Pts',(0.849316107475012,-1.,-4.02666418343508));
#38551=CARTESIAN_POINT('Ctrl Pts',(0.853887006632178,-1.,-4.03293960436946));
#38552=CARTESIAN_POINT('Ctrl Pts',(0.858491822322571,-1.,-4.03920099284658));
#38553=CARTESIAN_POINT('Ctrl Pts',(0.863130256642173,-1.,-4.04544845048097));
#38554=CARTESIAN_POINT('Ctrl Pts',(0.867801988858176,-1.,-4.05168199437128));
#38555=CARTESIAN_POINT('Ctrl Pts',(0.872506694780563,-1.,-4.05790159030495));
#38556=CARTESIAN_POINT('Ctrl Pts',(0.877244060484595,-1.,-4.06410717232347));
#38557=CARTESIAN_POINT('Ctrl Pts',(0.882013797525916,-1.,-4.07029866694292));
#38558=CARTESIAN_POINT('Ctrl Pts',(0.886815658360739,-1.,-4.07647601774639));
#38559=CARTESIAN_POINT('Ctrl Pts',(0.891649447920401,-1.,-4.08263920306651));
#38560=CARTESIAN_POINT('Ctrl Pts',(0.896515019236368,-1.,-4.08878822249095));
#38561=CARTESIAN_POINT('Ctrl Pts',(0.900432820945975,-1.,-4.09369611524319));
#38562=CARTESIAN_POINT('Ctrl Pts',(0.903385402444212,-1.,-4.09737067247114));
#38563=CARTESIAN_POINT('Ctrl Pts',(0.905360112216302,-1.,-4.09981755067956));
#38564=CARTESIAN_POINT('Ctrl Pts',(0.906349047628866,-1.,-4.10104028313088));
#38565=CARTESIAN_POINT('',(1.05427041296137,-1.,-4.06552750530042));
#38566=CARTESIAN_POINT('',(0.906349047628866,-1.,-4.10104028313088));
#38567=CARTESIAN_POINT('',(1.07167739962028,-1.,-3.59360648251073));
#38568=CARTESIAN_POINT('Ctrl Pts',(1.05427041296137,-1.,-4.06552750530042));
#38569=CARTESIAN_POINT('Ctrl Pts',(1.05459645194823,-1.,-4.06398907542249));
#38570=CARTESIAN_POINT('Ctrl Pts',(1.05524507177599,-1.,-4.06091239149123));
#38571=CARTESIAN_POINT('Ctrl Pts',(1.05620762707996,-1.,-4.05629789307025));
#38572=CARTESIAN_POINT('Ctrl Pts',(1.05747027727959,-1.,-4.05014628384869));
#38573=CARTESIAN_POINT('Ctrl Pts',(1.05901393666566,-1.,-4.04245854427496));
#38574=CARTESIAN_POINT('Ctrl Pts',(1.06052284711857,-1.,-4.03477261141553));
#38575=CARTESIAN_POINT('Ctrl Pts',(1.06199687787462,-1.,-4.02708855235633));
#38576=CARTESIAN_POINT('Ctrl Pts',(1.06343586496236,-1.,-4.01940647495943));
#38577=CARTESIAN_POINT('Ctrl Pts',(1.06483961343109,-1.,-4.01172654187398));
#38578=CARTESIAN_POINT('Ctrl Pts',(1.06620789963606,-1.,-4.00404894952579));
#38579=CARTESIAN_POINT('Ctrl Pts',(1.06754047381312,-1.,-3.99637389920441));
#38580=CARTESIAN_POINT('Ctrl Pts',(1.06883706263941,-1.,-3.98870156857412));
#38581=CARTESIAN_POINT('Ctrl Pts',(1.07009737257767,-1.,-3.98103208801101));
#38582=CARTESIAN_POINT('Ctrl Pts',(1.07132109206164,-1.,-3.9733655022223));
#38583=CARTESIAN_POINT('Ctrl Pts',(1.07250789943007,-1.,-3.96570179322338));
#38584=CARTESIAN_POINT('Ctrl Pts',(1.07365747426491,-1.,-3.95804094429373));
#38585=CARTESIAN_POINT('Ctrl Pts',(1.07476950921587,-1.,-3.95038299600676));
#38586=CARTESIAN_POINT('Ctrl Pts',(1.07584371946443,-1.,-3.94272809633331));
#38587=CARTESIAN_POINT('Ctrl Pts',(1.07687985975384,-1.,-3.93507657572883));
#38588=CARTESIAN_POINT('Ctrl Pts',(1.07787771707195,-1.,-3.9274289334984));
#38589=CARTESIAN_POINT('Ctrl Pts',(1.07883706663554,-1.,-3.91978568924178));
#38590=CARTESIAN_POINT('Ctrl Pts',(1.07975763507473,-1.,-3.91214726022143));
#38591=CARTESIAN_POINT('Ctrl Pts',(1.08063906483818,-1.,-3.90451384092545));
#38592=CARTESIAN_POINT('Ctrl Pts',(1.08148086931358,-1.,-3.8968852509835));
#38593=CARTESIAN_POINT('Ctrl Pts',(1.08228241999346,-1.,-3.88926088975114));
#38594=CARTESIAN_POINT('Ctrl Pts',(1.08304304871028,-1.,-3.88164007721313));
#38595=CARTESIAN_POINT('Ctrl Pts',(1.08376213307504,-1.,-3.8740223372254));
#38596=CARTESIAN_POINT('Ctrl Pts',(1.08443918607927,-1.,-3.86640769434274));
#38597=CARTESIAN_POINT('Ctrl Pts',(1.08507395120059,-1.,-3.85879698702532));
#38598=CARTESIAN_POINT('Ctrl Pts',(1.08566647671844,-1.,-3.85119211322755));
#38599=CARTESIAN_POINT('Ctrl Pts',(1.08621688337604,-1.,-3.8435952876495));
#38600=CARTESIAN_POINT('Ctrl Pts',(1.08672515456902,-1.,-3.83600837071708));
#38601=CARTESIAN_POINT('Ctrl Pts',(1.08719091307558,-1.,-3.82843215316984));
#38602=CARTESIAN_POINT('Ctrl Pts',(1.08761321539442,-1.,-3.82086569676319));
#38603=CARTESIAN_POINT('Ctrl Pts',(1.08799030610862,-1.,-3.81330554446323));
#38604=CARTESIAN_POINT('Ctrl Pts',(1.0883200925538,-1.,-3.8057472665766));
#38605=CARTESIAN_POINT('Ctrl Pts',(1.08860064435778,-1.,-3.79818708705259));
#38606=CARTESIAN_POINT('Ctrl Pts',(1.08883071512098,-1.,-3.79062357974404));
#38607=CARTESIAN_POINT('Ctrl Pts',(1.08901018614636,-1.,-3.78305911299504));
#38608=CARTESIAN_POINT('Ctrl Pts',(1.0891407279127,-1.,-3.77550199409424));
#38609=CARTESIAN_POINT('Ctrl Pts',(1.08922484204256,-1.,-3.76796340094448));
#38610=CARTESIAN_POINT('Ctrl Pts',(1.08926462734281,-1.,-3.76045342580208));
#38611=CARTESIAN_POINT('Ctrl Pts',(1.08926054632925,-1.,-3.75297711748132));
#38612=CARTESIAN_POINT('Ctrl Pts',(1.08921040494017,-1.,-3.74553121371757));
#38613=CARTESIAN_POINT('Ctrl Pts',(1.08910769013297,-1.,-3.73809879348239));
#38614=CARTESIAN_POINT('Ctrl Pts',(1.08894337390937,-1.,-3.73065515162988));
#38615=CARTESIAN_POINT('Ctrl Pts',(1.08870887220082,-1.,-3.72317741369398));
#38616=CARTESIAN_POINT('Ctrl Pts',(1.0883988733478,-1.,-3.71565372339075));
#38617=CARTESIAN_POINT('Ctrl Pts',(1.08801367312185,-1.,-3.70809084139457));
#38618=CARTESIAN_POINT('Ctrl Pts',(1.08756311291309,-1.,-3.70052690909833));
#38619=CARTESIAN_POINT('Ctrl Pts',(1.08706319540271,-1.,-3.69302062410157));
#38620=CARTESIAN_POINT('Ctrl Pts',(1.0865288888259,-1.,-3.68562817420797));
#38621=CARTESIAN_POINT('Ctrl Pts',(1.0859675575576,-1.,-3.67838211685118));
#38622=CARTESIAN_POINT('Ctrl Pts',(1.0853733414449,-1.,-3.67127347729666));
#38623=CARTESIAN_POINT('Ctrl Pts',(1.08471809922901,-1.,-3.66422237895365));
#38624=CARTESIAN_POINT('Ctrl Pts',(1.08395671077807,-1.,-3.65709649161166));
#38625=CARTESIAN_POINT('Ctrl Pts',(1.08304289898623,-1.,-3.64976441208358));
#38626=CARTESIAN_POINT('Ctrl Pts',(1.08194278850996,-1.,-3.64214167843677));
#38627=CARTESIAN_POINT('Ctrl Pts',(1.08064765719867,-1.,-3.63423373196529));
#38628=CARTESIAN_POINT('Ctrl Pts',(1.07919137290742,-1.,-3.62619537902361));
#38629=CARTESIAN_POINT('Ctrl Pts',(1.07764868137619,-1.,-3.61832318504575));
#38630=CARTESIAN_POINT('Ctrl Pts',(1.07611545402734,-1.,-3.61098481349204));
#38631=CARTESIAN_POINT('Ctrl Pts',(1.07469327168578,-1.,-3.60456339887778));
#38632=CARTESIAN_POINT('Ctrl Pts',(1.07347372545714,-1.,-3.59940121154535));
#38633=CARTESIAN_POINT('Ctrl Pts',(1.07259084660935,-1.,-3.59600583194946));
#38634=CARTESIAN_POINT('Ctrl Pts',(1.07209229745229,-1.,-3.59439596999862));
#38635=CARTESIAN_POINT('Ctrl Pts',(1.07183575450617,-1.,-3.59379266874567));
#38636=CARTESIAN_POINT('Ctrl Pts',(1.07171709254135,-1.,-3.5936351279798));
#38637=CARTESIAN_POINT('Ctrl Pts',(1.07167739962028,-1.,-3.59360648251073));
#38638=CARTESIAN_POINT('',(1.24526366418038,-1.,-3.5372048861597));
#38639=CARTESIAN_POINT('Origin',(0.,-1.,0.));
#38640=CARTESIAN_POINT('',(1.53673442965256,-1.,-3.90876544355381));
#38641=CARTESIAN_POINT('Ctrl Pts',(1.24526366418038,-1.,-3.5372048861597));
#38642=CARTESIAN_POINT('Ctrl Pts',(1.24524838931757,-1.,-3.53725139174486));
#38643=CARTESIAN_POINT('Ctrl Pts',(1.2452449899111,-1.,-3.5374485926552));
#38644=CARTESIAN_POINT('Ctrl Pts',(1.24539205388767,-1.,-3.53808746578196));
#38645=CARTESIAN_POINT('Ctrl Pts',(1.24593497226008,-1.,-3.53968291130022));
#38646=CARTESIAN_POINT('Ctrl Pts',(1.24721646231966,-1.,-3.54294877425964));
#38647=CARTESIAN_POINT('Ctrl Pts',(1.24926408628003,-1.,-3.54784190283068));
#38648=CARTESIAN_POINT('Ctrl Pts',(1.2518879294064,-1.,-3.55387287418985));
#38649=CARTESIAN_POINT('Ctrl Pts',(1.25496090900009,-1.,-3.56071094991199));
#38650=CARTESIAN_POINT('Ctrl Pts',(1.25834000485716,-1.,-3.56798645995275));
#38651=CARTESIAN_POINT('Ctrl Pts',(1.2618866714281,-1.,-3.5753456065171));
#38652=CARTESIAN_POINT('Ctrl Pts',(1.26548706249862,-1.,-3.58250452868618));
#38653=CARTESIAN_POINT('Ctrl Pts',(1.26907758484709,-1.,-3.58931807846313));
#38654=CARTESIAN_POINT('Ctrl Pts',(1.27264798379307,-1.,-3.59578698050006));
#38655=CARTESIAN_POINT('Ctrl Pts',(1.27622049908625,-1.,-3.60199947736298));
#38656=CARTESIAN_POINT('Ctrl Pts',(1.27983492861691,-1.,-3.60808907746339));
#38657=CARTESIAN_POINT('Ctrl Pts',(1.28353255117765,-1.,-3.61418935913823));
#38658=CARTESIAN_POINT('Ctrl Pts',(1.28733755029384,-1.,-3.6203814849236));
#38659=CARTESIAN_POINT('Ctrl Pts',(1.29125046021878,-1.,-3.62667616004369));
#38660=CARTESIAN_POINT('Ctrl Pts',(1.29525810207762,-1.,-3.63304271631046));
#38661=CARTESIAN_POINT('Ctrl Pts',(1.2993395590647,-1.,-3.63942689872808));
#38662=CARTESIAN_POINT('Ctrl Pts',(1.30347327603774,-1.,-3.64577181380113));
#38663=CARTESIAN_POINT('Ctrl Pts',(1.30764479590039,-1.,-3.65204081987068));
#38664=CARTESIAN_POINT('Ctrl Pts',(1.31185038411218,-1.,-3.65822827358617));
#38665=CARTESIAN_POINT('Ctrl Pts',(1.31609271239911,-1.,-3.66434688899793));
#38666=CARTESIAN_POINT('Ctrl Pts',(1.32037828137766,-1.,-3.67042021752656));
#38667=CARTESIAN_POINT('Ctrl Pts',(1.32471430856415,-1.,-3.67647355257912));
#38668=CARTESIAN_POINT('Ctrl Pts',(1.3291054707274,-1.,-3.68252441182551));
#38669=CARTESIAN_POINT('Ctrl Pts',(1.33355191034523,-1.,-3.68857672413033));
#38670=CARTESIAN_POINT('Ctrl Pts',(1.33805103398219,-1.,-3.69462613305708));
#38671=CARTESIAN_POINT('Ctrl Pts',(1.34259860752933,-1.,-3.70066324015119));
#38672=CARTESIAN_POINT('Ctrl Pts',(1.34719008463534,-1.,-3.70667753188248));
#38673=CARTESIAN_POINT('Ctrl Pts',(1.35182193384424,-1.,-3.71266130563054));
#38674=CARTESIAN_POINT('Ctrl Pts',(1.35649266705037,-1.,-3.71861271513313));
#38675=CARTESIAN_POINT('Ctrl Pts',(1.36120211416354,-1.,-3.72453364678279));
#38676=CARTESIAN_POINT('Ctrl Pts',(1.36595093298676,-1.,-3.73042829011295));
#38677=CARTESIAN_POINT('Ctrl Pts',(1.37074003422739,-1.,-3.7363014588581));
#38678=CARTESIAN_POINT('Ctrl Pts',(1.37557002971687,-1.,-3.74215698162555));
#38679=CARTESIAN_POINT('Ctrl Pts',(1.38044070763295,-1.,-3.74799617204729));
#38680=CARTESIAN_POINT('Ctrl Pts',(1.38535129801176,-1.,-3.75381861212707));
#38681=CARTESIAN_POINT('Ctrl Pts',(1.39030069388918,-1.,-3.75962280650855));
#38682=CARTESIAN_POINT('Ctrl Pts',(1.39528769118052,-1.,-3.76540689249074));
#38683=CARTESIAN_POINT('Ctrl Pts',(1.40031121335505,-1.,-3.77116930621827));
#38684=CARTESIAN_POINT('Ctrl Pts',(1.40537056004722,-1.,-3.77690952014259));
#38685=CARTESIAN_POINT('Ctrl Pts',(1.41046532282593,-1.,-3.78262780065471));
#38686=CARTESIAN_POINT('Ctrl Pts',(1.4155952780383,-1.,-3.78832489879426));
#38687=CARTESIAN_POINT('Ctrl Pts',(1.42076028482836,-1.,-3.79400175744408));
#38688=CARTESIAN_POINT('Ctrl Pts',(1.42596018777283,-1.,-3.7996592319632));
#38689=CARTESIAN_POINT('Ctrl Pts',(1.4311946992132,-1.,-3.80529775429805));
#38690=CARTESIAN_POINT('Ctrl Pts',(1.43646341556724,-1.,-3.81091737726815));
#38691=CARTESIAN_POINT('Ctrl Pts',(1.44176587041347,-1.,-3.81651792398414));
#38692=CARTESIAN_POINT('Ctrl Pts',(1.44710157648539,-1.,-3.82209910620533));
#38693=CARTESIAN_POINT('Ctrl Pts',(1.45247006796836,-1.,-3.82766064519075));
#38694=CARTESIAN_POINT('Ctrl Pts',(1.45787095220852,-1.,-3.83320241775423));
#38695=CARTESIAN_POINT('Ctrl Pts',(1.46330391180752,-1.,-3.83872447159639));
#38696=CARTESIAN_POINT('Ctrl Pts',(1.46876867426504,-1.,-3.84422695454796));
#38697=CARTESIAN_POINT('Ctrl Pts',(1.47426499018538,-1.,-3.84971006847277));
#38698=CARTESIAN_POINT('Ctrl Pts',(1.4797926099102,-1.,-3.85517401698843));
#38699=CARTESIAN_POINT('Ctrl Pts',(1.48535125509919,-1.,-3.86061894706087));
#38700=CARTESIAN_POINT('Ctrl Pts',(1.4909406116431,-1.,-3.86604492575189));
#38701=CARTESIAN_POINT('Ctrl Pts',(1.49656035399122,-1.,-3.87145196998465));
#38702=CARTESIAN_POINT('Ctrl Pts',(1.50221016176556,-1.,-3.87684006372134));
#38703=CARTESIAN_POINT('Ctrl Pts',(1.50788973857757,-1.,-3.88220917950538));
#38704=CARTESIAN_POINT('Ctrl Pts',(1.51359883110559,-1.,-3.88755930033884));
#38705=CARTESIAN_POINT('Ctrl Pts',(1.51933724329305,-1.,-3.89289043533657));
#38706=CARTESIAN_POINT('Ctrl Pts',(1.52510482991635,-1.,-3.89820260708225));
#38707=CARTESIAN_POINT('Ctrl Pts',(1.52974216056287,-1.,-3.90243719631596));
#38708=CARTESIAN_POINT('Ctrl Pts',(1.53323321827755,-1.,-3.90560462813969));
#38709=CARTESIAN_POINT('Ctrl Pts',(1.53556639217905,-1.,-3.90771246855019));
#38710=CARTESIAN_POINT('Ctrl Pts',(1.53673442965256,-1.,-3.90876544355381));
#38711=CARTESIAN_POINT('',(1.67727921511438,-1.,-3.85054988729471));
#38712=CARTESIAN_POINT('',(1.53673442965256,-1.,-3.90876544355381));
#38713=CARTESIAN_POINT('',(1.62064718014093,-1.,-3.38171594275765));
#38714=CARTESIAN_POINT('Ctrl Pts',(1.67727921511438,-1.,-3.85054988729471));
#38715=CARTESIAN_POINT('Ctrl Pts',(1.67736057656533,-1.,-3.84897939430696));
#38716=CARTESIAN_POINT('Ctrl Pts',(1.6775199114018,-1.,-3.84583912296459));
#38717=CARTESIAN_POINT('Ctrl Pts',(1.67774874946079,-1.,-3.84113085985244));
#38718=CARTESIAN_POINT('Ctrl Pts',(1.67803353064351,-1.,-3.8348574651399));
#38719=CARTESIAN_POINT('Ctrl Pts',(1.6783555575934,-1.,-3.82702289286713));
#38720=CARTESIAN_POINT('Ctrl Pts',(1.67864354605954,-1.,-3.81919554099578));
#38721=CARTESIAN_POINT('Ctrl Pts',(1.6788973773827,-1.,-3.81137549624179));
#38722=CARTESIAN_POINT('Ctrl Pts',(1.67911690648355,-1.,-3.80356289079005));
#38723=CARTESIAN_POINT('Ctrl Pts',(1.67930196625548,-1.,-3.79575791578424));
#38724=CARTESIAN_POINT('Ctrl Pts',(1.67945236653493,-1.,-3.7879608002176));
#38725=CARTESIAN_POINT('Ctrl Pts',(1.67956789212141,-1.,-3.78017178197317));
#38726=CARTESIAN_POINT('Ctrl Pts',(1.67964830084993,-1.,-3.77239107928502));
#38727=CARTESIAN_POINT('Ctrl Pts',(1.67969332319245,-1.,-3.76461886684344));
#38728=CARTESIAN_POINT('Ctrl Pts',(1.67970265841239,-1.,-3.75685523754493));
#38729=CARTESIAN_POINT('Ctrl Pts',(1.67967598599525,-1.,-3.7491002239452));
#38730=CARTESIAN_POINT('Ctrl Pts',(1.6796129868522,-1.,-3.74135385965401));
#38731=CARTESIAN_POINT('Ctrl Pts',(1.67951336376402,-1.,-3.73361623282543));
#38732=CARTESIAN_POINT('Ctrl Pts',(1.67937685856652,-1.,-3.72588753416396));
#38733=CARTESIAN_POINT('Ctrl Pts',(1.67920328071708,-1.,-3.71816812842322));
#38734=CARTESIAN_POINT('Ctrl Pts',(1.67899249793462,-1.,-3.71045854208343));
#38735=CARTESIAN_POINT('Ctrl Pts',(1.67874436948667,-1.,-3.70275932351108));
#38736=CARTESIAN_POINT('Ctrl Pts',(1.67845869064323,-1.,-3.6950709275959));
#38737=CARTESIAN_POINT('Ctrl Pts',(1.67813513867965,-1.,-3.68739360236487));
#38738=CARTESIAN_POINT('Ctrl Pts',(1.67777320475848,-1.,-3.67972724579124));
#38739=CARTESIAN_POINT('Ctrl Pts',(1.67737217414874,-1.,-3.67207136294575));
#38740=CARTESIAN_POINT('Ctrl Pts',(1.67693128053132,-1.,-3.66442538670968));
#38741=CARTESIAN_POINT('Ctrl Pts',(1.67644983469449,-1.,-3.6567889441642));
#38742=CARTESIAN_POINT('Ctrl Pts',(1.67592735946692,-1.,-3.64916213574667));
#38743=CARTESIAN_POINT('Ctrl Pts',(1.67536373264848,-1.,-3.6415458297234));
#38744=CARTESIAN_POINT('Ctrl Pts',(1.67475929882971,-1.,-3.63394189312924));
#38745=CARTESIAN_POINT('Ctrl Pts',(1.67411452372271,-1.,-3.62635249450923));
#38746=CARTESIAN_POINT('Ctrl Pts',(1.67342968196224,-1.,-3.61877947398184));
#38747=CARTESIAN_POINT('Ctrl Pts',(1.67270452466968,-1.,-3.61122367156181));
#38748=CARTESIAN_POINT('Ctrl Pts',(1.67193797318597,-1.,-3.60368430815201));
#38749=CARTESIAN_POINT('Ctrl Pts',(1.67112775290707,-1.,-3.59615824388807));
#38750=CARTESIAN_POINT('Ctrl Pts',(1.67027110397604,-1.,-3.58864143097834));
#38751=CARTESIAN_POINT('Ctrl Pts',(1.66936552908232,-1.,-3.58113044183829));
#38752=CARTESIAN_POINT('Ctrl Pts',(1.668409574073,-1.,-3.57362406285887));
#38753=CARTESIAN_POINT('Ctrl Pts',(1.66740349220305,-1.,-3.56612465179422));
#38754=CARTESIAN_POINT('Ctrl Pts',(1.66635023293114,-1.,-3.55864015233602));
#38755=CARTESIAN_POINT('Ctrl Pts',(1.66525401568994,-1.,-3.55118121342861));
#38756=CARTESIAN_POINT('Ctrl Pts',(1.66411849222326,-1.,-3.54375747475014));
#38757=CARTESIAN_POINT('Ctrl Pts',(1.66294490916111,-1.,-3.5363738506022));
#38758=CARTESIAN_POINT('Ctrl Pts',(1.66173058912371,-1.,-3.52902746211093));
#38759=CARTESIAN_POINT('Ctrl Pts',(1.66046645222279,-1.,-3.52170261543816));
#38760=CARTESIAN_POINT('Ctrl Pts',(1.65913971687342,-1.,-3.5143763218894));
#38761=CARTESIAN_POINT('Ctrl Pts',(1.65773832633632,-1.,-3.50702733146542));
#38762=CARTESIAN_POINT('Ctrl Pts',(1.65625517961588,-1.,-3.4996447647794));
#38763=CARTESIAN_POINT('Ctrl Pts',(1.65469162644468,-1.,-3.49223525300176));
#38764=CARTESIAN_POINT('Ctrl Pts',(1.65306335367739,-1.,-3.48483492840894));
#38765=CARTESIAN_POINT('Ctrl Pts',(1.65139534930322,-1.,-3.47749926256476));
#38766=CARTESIAN_POINT('Ctrl Pts',(1.64971118698256,-1.,-3.47028140995992));
#38767=CARTESIAN_POINT('Ctrl Pts',(1.64802323352738,-1.,-3.46321237515));
#38768=CARTESIAN_POINT('Ctrl Pts',(1.64632429697521,-1.,-3.45628421062422));
#38769=CARTESIAN_POINT('Ctrl Pts',(1.64457408708107,-1.,-3.44942242546795));
#38770=CARTESIAN_POINT('Ctrl Pts',(1.64270733821113,-1.,-3.44250337701888));
#38771=CARTESIAN_POINT('Ctrl Pts',(1.64065778702023,-1.,-3.43540451921548));
#38772=CARTESIAN_POINT('Ctrl Pts',(1.63837876246926,-1.,-3.42804772926291));
#38773=CARTESIAN_POINT('Ctrl Pts',(1.63586250099773,-1.,-3.42043974590882));
#38774=CARTESIAN_POINT('Ctrl Pts',(1.63316667054044,-1.,-3.41272817148478));
#38775=CARTESIAN_POINT('Ctrl Pts',(1.63041148964828,-1.,-3.40519422740235));
#38776=CARTESIAN_POINT('Ctrl Pts',(1.62774916464408,-1.,-3.39818605297991));
#38777=CARTESIAN_POINT('Ctrl Pts',(1.62533996116713,-1.,-3.39206617496906));
#38778=CARTESIAN_POINT('Ctrl Pts',(1.6233278855625,-1.,-3.38715832179072));
#38779=CARTESIAN_POINT('Ctrl Pts',(1.62192472202769,-1.,-3.38394285763222));
#38780=CARTESIAN_POINT('Ctrl Pts',(1.62118047294498,-1.,-3.38243080602408));
#38781=CARTESIAN_POINT('Ctrl Pts',(1.62083271135947,-1.,-3.38187506456922));
#38782=CARTESIAN_POINT('Ctrl Pts',(1.62069086551492,-1.,-3.38173802621259));
#38783=CARTESIAN_POINT('Ctrl Pts',(1.62064718014093,-1.,-3.38171594275765));
#38784=CARTESIAN_POINT('',(1.78327315618183,-1.,-3.29885386921599));
#38785=CARTESIAN_POINT('Origin',(0.,-1.,0.));
#38786=CARTESIAN_POINT('',(2.12928030988903,-1.,-3.62024382630768));
#38787=CARTESIAN_POINT('Ctrl Pts',(1.78327315618183,-1.,-3.29885386921599));
#38788=CARTESIAN_POINT('Ctrl Pts',(1.78326534445426,-1.,-3.29890219175522));
#38789=CARTESIAN_POINT('Ctrl Pts',(1.78329283591903,-1.,-3.29909749657945));
#38790=CARTESIAN_POINT('Ctrl Pts',(1.78353803106983,-1.,-3.29970549824337));
#38791=CARTESIAN_POINT('Ctrl Pts',(1.7843238478823,-1.,-3.30119637003466));
#38792=CARTESIAN_POINT('Ctrl Pts',(1.78610045419769,-1.,-3.30422155558973));
#38793=CARTESIAN_POINT('Ctrl Pts',(1.78888832245965,-1.,-3.30873412266954));
#38794=CARTESIAN_POINT('Ctrl Pts',(1.79242331350137,-1.,-3.31428038326763));
#38795=CARTESIAN_POINT('Ctrl Pts',(1.79652817033444,-1.,-3.32055355101168));
#38796=CARTESIAN_POINT('Ctrl Pts',(1.80100380443535,-1.,-3.3272108803981));
#38797=CARTESIAN_POINT('Ctrl Pts',(1.80565802981138,-1.,-3.33392460276874));
#38798=CARTESIAN_POINT('Ctrl Pts',(1.81033399625311,-1.,-3.34043216147532));
#38799=CARTESIAN_POINT('Ctrl Pts',(1.81494618732772,-1.,-3.34660014370527));
#38800=CARTESIAN_POINT('Ctrl Pts',(1.81948458796748,-1.,-3.35243086937451));
#38801=CARTESIAN_POINT('Ctrl Pts',(1.82398496829247,-1.,-3.35800801557326));
#38802=CARTESIAN_POINT('Ctrl Pts',(1.82850752153182,-1.,-3.36345722124127));
#38803=CARTESIAN_POINT('Ctrl Pts',(1.83311391452338,-1.,-3.36890396271864));
#38804=CARTESIAN_POINT('Ctrl Pts',(1.83784072967111,-1.,-3.37442462015914));
#38805=CARTESIAN_POINT('Ctrl Pts',(1.84269016931679,-1.,-3.38002968341222));
#38806=CARTESIAN_POINT('Ctrl Pts',(1.84764441927778,-1.,-3.38569092349639));
#38807=CARTESIAN_POINT('Ctrl Pts',(1.85267433291778,-1.,-3.39135802549415));
#38808=CARTESIAN_POINT('Ctrl Pts',(1.85774972037055,-1.,-3.39697816833056));
#38809=CARTESIAN_POINT('Ctrl Pts',(1.86285057051228,-1.,-3.40251742305445));
#38810=CARTESIAN_POINT('Ctrl Pts',(1.86797231196635,-1.,-3.40797080000513));
#38811=CARTESIAN_POINT('Ctrl Pts',(1.87311957248106,-1.,-3.41335043875182));
#38812=CARTESIAN_POINT('Ctrl Pts',(1.87830245689338,-1.,-3.4186785838376));
#38813=CARTESIAN_POINT('Ctrl Pts',(1.88353205062063,-1.,-3.42397908819741));
#38814=CARTESIAN_POINT('Ctrl Pts',(1.88881571322018,-1.,-3.42926852222174));
#38815=CARTESIAN_POINT('Ctrl Pts',(1.89415420002553,-1.,-3.43455074411591));
#38816=CARTESIAN_POINT('Ctrl Pts',(1.89954426803392,-1.,-3.43982185678105));
#38817=CARTESIAN_POINT('Ctrl Pts',(1.90498026502308,-1.,-3.44507323983374));
#38818=CARTESIAN_POINT('Ctrl Pts',(1.91045605593638,-1.,-3.45029522038885));
#38819=CARTESIAN_POINT('Ctrl Pts',(1.9159669478406,-1.,-3.45548074309943));
#38820=CARTESIAN_POINT('Ctrl Pts',(1.9215111821321,-1.,-3.4606282172248));
#38821=CARTESIAN_POINT('Ctrl Pts',(1.92708888591159,-1.,-3.46573953254084));
#38822=CARTESIAN_POINT('Ctrl Pts',(1.93270136427083,-1.,-3.47081872409783));
#38823=CARTESIAN_POINT('Ctrl Pts',(1.93835026973888,-1.,-3.47587040389916));
#38824=CARTESIAN_POINT('Ctrl Pts',(1.94403680554062,-1.,-3.48089825770412));
#38825=CARTESIAN_POINT('Ctrl Pts',(1.94976096795902,-1.,-3.485903616108));
#38826=CARTESIAN_POINT('Ctrl Pts',(1.95552193112071,-1.,-3.49088618670967));
#38827=CARTESIAN_POINT('Ctrl Pts',(1.96131836776489,-1.,-3.49584466573045));
#38828=CARTESIAN_POINT('Ctrl Pts',(1.9671487972405,-1.,-3.50077740176262));
#38829=CARTESIAN_POINT('Ctrl Pts',(1.9730119116298,-1.,-3.505683018611));
#38830=CARTESIAN_POINT('Ctrl Pts',(1.97890693666316,-1.,-3.51056110478334));
#38831=CARTESIAN_POINT('Ctrl Pts',(1.98483351061066,-1.,-3.51541198728362));
#38832=CARTESIAN_POINT('Ctrl Pts',(1.99079153006143,-1.,-3.52023644289195));
#38833=CARTESIAN_POINT('Ctrl Pts',(1.99678100339305,-1.,-3.52503542491745));
#38834=CARTESIAN_POINT('Ctrl Pts',(2.00280191090341,-1.,-3.52980980250181));
#38835=CARTESIAN_POINT('Ctrl Pts',(2.00885403604685,-1.,-3.53456004727321));
#38836=CARTESIAN_POINT('Ctrl Pts',(2.0149369884727,-1.,-3.53928627453503));
#38837=CARTESIAN_POINT('Ctrl Pts',(2.0210502798303,-1.,-3.54398838254011));
#38838=CARTESIAN_POINT('Ctrl Pts',(2.02719338376144,-1.,-3.54866616282173));
#38839=CARTESIAN_POINT('Ctrl Pts',(2.03336579658174,-1.,-3.55331941294018));
#38840=CARTESIAN_POINT('Ctrl Pts',(2.03956711120099,-1.,-3.55794807265052));
#38841=CARTESIAN_POINT('Ctrl Pts',(2.04579702159056,-1.,-3.5625522387181));
#38842=CARTESIAN_POINT('Ctrl Pts',(2.0520552817309,-1.,-3.56713209978208));
#38843=CARTESIAN_POINT('Ctrl Pts',(2.05834167687523,-1.,-3.57168789423507));
#38844=CARTESIAN_POINT('Ctrl Pts',(2.06465599229174,-1.,-3.576219862243));
#38845=CARTESIAN_POINT('Ctrl Pts',(2.07099797605747,-1.,-3.58072819250442));
#38846=CARTESIAN_POINT('Ctrl Pts',(2.07736732842117,-1.,-3.58521300039299));
#38847=CARTESIAN_POINT('Ctrl Pts',(2.08376373048756,-1.,-3.58967435355088));
#38848=CARTESIAN_POINT('Ctrl Pts',(2.09018686331416,-1.,-3.59411228625588));
#38849=CARTESIAN_POINT('Ctrl Pts',(2.09663642986631,-1.,-3.59852681775485));
#38850=CARTESIAN_POINT('Ctrl Pts',(2.1031121772821,-1.,-3.60291797088734));
#38851=CARTESIAN_POINT('Ctrl Pts',(2.10961391334462,-1.,-3.60728578532601));
#38852=CARTESIAN_POINT('Ctrl Pts',(2.11614149815106,-1.,-3.61163030609447));
#38853=CARTESIAN_POINT('Ctrl Pts',(2.12138417126355,-1.,-3.61508732216891));
#38854=CARTESIAN_POINT('Ctrl Pts',(2.12532774376758,-1.,-3.61766963590482));
#38855=CARTESIAN_POINT('Ctrl Pts',(2.12796193131368,-1.,-3.61938653649098));
#38856=CARTESIAN_POINT('Ctrl Pts',(2.12928030988903,-1.,-3.62024382630768));
#38857=CARTESIAN_POINT('',(2.25898783642071,-1.,-3.54075895182139));
#38858=CARTESIAN_POINT('',(2.12928030988903,-1.,-3.62024382630768));
#38859=CARTESIAN_POINT('',(2.1297112484669,-1.,-3.08655633322212));
#38860=CARTESIAN_POINT('Ctrl Pts',(2.25898783642071,-1.,-3.54075895182139));
#38861=CARTESIAN_POINT('Ctrl Pts',(2.2588225169468,-1.,-3.53919506647335));
#38862=CARTESIAN_POINT('Ctrl Pts',(2.25848864343951,-1.,-3.53606853162228));
#38863=CARTESIAN_POINT('Ctrl Pts',(2.25797812950104,-1.,-3.53138243688262));
#38864=CARTESIAN_POINT('Ctrl Pts',(2.25727802940898,-1.,-3.52514172847711));
#38865=CARTESIAN_POINT('Ctrl Pts',(2.25637049455044,-1.,-3.51735323667612));
#38866=CARTESIAN_POINT('Ctrl Pts',(2.25543046979799,-1.,-3.50957720117341));
#38867=CARTESIAN_POINT('Ctrl Pts',(2.25445785151868,-1.,-3.50181372617971));
#38868=CARTESIAN_POINT('Ctrl Pts',(2.25345251709759,-1.,-3.49406296494791));
#38869=CARTESIAN_POINT('Ctrl Pts',(2.25241433138695,-1.,-3.48632513240961));
#38870=CARTESIAN_POINT('Ctrl Pts',(2.25134314238687,-1.,-3.47860048448691));
#38871=CARTESIAN_POINT('Ctrl Pts',(2.25023877475942,-1.,-3.47088928979889));
#38872=CARTESIAN_POINT('Ctrl Pts',(2.2491010234604,-1.,-3.46319180177573));
#38873=CARTESIAN_POINT('Ctrl Pts',(2.2479296496077,-1.,-3.45550823512049));
#38874=CARTESIAN_POINT('Ctrl Pts',(2.2467243706995,-1.,-3.44783872863151));
#38875=CARTESIAN_POINT('Ctrl Pts',(2.24548487526022,-1.,-3.4401833646032));
#38876=CARTESIAN_POINT('Ctrl Pts',(2.24421085338727,-1.,-3.43254222614803));
#38877=CARTESIAN_POINT('Ctrl Pts',(2.24290202531101,-1.,-3.42491544683008));
#38878=CARTESIAN_POINT('Ctrl Pts',(2.24155816587844,-1.,-3.41730325539172));
#38879=CARTESIAN_POINT('Ctrl Pts',(2.24017914395289,-1.,-3.40970604190328));
#38880=CARTESIAN_POINT('Ctrl Pts',(2.2387649112415,-1.,-3.40212434705647));
#38881=CARTESIAN_POINT('Ctrl Pts',(2.23731541452791,-1.,-3.39455873448189));
#38882=CARTESIAN_POINT('Ctrl Pts',(2.23583052276308,-1.,-3.38700968549563));
#38883=CARTESIAN_POINT('Ctrl Pts',(2.23430995599561,-1.,-3.37947749555632));
#38884=CARTESIAN_POINT('Ctrl Pts',(2.23275319569221,-1.,-3.37196214349304));
#38885=CARTESIAN_POINT('Ctrl Pts',(2.23115945849739,-1.,-3.36446325227848));
#38886=CARTESIAN_POINT('Ctrl Pts',(2.22952789880982,-1.,-3.35698038165483));
#38887=CARTESIAN_POINT('Ctrl Pts',(2.22785777756576,-1.,-3.34951327111096));
#38888=CARTESIAN_POINT('Ctrl Pts',(2.22614863918047,-1.,-3.34206209449375));
#38889=CARTESIAN_POINT('Ctrl Pts',(2.22440049878511,-1.,-3.33462772849598));
#38890=CARTESIAN_POINT('Ctrl Pts',(2.22261398879635,-1.,-3.3272119632604));
#38891=CARTESIAN_POINT('Ctrl Pts',(2.22078990842776,-1.,-3.31981686778022));
#38892=CARTESIAN_POINT('Ctrl Pts',(2.21892881679086,-1.,-3.31244421655666));
#38893=CARTESIAN_POINT('Ctrl Pts',(2.21703059947836,-1.,-3.30509487819569));
#38894=CARTESIAN_POINT('Ctrl Pts',(2.21509406923368,-1.,-3.29776825193159));
#38895=CARTESIAN_POINT('Ctrl Pts',(2.21311648827391,-1.,-3.29046159238343));
#38896=CARTESIAN_POINT('Ctrl Pts',(2.21109449750641,-1.,-3.28317133333131));
#38897=CARTESIAN_POINT('Ctrl Pts',(2.2090250941743,-1.,-3.2758944800554));
#38898=CARTESIAN_POINT('Ctrl Pts',(2.20690665217742,-1.,-3.26863006136782));
#38899=CARTESIAN_POINT('Ctrl Pts',(2.20473979048678,-1.,-3.26138036637705));
#38900=CARTESIAN_POINT('Ctrl Pts',(2.20252866491545,-1.,-3.25415277957775));
#38901=CARTESIAN_POINT('Ctrl Pts',(2.20027910880981,-1.,-3.24695715874338));
#38902=CARTESIAN_POINT('Ctrl Pts',(2.19799623693253,-1.,-3.23980245361308));
#38903=CARTESIAN_POINT('Ctrl Pts',(2.19568204933168,-1.,-3.23269332296933));
#38904=CARTESIAN_POINT('Ctrl Pts',(2.19333345123538,-1.,-3.22562734221646));
#38905=CARTESIAN_POINT('Ctrl Pts',(2.19093901948667,-1.,-3.21859043114095));
#38906=CARTESIAN_POINT('Ctrl Pts',(2.18848253363901,-1.,-3.21156188355769));
#38907=CARTESIAN_POINT('Ctrl Pts',(2.18594876115934,-1.,-3.20452259717976));
#38908=CARTESIAN_POINT('Ctrl Pts',(2.18332898656602,-1.,-3.19746293740411));
#38909=CARTESIAN_POINT('Ctrl Pts',(2.18062558031778,-1.,-3.19038924261573));
#38910=CARTESIAN_POINT('Ctrl Pts',(2.17785968847142,-1.,-3.18333474627807));
#38911=CARTESIAN_POINT('Ctrl Pts',(2.17506466903694,-1.,-3.17635032802523));
#38912=CARTESIAN_POINT('Ctrl Pts',(2.17227212063817,-1.,-3.16948480019497));
#38913=CARTESIAN_POINT('Ctrl Pts',(2.16949910801219,-1.,-3.16276685102972));
#38914=CARTESIAN_POINT('Ctrl Pts',(2.16673728447689,-1.,-3.15618975593656));
#38915=CARTESIAN_POINT('Ctrl Pts',(2.16393520288072,-1.,-3.14968624389054));
#38916=CARTESIAN_POINT('Ctrl Pts',(2.16100905914435,-1.,-3.14314440427022));
#38917=CARTESIAN_POINT('Ctrl Pts',(2.15787423530676,-1.,-3.13645356563038));
#38918=CARTESIAN_POINT('Ctrl Pts',(2.1544724138292,-1.,-3.12954386795646));
#38919=CARTESIAN_POINT('Ctrl Pts',(2.15079698090584,-1.,-3.12242318151938));
#38920=CARTESIAN_POINT('Ctrl Pts',(2.14692798457532,-1.,-3.11522827016855));
#38921=CARTESIAN_POINT('Ctrl Pts',(2.14302815601973,-1.,-3.1082180866886));
#38922=CARTESIAN_POINT('Ctrl Pts',(2.13930228863751,-1.,-3.10171267391049));
#38923=CARTESIAN_POINT('Ctrl Pts',(2.13596538661048,-1.,-3.0960450242104));
#38924=CARTESIAN_POINT('Ctrl Pts',(2.13321032560893,-1.,-3.09151235281963));
#38925=CARTESIAN_POINT('Ctrl Pts',(2.13132142793017,-1.,-3.08855597949761));
#38926=CARTESIAN_POINT('Ctrl Pts',(2.13034980480424,-1.,-3.08717896996098));
#38927=CARTESIAN_POINT('Ctrl Pts',(2.12991938762373,-1.,-3.08668447250322));
#38928=CARTESIAN_POINT('Ctrl Pts',(2.1297578506149,-1.,-3.08657131089497));
#38929=CARTESIAN_POINT('Ctrl Pts',(2.1297112484669,-1.,-3.08655633322212));
#38930=CARTESIAN_POINT('',(2.27737254473378,-1.,-2.97927412174388));
#38931=CARTESIAN_POINT('Origin',(0.,-1.,0.));
#38932=CARTESIAN_POINT('',(2.66939624221984,-1.,-3.24257979115744));
#38933=CARTESIAN_POINT('Ctrl Pts',(2.27737254473378,-1.,-2.97927412174388));
#38934=CARTESIAN_POINT('Ctrl Pts',(2.27737238849212,-1.,-2.97932307137589));
#38935=CARTESIAN_POINT('Ctrl Pts',(2.27743009389704,-1.,-2.97951167106106));
#38936=CARTESIAN_POINT('Ctrl Pts',(2.27776738270369,-1.,-2.98007383024333));
#38937=CARTESIAN_POINT('Ctrl Pts',(2.27877674853833,-1.,-2.98142341809623));
#38938=CARTESIAN_POINT('Ctrl Pts',(2.28100472516582,-1.,-2.98413343613858));
#38939=CARTESIAN_POINT('Ctrl Pts',(2.28446419116036,-1.,-2.98815432734929));
#38940=CARTESIAN_POINT('Ctrl Pts',(2.28882328690601,-1.,-2.9930793098434));
#38941=CARTESIAN_POINT('Ctrl Pts',(2.29385894577999,-1.,-2.99863310340004));
#38942=CARTESIAN_POINT('Ctrl Pts',(2.29932091315939,-1.,-3.00450832658822));
#38943=CARTESIAN_POINT('Ctrl Pts',(2.30496809486528,-1.,-3.01041131063882));
#38944=CARTESIAN_POINT('Ctrl Pts',(2.31060449886577,-1.,-3.01610726819019));
#38945=CARTESIAN_POINT('Ctrl Pts',(2.31612479121528,-1.,-3.02147780668029));
#38946=CARTESIAN_POINT('Ctrl Pts',(2.32151944306299,-1.,-3.02652678416478));
#38947=CARTESIAN_POINT('Ctrl Pts',(2.32683687412027,-1.,-3.03133125185047));
#38948=CARTESIAN_POINT('Ctrl Pts',(2.33215619079807,-1.,-3.03600588555765));
#38949=CARTESIAN_POINT('Ctrl Pts',(2.33755792953726,-1.,-3.04066496998569));
#38950=CARTESIAN_POINT('Ctrl Pts',(2.3430901708402,-1.,-3.04537822217311));
#38951=CARTESIAN_POINT('Ctrl Pts',(2.34875673090816,-1.,-3.05015565829976));
#38952=CARTESIAN_POINT('Ctrl Pts',(2.35453559889506,-1.,-3.05497218368188));
#38953=CARTESIAN_POINT('Ctrl Pts',(2.36039011602084,-1.,-3.05978266240056));
#38954=CARTESIAN_POINT('Ctrl Pts',(2.36628220107001,-1.,-3.06453964643152));
#38955=CARTESIAN_POINT('Ctrl Pts',(2.37218678163157,-1.,-3.06921275497472));
#38956=CARTESIAN_POINT('Ctrl Pts',(2.37809856205524,-1.,-3.07379777492133));
#38957=CARTESIAN_POINT('Ctrl Pts',(2.38402401216107,-1.,-3.07830597244301));
#38958=CARTESIAN_POINT('Ctrl Pts',(2.38997659219192,-1.,-3.08275773747083));
#38959=CARTESIAN_POINT('Ctrl Pts',(2.39597098250635,-1.,-3.08717489512919));
#38960=CARTESIAN_POINT('Ctrl Pts',(2.40201704423352,-1.,-3.09157266051115));
#38961=CARTESIAN_POINT('Ctrl Pts',(2.40811612696382,-1.,-3.09595472616093));
#38962=CARTESIAN_POINT('Ctrl Pts',(2.41426441798067,-1.,-3.10031775027683));
#38963=CARTESIAN_POINT('Ctrl Pts',(2.42045498612494,-1.,-3.10465410280902));
#38964=CARTESIAN_POINT('Ctrl Pts',(2.42668025870013,-1.,-3.10895518969592));
#38965=CARTESIAN_POINT('Ctrl Pts',(2.4329344968514,-1.,-3.11321477659012));
#38966=CARTESIAN_POINT('Ctrl Pts',(2.43921571477975,-1.,-3.11743156744182));
#38967=CARTESIAN_POINT('Ctrl Pts',(2.44552433364716,-1.,-3.12160740887768));
#38968=CARTESIAN_POINT('Ctrl Pts',(2.45186227369848,-1.,-3.12574608210849));
#38969=CARTESIAN_POINT('Ctrl Pts',(2.45823188859366,-1.,-3.12985188384372));
#38970=CARTESIAN_POINT('Ctrl Pts',(2.4646349433237,-1.,-3.13392826623902));
#38971=CARTESIAN_POINT('Ctrl Pts',(2.47107164236827,-1.,-3.13797654408931));
#38972=CARTESIAN_POINT('Ctrl Pts',(2.47754112428027,-1.,-3.14199655778845));
#38973=CARTESIAN_POINT('Ctrl Pts',(2.48404187418376,-1.,-3.1459872272388));
#38974=CARTESIAN_POINT('Ctrl Pts',(2.49057217131985,-1.,-3.14994715298903));
#38975=CARTESIAN_POINT('Ctrl Pts',(2.49713050858911,-1.,-3.15387518039064));
#38976=CARTESIAN_POINT('Ctrl Pts',(2.50371605688287,-1.,-3.15777102413998));
#38977=CARTESIAN_POINT('Ctrl Pts',(2.51032851007939,-1.,-3.16163506380211));
#38978=CARTESIAN_POINT('Ctrl Pts',(2.51696788755615,-1.,-3.16546808277069));
#38979=CARTESIAN_POINT('Ctrl Pts',(2.523634346718,-1.,-3.16927102130751));
#38980=CARTESIAN_POINT('Ctrl Pts',(2.5303280040691,-1.,-3.17304474093574));
#38981=CARTESIAN_POINT('Ctrl Pts',(2.53704871950871,-1.,-3.17678974135225));
#38982=CARTESIAN_POINT('Ctrl Pts',(2.54379612552948,-1.,-3.18050619750515));
#38983=CARTESIAN_POINT('Ctrl Pts',(2.55056972387638,-1.,-3.18419408529482));
#38984=CARTESIAN_POINT('Ctrl Pts',(2.55736896206016,-1.,-3.1878532811617));
#38985=CARTESIAN_POINT('Ctrl Pts',(2.56419331092909,-1.,-3.19148366395201));
#38986=CARTESIAN_POINT('Ctrl Pts',(2.57104235898053,-1.,-3.19508523784548));
#38987=CARTESIAN_POINT('Ctrl Pts',(2.577915819091,-1.,-3.19865814628955));
#38988=CARTESIAN_POINT('Ctrl Pts',(2.58481347777953,-1.,-3.20220261408685));
#38989=CARTESIAN_POINT('Ctrl Pts',(2.59173516023605,-1.,-3.20571891028879));
#38990=CARTESIAN_POINT('Ctrl Pts',(2.59868069194267,-1.,-3.2092073056959));
#38991=CARTESIAN_POINT('Ctrl Pts',(2.60564985359699,-1.,-3.21266802609297));
#38992=CARTESIAN_POINT('Ctrl Pts',(2.61264236718662,-1.,-3.21610123232465));
#38993=CARTESIAN_POINT('Ctrl Pts',(2.61965792832396,-1.,-3.21950704108654));
#38994=CARTESIAN_POINT('Ctrl Pts',(2.62669622735548,-1.,-3.222885536128));
#38995=CARTESIAN_POINT('Ctrl Pts',(2.63375697391438,-1.,-3.22623678292539));
#38996=CARTESIAN_POINT('Ctrl Pts',(2.64083992182478,-1.,-3.2295608435934));
#38997=CARTESIAN_POINT('Ctrl Pts',(2.64794488744246,-1.,-3.23285778738558));
#38998=CARTESIAN_POINT('Ctrl Pts',(2.6550717396303,-1.,-3.23612768065687));
#38999=CARTESIAN_POINT('Ctrl Pts',(2.6607906631973,-1.,-3.23872200036311));
#39000=CARTESIAN_POINT('Ctrl Pts',(2.66508964664767,-1.,-3.24065561087681));
#39001=CARTESIAN_POINT('Ctrl Pts',(2.66795998539861,-1.,-3.24193929584813));
#39002=CARTESIAN_POINT('Ctrl Pts',(2.66939624221984,-1.,-3.24257979115744));
#39003=CARTESIAN_POINT('',(2.78507268004356,-1.,-3.14378277984898));
#39004=CARTESIAN_POINT('',(2.66939624221984,-1.,-3.24257979115744));
#39005=CARTESIAN_POINT('',(2.58633475774921,-1.,-2.71539546306948));
#39006=CARTESIAN_POINT('Ctrl Pts',(2.78507268004356,-1.,-3.14378277984898));
#39007=CARTESIAN_POINT('Ctrl Pts',(2.7846647503589,-1.,-3.14226401018816));
#39008=CARTESIAN_POINT('Ctrl Pts',(2.78384588958165,-1.,-3.13922819749279));
#39009=CARTESIAN_POINT('Ctrl Pts',(2.78260859419319,-1.,-3.13467965833037));
#39010=CARTESIAN_POINT('Ctrl Pts',(2.78094085161413,-1.,-3.12862530318457));
#39011=CARTESIAN_POINT('Ctrl Pts',(2.77882610146731,-1.,-3.12107467037201));
#39012=CARTESIAN_POINT('Ctrl Pts',(2.77668121002545,-1.,-3.11354142303921));
#39013=CARTESIAN_POINT('Ctrl Pts',(2.77450609123362,-1.,-3.10602568032564));
#39014=CARTESIAN_POINT('Ctrl Pts',(2.77230064796057,-1.,-3.0985276127786));
#39015=CARTESIAN_POINT('Ctrl Pts',(2.7700647803451,-1.,-3.09104745382531));
#39016=CARTESIAN_POINT('Ctrl Pts',(2.76779837829373,-1.,-3.08358548001504));
#39017=CARTESIAN_POINT('Ctrl Pts',(2.76550131064852,-1.,-3.07614198408862));
#39018=CARTESIAN_POINT('Ctrl Pts',(2.76317341453493,-1.,-3.0687172484321));
#39019=CARTESIAN_POINT('Ctrl Pts',(2.76081448759882,-1.,-3.06131152247454));
#39020=CARTESIAN_POINT('Ctrl Pts',(2.75842427252931,-1.,-3.05392498749847));
#39021=CARTESIAN_POINT('Ctrl Pts',(2.75600247455925,-1.,-3.04655777351067));
#39022=CARTESIAN_POINT('Ctrl Pts',(2.75354880060314,-1.,-3.03921001107977));
#39023=CARTESIAN_POINT('Ctrl Pts',(2.75106299522979,-1.,-3.03188187589107));
#39024=CARTESIAN_POINT('Ctrl Pts',(2.7485448718414,-1.,-3.02457362909245));
#39025=CARTESIAN_POINT('Ctrl Pts',(2.74599436193625,-1.,-3.01728567646611));
#39026=CARTESIAN_POINT('Ctrl Pts',(2.74341150239887,-1.,-3.01001855960162));
#39027=CARTESIAN_POINT('Ctrl Pts',(2.74079632883931,-1.,-3.00277284351521));
#39028=CARTESIAN_POINT('Ctrl Pts',(2.73814878711641,-1.,-2.99554902409778));
#39029=CARTESIAN_POINT('Ctrl Pts',(2.73546864694536,-1.,-2.9883474369644));
#39030=CARTESIAN_POINT('Ctrl Pts',(2.73275539286497,-1.,-2.98116814232129));
#39031=CARTESIAN_POINT('Ctrl Pts',(2.73000819218414,-1.,-2.97401089032677));
#39032=CARTESIAN_POINT('Ctrl Pts',(2.72722614084076,-1.,-2.96687537842451));
#39033=CARTESIAN_POINT('Ctrl Pts',(2.72440846811729,-1.,-2.95976146492576));
#39034=CARTESIAN_POINT('Ctrl Pts',(2.72155475123364,-1.,-2.95266939280621));
#39035=CARTESIAN_POINT('Ctrl Pts',(2.71866514227965,-1.,-2.94560002559806));
#39036=CARTESIAN_POINT('Ctrl Pts',(2.7157405459259,-1.,-2.93855503247266));
#39037=CARTESIAN_POINT('Ctrl Pts',(2.71278207520817,-1.,-2.93153633192595));
#39038=CARTESIAN_POINT('Ctrl Pts',(2.70979055994754,-1.,-2.92454558914778));
#39039=CARTESIAN_POINT('Ctrl Pts',(2.70676602302518,-1.,-2.91758367994737));
#39040=CARTESIAN_POINT('Ctrl Pts',(2.70370719782113,-1.,-2.91065019668329));
#39041=CARTESIAN_POINT('Ctrl Pts',(2.70061095078692,-1.,-2.90374285605838));
#39042=CARTESIAN_POINT('Ctrl Pts',(2.69747340630625,-1.,-2.89685866123671));
#39043=CARTESIAN_POINT('Ctrl Pts',(2.69429113011374,-1.,-2.88999512410309));
#39044=CARTESIAN_POINT('Ctrl Pts',(2.69106236420198,-1.,-2.88315153980466));
#39045=CARTESIAN_POINT('Ctrl Pts',(2.68778807801686,-1.,-2.8763300724388));
#39046=CARTESIAN_POINT('Ctrl Pts',(2.68447353139599,-1.,-2.86953736547238));
#39047=CARTESIAN_POINT('Ctrl Pts',(2.68112602796308,-1.,-2.86278224277689));
#39048=CARTESIAN_POINT('Ctrl Pts',(2.67775201955724,-1.,-2.85607274378018));
#39049=CARTESIAN_POINT('Ctrl Pts',(2.67435421039677,-1.,-2.84941315703092));
#39050=CARTESIAN_POINT('Ctrl Pts',(2.67092916452125,-1.,-2.84280157191323));
#39051=CARTESIAN_POINT('Ctrl Pts',(2.66746339678107,-1.,-2.83622586853982));
#39052=CARTESIAN_POINT('Ctrl Pts',(2.6639376472693,-1.,-2.82966813308998));
#39053=CARTESIAN_POINT('Ctrl Pts',(2.66033388273461,-1.,-2.82311188135078));
#39054=CARTESIAN_POINT('Ctrl Pts',(2.65664198781344,-1.,-2.81654896073883));
#39055=CARTESIAN_POINT('Ctrl Pts',(2.65286529532208,-1.,-2.80998526078165));
#39056=CARTESIAN_POINT('Ctrl Pts',(2.64902988983337,-1.,-2.80345029781152));
#39057=CARTESIAN_POINT('Ctrl Pts',(2.64517667799319,-1.,-2.79698910670736));
#39058=CARTESIAN_POINT('Ctrl Pts',(2.64134450532584,-1.,-2.79064495573224));
#39059=CARTESIAN_POINT('Ctrl Pts',(2.637554714303,-1.,-2.78444351041571));
#39060=CARTESIAN_POINT('Ctrl Pts',(2.63379800904599,-1.,-2.77837943466449));
#39061=CARTESIAN_POINT('Ctrl Pts',(2.63001305229625,-1.,-2.77239433377921));
#39062=CARTESIAN_POINT('Ctrl Pts',(2.62609956506355,-1.,-2.76639078479021));
#39063=CARTESIAN_POINT('Ctrl Pts',(2.62195665834605,-1.,-2.76027271596686));
#39064=CARTESIAN_POINT('Ctrl Pts',(2.61751580407667,-1.,-2.7539802502603));
#39065=CARTESIAN_POINT('Ctrl Pts',(2.61277170105813,-1.,-2.74752219567252));
#39066=CARTESIAN_POINT('Ctrl Pts',(2.60782480638448,-1.,-2.7410211099909));
#39067=CARTESIAN_POINT('Ctrl Pts',(2.60287635688728,-1.,-2.73470730109615));
#39068=CARTESIAN_POINT('Ctrl Pts',(2.59817869034746,-1.,-2.7288648348152));
#39069=CARTESIAN_POINT('Ctrl Pts',(2.59399625537278,-1.,-2.72378896977134));
#39070=CARTESIAN_POINT('Ctrl Pts',(2.59056604771971,-1.,-2.71974308958086));
#39071=CARTESIAN_POINT('Ctrl Pts',(2.58823792682672,-1.,-2.71711860281815));
#39072=CARTESIAN_POINT('Ctrl Pts',(2.58706285424358,-1.,-2.71591054189786));
#39073=CARTESIAN_POINT('Ctrl Pts',(2.58656037976753,-1.,-2.71548946460575));
#39074=CARTESIAN_POINT('Ctrl Pts',(2.58638312917167,-1.,-2.71540296616024));
#39075=CARTESIAN_POINT('Ctrl Pts',(2.58633475774921,-1.,-2.71539546306948));
#39076=CARTESIAN_POINT('',(2.71539546306824,-1.,-2.58633475775051));
#39077=CARTESIAN_POINT('Origin',(0.,-1.,0.));
#39078=CARTESIAN_POINT('',(3.14378277984898,-1.,-2.78507268004356));
#39079=CARTESIAN_POINT('Ctrl Pts',(2.71539546306824,-1.,-2.58633475775051));
#39080=CARTESIAN_POINT('Ctrl Pts',(2.71540296615967,-1.,-2.58638312917291));
#39081=CARTESIAN_POINT('Ctrl Pts',(2.71548946460616,-1.,-2.58656037976884));
#39082=CARTESIAN_POINT('Ctrl Pts',(2.71591054189884,-1.,-2.58706285424469));
#39083=CARTESIAN_POINT('Ctrl Pts',(2.7171186028189,-1.,-2.58823792682724));
#39084=CARTESIAN_POINT('Ctrl Pts',(2.7197430895797,-1.,-2.59056604771863));
#39085=CARTESIAN_POINT('Ctrl Pts',(2.72378896977273,-1.,-2.59399625537407));
#39086=CARTESIAN_POINT('Ctrl Pts',(2.72886483481804,-1.,-2.5981786903501));
#39087=CARTESIAN_POINT('Ctrl Pts',(2.73470730109906,-1.,-2.60287635689));
#39088=CARTESIAN_POINT('Ctrl Pts',(2.74102110999284,-1.,-2.60782480638629));
#39089=CARTESIAN_POINT('Ctrl Pts',(2.74752219567307,-1.,-2.61277170105864));
#39090=CARTESIAN_POINT('Ctrl Pts',(2.75398025025967,-1.,-2.61751580407608));
#39091=CARTESIAN_POINT('Ctrl Pts',(2.76027271596564,-1.,-2.62195665834491));
#39092=CARTESIAN_POINT('Ctrl Pts',(2.76639078478898,-1.,-2.6260995650624));
#39093=CARTESIAN_POINT('Ctrl Pts',(2.77239433377839,-1.,-2.63001305229548));
#39094=CARTESIAN_POINT('Ctrl Pts',(2.77837943466423,-1.,-2.63379800904575));
#39095=CARTESIAN_POINT('Ctrl Pts',(2.78444351041594,-1.,-2.63755471430322));
#39096=CARTESIAN_POINT('Ctrl Pts',(2.79064495573275,-1.,-2.64134450532632));
#39097=CARTESIAN_POINT('Ctrl Pts',(2.7969891067079,-1.,-2.6451766779937));
#39098=CARTESIAN_POINT('Ctrl Pts',(2.80345029781191,-1.,-2.64902988983373));
#39099=CARTESIAN_POINT('Ctrl Pts',(2.80998526078179,-1.,-2.65286529532221));
#39100=CARTESIAN_POINT('Ctrl Pts',(2.81654896073874,-1.,-2.65664198781335));
#39101=CARTESIAN_POINT('Ctrl Pts',(2.82311188135053,-1.,-2.66033388273437));
#39102=CARTESIAN_POINT('Ctrl Pts',(2.82966813308969,-1.,-2.66393764726902));
#39103=CARTESIAN_POINT('Ctrl Pts',(2.8362258685396,-1.,-2.66746339678085));
#39104=CARTESIAN_POINT('Ctrl Pts',(2.84280157191314,-1.,-2.67092916452117));
#39105=CARTESIAN_POINT('Ctrl Pts',(2.84941315703096,-1.,-2.67435421039682));
#39106=CARTESIAN_POINT('Ctrl Pts',(2.85607274378031,-1.,-2.67775201955736));
#39107=CARTESIAN_POINT('Ctrl Pts',(2.86278224277705,-1.,-2.68112602796323));
#39108=CARTESIAN_POINT('Ctrl Pts',(2.8695373654725,-1.,-2.68447353139611));
#39109=CARTESIAN_POINT('Ctrl Pts',(2.87633007243885,-1.,-2.68778807801691));
#39110=CARTESIAN_POINT('Ctrl Pts',(2.88315153980464,-1.,-2.69106236420197));
#39111=CARTESIAN_POINT('Ctrl Pts',(2.88999512410304,-1.,-2.69429113011369));
#39112=CARTESIAN_POINT('Ctrl Pts',(2.89685866123668,-1.,-2.69747340630621));
#39113=CARTESIAN_POINT('Ctrl Pts',(2.90374285605839,-1.,-2.70061095078692));
#39114=CARTESIAN_POINT('Ctrl Pts',(2.91065019668331,-1.,-2.70370719782114));
#39115=CARTESIAN_POINT('Ctrl Pts',(2.91758367994738,-1.,-2.70676602302518));
#39116=CARTESIAN_POINT('Ctrl Pts',(2.92454558914774,-1.,-2.70979055994751));
#39117=CARTESIAN_POINT('Ctrl Pts',(2.93153633192583,-1.,-2.71278207520807));
#39118=CARTESIAN_POINT('Ctrl Pts',(2.93855503247248,-1.,-2.71574054592575));
#39119=CARTESIAN_POINT('Ctrl Pts',(2.94560002559789,-1.,-2.71866514227951));
#39120=CARTESIAN_POINT('Ctrl Pts',(2.95266939280617,-1.,-2.72155475123361));
#39121=CARTESIAN_POINT('Ctrl Pts',(2.95976146492595,-1.,-2.72440846811745));
#39122=CARTESIAN_POINT('Ctrl Pts',(2.96687537842492,-1.,-2.72722614084112));
#39123=CARTESIAN_POINT('Ctrl Pts',(2.97401089032729,-1.,-2.7300081921846));
#39124=CARTESIAN_POINT('Ctrl Pts',(2.98116814232175,-1.,-2.73275539286537));
#39125=CARTESIAN_POINT('Ctrl Pts',(2.98834743696455,-1.,-2.73546864694548));
#39126=CARTESIAN_POINT('Ctrl Pts',(2.99554902409741,-1.,-2.73814878711609));
#39127=CARTESIAN_POINT('Ctrl Pts',(3.00277284351431,-1.,-2.74079632883852));
#39128=CARTESIAN_POINT('Ctrl Pts',(3.01001855960041,-1.,-2.7434115023978));
#39129=CARTESIAN_POINT('Ctrl Pts',(3.01728567646502,-1.,-2.74599436193528));
#39130=CARTESIAN_POINT('Ctrl Pts',(3.02457362909199,-1.,-2.74854487184099));
#39131=CARTESIAN_POINT('Ctrl Pts',(3.03188187589168,-1.,-2.75106299523032));
#39132=CARTESIAN_POINT('Ctrl Pts',(3.03921001108158,-1.,-2.75354880060473));
#39133=CARTESIAN_POINT('Ctrl Pts',(3.04655777351333,-1.,-2.7560024745616));
#39134=CARTESIAN_POINT('Ctrl Pts',(3.05392498750112,-1.,-2.75842427253164));
#39135=CARTESIAN_POINT('Ctrl Pts',(3.06131152247599,-1.,-2.76081448760011));
#39136=CARTESIAN_POINT('Ctrl Pts',(3.06871724843121,-1.,-2.76317341453415));
#39137=CARTESIAN_POINT('Ctrl Pts',(3.07614198408488,-1.,-2.76550131064522));
#39138=CARTESIAN_POINT('Ctrl Pts',(3.08358548000904,-1.,-2.76779837828843));
#39139=CARTESIAN_POINT('Ctrl Pts',(3.09104745381882,-1.,-2.77006478033937));
#39140=CARTESIAN_POINT('Ctrl Pts',(3.09852761277432,-1.,-2.77230064795679));
#39141=CARTESIAN_POINT('Ctrl Pts',(3.10602568032641,-1.,-2.7745060912343));
#39142=CARTESIAN_POINT('Ctrl Pts',(3.11354142304692,-1.,-2.77668121003225));
#39143=CARTESIAN_POINT('Ctrl Pts',(3.12107467038623,-1.,-2.77882610147986));
#39144=CARTESIAN_POINT('Ctrl Pts',(3.12862530320194,-1.,-2.78094085162947));
#39145=CARTESIAN_POINT('Ctrl Pts',(3.1346796583452,-1.,-2.78260859420629));
#39146=CARTESIAN_POINT('Ctrl Pts',(3.13922819750185,-1.,-2.78384588958965));
#39147=CARTESIAN_POINT('Ctrl Pts',(3.14226401019149,-1.,-2.78466475036183));
#39148=CARTESIAN_POINT('Ctrl Pts',(3.14378277984898,-1.,-2.78507268004356));
#39149=CARTESIAN_POINT('',(3.24257979115744,-1.,-2.66939624221984));
#39150=CARTESIAN_POINT('',(3.14378277984898,-1.,-2.78507268004356));
#39151=CARTESIAN_POINT('',(2.97927412174279,-1.,-2.27737254473521));
#39152=CARTESIAN_POINT('Ctrl Pts',(3.24257979115744,-1.,-2.66939624221984));
#39153=CARTESIAN_POINT('Ctrl Pts',(3.24193929584471,-1.,-2.66795998539579));
#39154=CARTESIAN_POINT('Ctrl Pts',(3.24065561086749,-1.,-2.66508964663997));
#39155=CARTESIAN_POINT('Ctrl Pts',(3.23872200034785,-1.,-2.6607906631847));
#39156=CARTESIAN_POINT('Ctrl Pts',(3.236127680639,-1.,-2.65507173961555));
#39157=CARTESIAN_POINT('Ctrl Pts',(3.23285778737096,-1.,-2.64794488743038));
#39158=CARTESIAN_POINT('Ctrl Pts',(3.22956084358547,-1.,-2.64083992181823));
#39159=CARTESIAN_POINT('Ctrl Pts',(3.2262367829246,-1.,-2.63375697391372));
#39160=CARTESIAN_POINT('Ctrl Pts',(3.2228855361324,-1.,-2.62669622735912));
#39161=CARTESIAN_POINT('Ctrl Pts',(3.21950704109321,-1.,-2.61965792832947));
#39162=CARTESIAN_POINT('Ctrl Pts',(3.21610123233082,-1.,-2.61264236719171));
#39163=CARTESIAN_POINT('Ctrl Pts',(3.21266802609681,-1.,-2.60564985360017));
#39164=CARTESIAN_POINT('Ctrl Pts',(3.20920730569681,-1.,-2.59868069194342));
#39165=CARTESIAN_POINT('Ctrl Pts',(3.2057189102873,-1.,-2.59173516023481));
#39166=CARTESIAN_POINT('Ctrl Pts',(3.20220261408414,-1.,-2.58481347777729));
#39167=CARTESIAN_POINT('Ctrl Pts',(3.19865814628682,-1.,-2.57791581908875));
#39168=CARTESIAN_POINT('Ctrl Pts',(3.19508523784363,-1.,-2.57104235897899));
#39169=CARTESIAN_POINT('Ctrl Pts',(3.19148366395139,-1.,-2.56419331092858));
#39170=CARTESIAN_POINT('Ctrl Pts',(3.18785328116218,-1.,-2.55736896206056));
#39171=CARTESIAN_POINT('Ctrl Pts',(3.18419408529594,-1.,-2.55056972387731));
#39172=CARTESIAN_POINT('Ctrl Pts',(3.18050619750639,-1.,-2.54379612553051));
#39173=CARTESIAN_POINT('Ctrl Pts',(3.17678974135318,-1.,-2.53704871950948));
#39174=CARTESIAN_POINT('Ctrl Pts',(3.17304474093612,-1.,-2.53032800406941));
#39175=CARTESIAN_POINT('Ctrl Pts',(3.16927102130735,-1.,-2.52363434671788));
#39176=CARTESIAN_POINT('Ctrl Pts',(3.16546808277023,-1.,-2.51696788755577));
#39177=CARTESIAN_POINT('Ctrl Pts',(3.16163506380157,-1.,-2.51032851007894));
#39178=CARTESIAN_POINT('Ctrl Pts',(3.15777102413957,-1.,-2.50371605688252));
#39179=CARTESIAN_POINT('Ctrl Pts',(3.15387518039046,-1.,-2.49713050858896));
#39180=CARTESIAN_POINT('Ctrl Pts',(3.14994715298907,-1.,-2.49057217131988));
#39181=CARTESIAN_POINT('Ctrl Pts',(3.14598722723896,-1.,-2.4840418741839));
#39182=CARTESIAN_POINT('Ctrl Pts',(3.14199655778863,-1.,-2.47754112428043));
#39183=CARTESIAN_POINT('Ctrl Pts',(3.13797654408943,-1.,-2.47107164236838));
#39184=CARTESIAN_POINT('Ctrl Pts',(3.13392826623906,-1.,-2.46463494332374));
#39185=CARTESIAN_POINT('Ctrl Pts',(3.12985188384371,-1.,-2.45823188859366));
#39186=CARTESIAN_POINT('Ctrl Pts',(3.12574608210847,-1.,-2.45186227369846));
#39187=CARTESIAN_POINT('Ctrl Pts',(3.12160740887768,-1.,-2.44552433364715));
#39188=CARTESIAN_POINT('Ctrl Pts',(3.11743156744186,-1.,-2.43921571477977));
#39189=CARTESIAN_POINT('Ctrl Pts',(3.11321477659018,-1.,-2.43293449685144));
#39190=CARTESIAN_POINT('Ctrl Pts',(3.10895518969595,-1.,-2.42668025870015));
#39191=CARTESIAN_POINT('Ctrl Pts',(3.10465410280896,-1.,-2.42045498612489));
#39192=CARTESIAN_POINT('Ctrl Pts',(3.1003177502767,-1.,-2.41426441798057));
#39193=CARTESIAN_POINT('Ctrl Pts',(3.09595472616076,-1.,-2.40811612696369));
#39194=CARTESIAN_POINT('Ctrl Pts',(3.091572660511,-1.,-2.40201704423341));
#39195=CARTESIAN_POINT('Ctrl Pts',(3.08717489512914,-1.,-2.39597098250631));
#39196=CARTESIAN_POINT('Ctrl Pts',(3.08275773747093,-1.,-2.38997659219199));
#39197=CARTESIAN_POINT('Ctrl Pts',(3.07830597244326,-1.,-2.38402401216126));
#39198=CARTESIAN_POINT('Ctrl Pts',(3.07379777492165,-1.,-2.37809856205548));
#39199=CARTESIAN_POINT('Ctrl Pts',(3.069212754975,-1.,-2.37218678163178));
#39200=CARTESIAN_POINT('Ctrl Pts',(3.06453964643162,-1.,-2.36628220107009));
#39201=CARTESIAN_POINT('Ctrl Pts',(3.0597826624004,-1.,-2.36039011602072));
#39202=CARTESIAN_POINT('Ctrl Pts',(3.05497218368146,-1.,-2.35453559889474));
#39203=CARTESIAN_POINT('Ctrl Pts',(3.05015565829918,-1.,-2.34875673090771));
#39204=CARTESIAN_POINT('Ctrl Pts',(3.04537822217256,-1.,-2.34309017083977));
#39205=CARTESIAN_POINT('Ctrl Pts',(3.04066496998544,-1.,-2.33755792953706));
#39206=CARTESIAN_POINT('Ctrl Pts',(3.03600588555793,-1.,-2.33215619079829));
#39207=CARTESIAN_POINT('Ctrl Pts',(3.03133125185136,-1.,-2.32683687412097));
#39208=CARTESIAN_POINT('Ctrl Pts',(3.02652678416611,-1.,-2.32151944306402));
#39209=CARTESIAN_POINT('Ctrl Pts',(3.0214778066816,-1.,-2.31612479121631));
#39210=CARTESIAN_POINT('Ctrl Pts',(3.01610726819086,-1.,-2.31060449886629));
#39211=CARTESIAN_POINT('Ctrl Pts',(3.01041131063823,-1.,-2.30496809486482));
#39212=CARTESIAN_POINT('Ctrl Pts',(3.00450832658613,-1.,-2.29932091315775));
#39213=CARTESIAN_POINT('Ctrl Pts',(2.99863310339691,-1.,-2.29385894577754));
#39214=CARTESIAN_POINT('Ctrl Pts',(2.99307930984034,-1.,-2.28882328690362));
#39215=CARTESIAN_POINT('Ctrl Pts',(2.9881543273478,-1.,-2.28446419115919));
#39216=CARTESIAN_POINT('Ctrl Pts',(2.98413343613983,-1.,-2.28100472516679));
#39217=CARTESIAN_POINT('Ctrl Pts',(2.9814234180956,-1.,-2.27877674853766));
#39218=CARTESIAN_POINT('Ctrl Pts',(2.98007383024207,-1.,-2.27776738270289));
#39219=CARTESIAN_POINT('Ctrl Pts',(2.9795116710597,-1.,-2.27743009389684));
#39220=CARTESIAN_POINT('Ctrl Pts',(2.97932307137476,-1.,-2.27737238849287));
#39221=CARTESIAN_POINT('Ctrl Pts',(2.97927412174279,-1.,-2.27737254473521));
#39222=CARTESIAN_POINT('',(3.08655633322109,-1.,-2.12971124846838));
#39223=CARTESIAN_POINT('Origin',(0.,-1.,0.));
#39224=CARTESIAN_POINT('',(3.54075895182139,-1.,-2.25898783642071));
#39225=CARTESIAN_POINT('Ctrl Pts',(3.08655633322109,-1.,-2.12971124846838));
#39226=CARTESIAN_POINT('Ctrl Pts',(3.0865713108946,-1.,-2.1297578506162));
#39227=CARTESIAN_POINT('Ctrl Pts',(3.08668447250383,-1.,-2.12991938762497));
#39228=CARTESIAN_POINT('Ctrl Pts',(3.08717896996213,-1.,-2.13034980480519));
#39229=CARTESIAN_POINT('Ctrl Pts',(3.08855597949844,-1.,-2.13132142793056));
#39230=CARTESIAN_POINT('Ctrl Pts',(3.09151235281832,-1.,-2.13321032560805));
#39231=CARTESIAN_POINT('Ctrl Pts',(3.09604502421197,-1.,-2.13596538661154));
#39232=CARTESIAN_POINT('Ctrl Pts',(3.1017126739137,-1.,-2.13930228863968));
#39233=CARTESIAN_POINT('Ctrl Pts',(3.10821808669189,-1.,-2.14302815602195));
#39234=CARTESIAN_POINT('Ctrl Pts',(3.11522827017075,-1.,-2.1469279845768));
#39235=CARTESIAN_POINT('Ctrl Pts',(3.12242318152001,-1.,-2.15079698090627));
#39236=CARTESIAN_POINT('Ctrl Pts',(3.12954386795575,-1.,-2.15447241382872));
#39237=CARTESIAN_POINT('Ctrl Pts',(3.136453565629,-1.,-2.15787423530583));
#39238=CARTESIAN_POINT('Ctrl Pts',(3.14314440426882,-1.,-2.16100905914341));
#39239=CARTESIAN_POINT('Ctrl Pts',(3.14968624388961,-1.,-2.16393520288009));
#39240=CARTESIAN_POINT('Ctrl Pts',(3.15618975593627,-1.,-2.1667372844767));
#39241=CARTESIAN_POINT('Ctrl Pts',(3.16276685102999,-1.,-2.16949910801237));
#39242=CARTESIAN_POINT('Ctrl Pts',(3.16948480019555,-1.,-2.17227212063857));
#39243=CARTESIAN_POINT('Ctrl Pts',(3.17635032802584,-1.,-2.17506466903736));
#39244=CARTESIAN_POINT('Ctrl Pts',(3.18333474627851,-1.,-2.17785968847172));
#39245=CARTESIAN_POINT('Ctrl Pts',(3.19038924261589,-1.,-2.18062558031789));
#39246=CARTESIAN_POINT('Ctrl Pts',(3.197462937404,-1.,-2.18332898656595));
#39247=CARTESIAN_POINT('Ctrl Pts',(3.20452259717947,-1.,-2.18594876115914));
#39248=CARTESIAN_POINT('Ctrl Pts',(3.21156188355736,-1.,-2.18848253363878));
#39249=CARTESIAN_POINT('Ctrl Pts',(3.21859043114069,-1.,-2.1909390194865));
#39250=CARTESIAN_POINT('Ctrl Pts',(3.22562734221636,-1.,-2.19333345123531));
#39251=CARTESIAN_POINT('Ctrl Pts',(3.23269332296938,-1.,-2.19568204933172));
#39252=CARTESIAN_POINT('Ctrl Pts',(3.23980245361323,-1.,-2.19799623693263));
#39253=CARTESIAN_POINT('Ctrl Pts',(3.24695715874356,-1.,-2.20027910880993));
#39254=CARTESIAN_POINT('Ctrl Pts',(3.25415277957789,-1.,-2.20252866491554));
#39255=CARTESIAN_POINT('Ctrl Pts',(3.26138036637711,-1.,-2.20473979048682));
#39256=CARTESIAN_POINT('Ctrl Pts',(3.2686300613678,-1.,-2.20690665217741));
#39257=CARTESIAN_POINT('Ctrl Pts',(3.27589448005534,-1.,-2.20902509417425));
#39258=CARTESIAN_POINT('Ctrl Pts',(3.28317133333127,-1.,-2.21109449750638));
#39259=CARTESIAN_POINT('Ctrl Pts',(3.29046159238344,-1.,-2.21311648827391));
#39260=CARTESIAN_POINT('Ctrl Pts',(3.29776825193162,-1.,-2.2150940692337));
#39261=CARTESIAN_POINT('Ctrl Pts',(3.3050948781957,-1.,-2.21703059947837));
#39262=CARTESIAN_POINT('Ctrl Pts',(3.31244421655662,-1.,-2.21892881679083));
#39263=CARTESIAN_POINT('Ctrl Pts',(3.31981686778008,-1.,-2.22078990842768));
#39264=CARTESIAN_POINT('Ctrl Pts',(3.32721196326019,-1.,-2.22261398879623));
#39265=CARTESIAN_POINT('Ctrl Pts',(3.3346277284958,-1.,-2.224400498785));
#39266=CARTESIAN_POINT('Ctrl Pts',(3.34206209449371,-1.,-2.22614863918044));
#39267=CARTESIAN_POINT('Ctrl Pts',(3.34951327111117,-1.,-2.22785777756588));
#39268=CARTESIAN_POINT('Ctrl Pts',(3.35698038165529,-1.,-2.22952789881011));
#39269=CARTESIAN_POINT('Ctrl Pts',(3.36446325227908,-1.,-2.23115945849777));
#39270=CARTESIAN_POINT('Ctrl Pts',(3.37196214349356,-1.,-2.23275319569253));
#39271=CARTESIAN_POINT('Ctrl Pts',(3.37947749555649,-1.,-2.23430995599572));
#39272=CARTESIAN_POINT('Ctrl Pts',(3.38700968549522,-1.,-2.23583052276281));
#39273=CARTESIAN_POINT('Ctrl Pts',(3.39455873448088,-1.,-2.23731541452727));
#39274=CARTESIAN_POINT('Ctrl Pts',(3.40212434705511,-1.,-2.23876491124064));
#39275=CARTESIAN_POINT('Ctrl Pts',(3.40970604190205,-1.,-2.24017914395211));
#39276=CARTESIAN_POINT('Ctrl Pts',(3.41730325539119,-1.,-2.24155816587811));
#39277=CARTESIAN_POINT('Ctrl Pts',(3.42491544683075,-1.,-2.24290202531144));
#39278=CARTESIAN_POINT('Ctrl Pts',(3.43254222615007,-1.,-2.24421085338856));
#39279=CARTESIAN_POINT('Ctrl Pts',(3.44018336460619,-1.,-2.24548487526212));
#39280=CARTESIAN_POINT('Ctrl Pts',(3.44783872863448,-1.,-2.24672437070139));
#39281=CARTESIAN_POINT('Ctrl Pts',(3.45550823512213,-1.,-2.24792964960874));
#39282=CARTESIAN_POINT('Ctrl Pts',(3.46319180177474,-1.,-2.24910102345977));
#39283=CARTESIAN_POINT('Ctrl Pts',(3.47088928979467,-1.,-2.25023877475674));
#39284=CARTESIAN_POINT('Ctrl Pts',(3.47860048448015,-1.,-2.25134314238258));
#39285=CARTESIAN_POINT('Ctrl Pts',(3.48632513240231,-1.,-2.25241433138231));
#39286=CARTESIAN_POINT('Ctrl Pts',(3.49406296494309,-1.,-2.25345251709453));
#39287=CARTESIAN_POINT('Ctrl Pts',(3.50181372618058,-1.,-2.25445785151923));
#39288=CARTESIAN_POINT('Ctrl Pts',(3.50957720118209,-1.,-2.25543046980351));
#39289=CARTESIAN_POINT('Ctrl Pts',(3.51735323669213,-1.,-2.25637049456061));
#39290=CARTESIAN_POINT('Ctrl Pts',(3.52514172849666,-1.,-2.25727802942142));
#39291=CARTESIAN_POINT('Ctrl Pts',(3.53138243689932,-1.,-2.25797812951166));
#39292=CARTESIAN_POINT('Ctrl Pts',(3.53606853163247,-1.,-2.25848864344599));
#39293=CARTESIAN_POINT('Ctrl Pts',(3.5391950664771,-1.,-2.25882251694918));
#39294=CARTESIAN_POINT('Ctrl Pts',(3.54075895182139,-1.,-2.25898783642071));
#39295=CARTESIAN_POINT('',(3.62024382630768,-1.,-2.12928030988903));
#39296=CARTESIAN_POINT('',(3.54075895182139,-1.,-2.25898783642071));
#39297=CARTESIAN_POINT('',(3.29885386921513,-1.,-1.78327315618341));
#39298=CARTESIAN_POINT('Ctrl Pts',(3.62024382630768,-1.,-2.12928030988903));
#39299=CARTESIAN_POINT('Ctrl Pts',(3.61938653648716,-1.,-2.12796193131142));
#39300=CARTESIAN_POINT('Ctrl Pts',(3.61766963589442,-1.,-2.12532774376144));
#39301=CARTESIAN_POINT('Ctrl Pts',(3.61508732215187,-1.,-2.12138417125349));
#39302=CARTESIAN_POINT('Ctrl Pts',(3.61163030607452,-1.,-2.11614149813928));
#39303=CARTESIAN_POINT('Ctrl Pts',(3.60728578530968,-1.,-2.10961391333497));
#39304=CARTESIAN_POINT('Ctrl Pts',(3.60291797087849,-1.,-2.10311217727687));
#39305=CARTESIAN_POINT('Ctrl Pts',(3.59852681775396,-1.,-2.09663642986579));
#39306=CARTESIAN_POINT('Ctrl Pts',(3.5941122862608,-1.,-2.09018686331706));
#39307=CARTESIAN_POINT('Ctrl Pts',(3.58967435355834,-1.,-2.08376373049196));
#39308=CARTESIAN_POINT('Ctrl Pts',(3.58521300039988,-1.,-2.07736732842524));
#39309=CARTESIAN_POINT('Ctrl Pts',(3.58072819250872,-1.,-2.07099797606));
#39310=CARTESIAN_POINT('Ctrl Pts',(3.57621986224402,-1.,-2.06465599229234));
#39311=CARTESIAN_POINT('Ctrl Pts',(3.5716878942334,-1.,-2.05834167687425));
#39312=CARTESIAN_POINT('Ctrl Pts',(3.56713209977904,-1.,-2.05205528172911));
#39313=CARTESIAN_POINT('Ctrl Pts',(3.56255223871505,-1.,-2.04579702158876));
#39314=CARTESIAN_POINT('Ctrl Pts',(3.55794807264844,-1.,-2.03956711119976));
#39315=CARTESIAN_POINT('Ctrl Pts',(3.55331941293949,-1.,-2.03336579658133));
#39316=CARTESIAN_POINT('Ctrl Pts',(3.54866616282227,-1.,-2.02719338376175));
#39317=CARTESIAN_POINT('Ctrl Pts',(3.54398838254136,-1.,-2.02105027983104));
#39318=CARTESIAN_POINT('Ctrl Pts',(3.53928627453642,-1.,-2.01493698847351));
#39319=CARTESIAN_POINT('Ctrl Pts',(3.53456004727424,-1.,-2.00885403604746));
#39320=CARTESIAN_POINT('Ctrl Pts',(3.52980980250224,-1.,-2.00280191090366));
#39321=CARTESIAN_POINT('Ctrl Pts',(3.52503542491728,-1.,-1.99678100339296));
#39322=CARTESIAN_POINT('Ctrl Pts',(3.52023644289142,-1.,-1.99079153006112));
#39323=CARTESIAN_POINT('Ctrl Pts',(3.51541198728301,-1.,-1.9848335106103));
#39324=CARTESIAN_POINT('Ctrl Pts',(3.51056110478287,-1.,-1.97890693666288));
#39325=CARTESIAN_POINT('Ctrl Pts',(3.5056830186108,-1.,-1.97301191162968));
#39326=CARTESIAN_POINT('Ctrl Pts',(3.50077740176267,-1.,-1.96714879724052));
#39327=CARTESIAN_POINT('Ctrl Pts',(3.49584466573064,-1.,-1.961318367765));
#39328=CARTESIAN_POINT('Ctrl Pts',(3.49088618670987,-1.,-1.95552193112084));
#39329=CARTESIAN_POINT('Ctrl Pts',(3.48590361610814,-1.,-1.94976096795911));
#39330=CARTESIAN_POINT('Ctrl Pts',(3.48089825770416,-1.,-1.94403680554065));
#39331=CARTESIAN_POINT('Ctrl Pts',(3.47587040389915,-1.,-1.93835026973887));
#39332=CARTESIAN_POINT('Ctrl Pts',(3.47081872409781,-1.,-1.93270136427081));
#39333=CARTESIAN_POINT('Ctrl Pts',(3.46573953254084,-1.,-1.92708888591158));
#39334=CARTESIAN_POINT('Ctrl Pts',(3.46062821722485,-1.,-1.92151118213212));
#39335=CARTESIAN_POINT('Ctrl Pts',(3.4554807430995,-1.,-1.91596694784064));
#39336=CARTESIAN_POINT('Ctrl Pts',(3.45029522038888,-1.,-1.91045605593639));
#39337=CARTESIAN_POINT('Ctrl Pts',(3.44507323983367,-1.,-1.90498026502305));
#39338=CARTESIAN_POINT('Ctrl Pts',(3.4398218567809,-1.,-1.89954426803384));
#39339=CARTESIAN_POINT('Ctrl Pts',(3.43455074411571,-1.,-1.89415420002542));
#39340=CARTESIAN_POINT('Ctrl Pts',(3.42926852222158,-1.,-1.88881571322009));
#39341=CARTESIAN_POINT('Ctrl Pts',(3.42397908819736,-1.,-1.8835320506206));
#39342=CARTESIAN_POINT('Ctrl Pts',(3.41867858383771,-1.,-1.87830245689344));
#39343=CARTESIAN_POINT('Ctrl Pts',(3.41335043875209,-1.,-1.87311957248121));
#39344=CARTESIAN_POINT('Ctrl Pts',(3.40797080000549,-1.,-1.86797231196654));
#39345=CARTESIAN_POINT('Ctrl Pts',(3.40251742305476,-1.,-1.86285057051245));
#39346=CARTESIAN_POINT('Ctrl Pts',(3.39697816833067,-1.,-1.85774972037062));
#39347=CARTESIAN_POINT('Ctrl Pts',(3.39135802549398,-1.,-1.85267433291769));
#39348=CARTESIAN_POINT('Ctrl Pts',(3.38569092349592,-1.,-1.84764441927753));
#39349=CARTESIAN_POINT('Ctrl Pts',(3.38002968341157,-1.,-1.84269016931643));
#39350=CARTESIAN_POINT('Ctrl Pts',(3.37442462015853,-1.,-1.83784072967077));
#39351=CARTESIAN_POINT('Ctrl Pts',(3.36890396271836,-1.,-1.83311391452322));
#39352=CARTESIAN_POINT('Ctrl Pts',(3.36345722124158,-1.,-1.82850752153199));
#39353=CARTESIAN_POINT('Ctrl Pts',(3.35800801557424,-1.,-1.82398496829301));
#39354=CARTESIAN_POINT('Ctrl Pts',(3.35243086937598,-1.,-1.81948458796829));
#39355=CARTESIAN_POINT('Ctrl Pts',(3.34660014370673,-1.,-1.81494618732853));
#39356=CARTESIAN_POINT('Ctrl Pts',(3.34043216147606,-1.,-1.81033399625352));
#39357=CARTESIAN_POINT('Ctrl Pts',(3.33392460276808,-1.,-1.80565802981102));
#39358=CARTESIAN_POINT('Ctrl Pts',(3.32721088039578,-1.,-1.80100380443406));
#39359=CARTESIAN_POINT('Ctrl Pts',(3.3205535510082,-1.,-1.79652817033251));
#39360=CARTESIAN_POINT('Ctrl Pts',(3.31428038326424,-1.,-1.79242331349949));
#39361=CARTESIAN_POINT('Ctrl Pts',(3.30873412266788,-1.,-1.78888832245873));
#39362=CARTESIAN_POINT('Ctrl Pts',(3.30422155559112,-1.,-1.78610045419846));
#39363=CARTESIAN_POINT('Ctrl Pts',(3.30119637003393,-1.,-1.78432384788174));
#39364=CARTESIAN_POINT('Ctrl Pts',(3.299705498242,-1.,-1.78353803106924));
#39365=CARTESIAN_POINT('Ctrl Pts',(3.29909749657808,-1.,-1.78329283591905));
#39366=CARTESIAN_POINT('Ctrl Pts',(3.29890219175423,-1.,-1.78326534445518));
#39367=CARTESIAN_POINT('Ctrl Pts',(3.29885386921513,-1.,-1.78327315618341));
#39368=CARTESIAN_POINT('',(3.38171594275687,-1.,-1.62064718014256));
#39369=CARTESIAN_POINT('Origin',(0.,-1.,0.));
#39370=CARTESIAN_POINT('',(3.85054988729471,-1.,-1.67727921511438));
#39371=CARTESIAN_POINT('Ctrl Pts',(3.38171594275687,-1.,-1.62064718014256));
#39372=CARTESIAN_POINT('Ctrl Pts',(3.38173802621242,-1.,-1.62069086551626));
#39373=CARTESIAN_POINT('Ctrl Pts',(3.38187506457001,-1.,-1.62083271136059));
#39374=CARTESIAN_POINT('Ctrl Pts',(3.38243080602536,-1.,-1.62118047294574));
#39375=CARTESIAN_POINT('Ctrl Pts',(3.3839428576331,-1.,-1.62192472202795));
#39376=CARTESIAN_POINT('Ctrl Pts',(3.38715832178929,-1.,-1.62332788556183));
#39377=CARTESIAN_POINT('Ctrl Pts',(3.39206617497078,-1.,-1.62533996116793));
#39378=CARTESIAN_POINT('Ctrl Pts',(3.39818605298342,-1.,-1.62774916464571));
#39379=CARTESIAN_POINT('Ctrl Pts',(3.40519422740596,-1.,-1.63041148964996));
#39380=CARTESIAN_POINT('Ctrl Pts',(3.41272817148719,-1.,-1.63316667054156));
#39381=CARTESIAN_POINT('Ctrl Pts',(3.4204397459095,-1.,-1.63586250099804));
#39382=CARTESIAN_POINT('Ctrl Pts',(3.42804772926213,-1.,-1.6383787624689));
#39383=CARTESIAN_POINT('Ctrl Pts',(3.43540451921397,-1.,-1.64065778701952));
#39384=CARTESIAN_POINT('Ctrl Pts',(3.44250337701736,-1.,-1.64270733821042));
#39385=CARTESIAN_POINT('Ctrl Pts',(3.44942242546693,-1.,-1.64457408708059));
#39386=CARTESIAN_POINT('Ctrl Pts',(3.4562842106239,-1.,-1.64632429697506));
#39387=CARTESIAN_POINT('Ctrl Pts',(3.46321237515029,-1.,-1.64802323352752));
#39388=CARTESIAN_POINT('Ctrl Pts',(3.47028140996055,-1.,-1.64971118698285));
#39389=CARTESIAN_POINT('Ctrl Pts',(3.47749926256543,-1.,-1.65139534930353));
#39390=CARTESIAN_POINT('Ctrl Pts',(3.48483492840942,-1.,-1.65306335367762));
#39391=CARTESIAN_POINT('Ctrl Pts',(3.49223525300194,-1.,-1.65469162644476));
#39392=CARTESIAN_POINT('Ctrl Pts',(3.49964476477929,-1.,-1.65625517961583));
#39393=CARTESIAN_POINT('Ctrl Pts',(3.5070273314651,-1.,-1.65773832633617));
#39394=CARTESIAN_POINT('Ctrl Pts',(3.51437632188903,-1.,-1.65913971687324));
#39395=CARTESIAN_POINT('Ctrl Pts',(3.52170261543787,-1.,-1.66046645222266));
#39396=CARTESIAN_POINT('Ctrl Pts',(3.52902746211081,-1.,-1.66173058912365));
#39397=CARTESIAN_POINT('Ctrl Pts',(3.53637385060225,-1.,-1.66294490916113));
#39398=CARTESIAN_POINT('Ctrl Pts',(3.5437574747503,-1.,-1.66411849222334));
#39399=CARTESIAN_POINT('Ctrl Pts',(3.5511812134288,-1.,-1.66525401569004));
#39400=CARTESIAN_POINT('Ctrl Pts',(3.55864015233617,-1.,-1.66635023293121));
#39401=CARTESIAN_POINT('Ctrl Pts',(3.56612465179429,-1.,-1.66740349220308));
#39402=CARTESIAN_POINT('Ctrl Pts',(3.57362406285884,-1.,-1.66840957407299));
#39403=CARTESIAN_POINT('Ctrl Pts',(3.58113044183823,-1.,-1.66936552908228));
#39404=CARTESIAN_POINT('Ctrl Pts',(3.5886414309783,-1.,-1.67027110397602));
#39405=CARTESIAN_POINT('Ctrl Pts',(3.59615824388808,-1.,-1.67112775290706));
#39406=CARTESIAN_POINT('Ctrl Pts',(3.60368430815203,-1.,-1.67193797318598));
#39407=CARTESIAN_POINT('Ctrl Pts',(3.61122367156182,-1.,-1.67270452466968));
#39408=CARTESIAN_POINT('Ctrl Pts',(3.61877947398179,-1.,-1.67342968196223));
#39409=CARTESIAN_POINT('Ctrl Pts',(3.62635249450908,-1.,-1.67411452372265));
#39410=CARTESIAN_POINT('Ctrl Pts',(3.63394189312902,-1.,-1.67475929882962));
#39411=CARTESIAN_POINT('Ctrl Pts',(3.6415458297232,-1.,-1.6753637326484));
#39412=CARTESIAN_POINT('Ctrl Pts',(3.64916213574663,-1.,-1.6759273594669));
#39413=CARTESIAN_POINT('Ctrl Pts',(3.65678894416442,-1.,-1.67644983469459));
#39414=CARTESIAN_POINT('Ctrl Pts',(3.66442538671018,-1.,-1.67693128053153));
#39415=CARTESIAN_POINT('Ctrl Pts',(3.67207136294639,-1.,-1.67737217414901));
#39416=CARTESIAN_POINT('Ctrl Pts',(3.6797272457918,-1.,-1.67777320475872));
#39417=CARTESIAN_POINT('Ctrl Pts',(3.68739360236505,-1.,-1.67813513867973));
#39418=CARTESIAN_POINT('Ctrl Pts',(3.69507092759545,-1.,-1.67845869064304));
#39419=CARTESIAN_POINT('Ctrl Pts',(3.70275932350998,-1.,-1.6787443694862));
#39420=CARTESIAN_POINT('Ctrl Pts',(3.71045854208195,-1.,-1.67899249793398));
#39421=CARTESIAN_POINT('Ctrl Pts',(3.71816812842188,-1.,-1.6792032807165));
#39422=CARTESIAN_POINT('Ctrl Pts',(3.72588753416339,-1.,-1.67937685856627));
#39423=CARTESIAN_POINT('Ctrl Pts',(3.73361623282617,-1.,-1.67951336376434));
#39424=CARTESIAN_POINT('Ctrl Pts',(3.74135385965622,-1.,-1.67961298685316));
#39425=CARTESIAN_POINT('Ctrl Pts',(3.74910022394845,-1.,-1.67967598599665));
#39426=CARTESIAN_POINT('Ctrl Pts',(3.75685523754816,-1.,-1.67970265841379));
#39427=CARTESIAN_POINT('Ctrl Pts',(3.76461886684523,-1.,-1.67969332319322));
#39428=CARTESIAN_POINT('Ctrl Pts',(3.77239107928394,-1.,-1.67964830084946));
#39429=CARTESIAN_POINT('Ctrl Pts',(3.78017178196859,-1.,-1.67956789211943));
#39430=CARTESIAN_POINT('Ctrl Pts',(3.78796080021026,-1.,-1.67945236653175));
#39431=CARTESIAN_POINT('Ctrl Pts',(3.7957579157763,-1.,-1.67930196625204));
#39432=CARTESIAN_POINT('Ctrl Pts',(3.80356289078481,-1.,-1.67911690648128));
#39433=CARTESIAN_POINT('Ctrl Pts',(3.81137549624273,-1.,-1.67889737738311));
#39434=CARTESIAN_POINT('Ctrl Pts',(3.81919554100522,-1.,-1.67864354606363));
#39435=CARTESIAN_POINT('Ctrl Pts',(3.82702289288453,-1.,-1.67835555760094));
#39436=CARTESIAN_POINT('Ctrl Pts',(3.83485746516115,-1.,-1.67803353065273));
#39437=CARTESIAN_POINT('Ctrl Pts',(3.8411308598706,-1.,-1.67774874946867));
#39438=CARTESIAN_POINT('Ctrl Pts',(3.84583912297567,-1.,-1.67751991140661));
#39439=CARTESIAN_POINT('Ctrl Pts',(3.84897939431104,-1.,-1.6773605765671));
#39440=CARTESIAN_POINT('Ctrl Pts',(3.85054988729471,-1.,-1.67727921511438));
#39441=CARTESIAN_POINT('',(3.90876544355381,-1.,-1.53673442965256));
#39442=CARTESIAN_POINT('',(3.85054988729471,-1.,-1.67727921511438));
#39443=CARTESIAN_POINT('',(3.5372048861591,-1.,-1.24526366418208));
#39444=CARTESIAN_POINT('Ctrl Pts',(3.90876544355381,-1.,-1.53673442965256));
#39445=CARTESIAN_POINT('Ctrl Pts',(3.90771246854607,-1.,-1.53556639217742));
#39446=CARTESIAN_POINT('Ctrl Pts',(3.90560462812846,-1.,-1.53323321827311));
#39447=CARTESIAN_POINT('Ctrl Pts',(3.90243719629755,-1.,-1.5297421605556));
#39448=CARTESIAN_POINT('Ctrl Pts',(3.8982026070607,-1.,-1.52510482990784));
#39449=CARTESIAN_POINT('Ctrl Pts',(3.89289043531893,-1.,-1.51933724328609));
#39450=CARTESIAN_POINT('Ctrl Pts',(3.88755930032927,-1.,-1.51359883110181));
#39451=CARTESIAN_POINT('Ctrl Pts',(3.88220917950443,-1.,-1.50788973857719));
#39452=CARTESIAN_POINT('Ctrl Pts',(3.87684006372665,-1.,-1.50221016176766));
#39453=CARTESIAN_POINT('Ctrl Pts',(3.8714519699927,-1.,-1.4965603539944));
#39454=CARTESIAN_POINT('Ctrl Pts',(3.86604492575933,-1.,-1.49094061164604));
#39455=CARTESIAN_POINT('Ctrl Pts',(3.86061894706551,-1.,-1.48535125510102));
#39456=CARTESIAN_POINT('Ctrl Pts',(3.85517401698952,-1.,-1.47979260991063));
#39457=CARTESIAN_POINT('Ctrl Pts',(3.84971006847096,-1.,-1.47426499018467));
#39458=CARTESIAN_POINT('Ctrl Pts',(3.84422695454469,-1.,-1.46876867426375));
#39459=CARTESIAN_POINT('Ctrl Pts',(3.83872447159309,-1.,-1.46330391180621));
#39460=CARTESIAN_POINT('Ctrl Pts',(3.83320241775199,-1.,-1.45787095220763));
#39461=CARTESIAN_POINT('Ctrl Pts',(3.82766064519,-1.,-1.45247006796807));
#39462=CARTESIAN_POINT('Ctrl Pts',(3.82209910620591,-1.,-1.44710157648562));
#39463=CARTESIAN_POINT('Ctrl Pts',(3.8165179239855,-1.,-1.44176587041401));
#39464=CARTESIAN_POINT('Ctrl Pts',(3.81091737726965,-1.,-1.43646341556783));
#39465=CARTESIAN_POINT('Ctrl Pts',(3.80529775429916,-1.,-1.43119469921364));
#39466=CARTESIAN_POINT('Ctrl Pts',(3.79965923196365,-1.,-1.42596018777301));
#39467=CARTESIAN_POINT('Ctrl Pts',(3.7940017574439,-1.,-1.42076028482828));
#39468=CARTESIAN_POINT('Ctrl Pts',(3.78832489879369,-1.,-1.41559527803808));
#39469=CARTESIAN_POINT('Ctrl Pts',(3.78262780065406,-1.,-1.41046532282567));
#39470=CARTESIAN_POINT('Ctrl Pts',(3.77690952014209,-1.,-1.40537056004702));
#39471=CARTESIAN_POINT('Ctrl Pts',(3.77116930621804,-1.,-1.40031121335495));
#39472=CARTESIAN_POINT('Ctrl Pts',(3.76540689249078,-1.,-1.39528769118054));
#39473=CARTESIAN_POINT('Ctrl Pts',(3.75962280650875,-1.,-1.39030069388926));
#39474=CARTESIAN_POINT('Ctrl Pts',(3.75381861212728,-1.,-1.38535129801185));
#39475=CARTESIAN_POINT('Ctrl Pts',(3.74799617204744,-1.,-1.38044070763302));
#39476=CARTESIAN_POINT('Ctrl Pts',(3.7421569816256,-1.,-1.3755700297169));
#39477=CARTESIAN_POINT('Ctrl Pts',(3.73630145885809,-1.,-1.37074003422739));
#39478=CARTESIAN_POINT('Ctrl Pts',(3.73042829011293,-1.,-1.36595093298674));
#39479=CARTESIAN_POINT('Ctrl Pts',(3.72453364678279,-1.,-1.36120211416354));
#39480=CARTESIAN_POINT('Ctrl Pts',(3.71861271513318,-1.,-1.35649266705038));
#39481=CARTESIAN_POINT('Ctrl Pts',(3.71266130563061,-1.,-1.35182193384426));
#39482=CARTESIAN_POINT('Ctrl Pts',(3.7066775318825,-1.,-1.34719008463535));
#39483=CARTESIAN_POINT('Ctrl Pts',(3.70066324015112,-1.,-1.3425986075293));
#39484=CARTESIAN_POINT('Ctrl Pts',(3.69462613305692,-1.,-1.33805103398214));
#39485=CARTESIAN_POINT('Ctrl Pts',(3.68857672413013,-1.,-1.33355191034515));
#39486=CARTESIAN_POINT('Ctrl Pts',(3.68252441182534,-1.,-1.32910547072734));
#39487=CARTESIAN_POINT('Ctrl Pts',(3.67647355257906,-1.,-1.32471430856413));
#39488=CARTESIAN_POINT('Ctrl Pts',(3.67042021752668,-1.,-1.3203782813777));
#39489=CARTESIAN_POINT('Ctrl Pts',(3.66434688899822,-1.,-1.31609271239922));
#39490=CARTESIAN_POINT('Ctrl Pts',(3.65822827358655,-1.,-1.31185038411231));
#39491=CARTESIAN_POINT('Ctrl Pts',(3.65204081987101,-1.,-1.30764479590051));
#39492=CARTESIAN_POINT('Ctrl Pts',(3.64577181380125,-1.,-1.30347327603778));
#39493=CARTESIAN_POINT('Ctrl Pts',(3.6394268987279,-1.,-1.29933955906463));
#39494=CARTESIAN_POINT('Ctrl Pts',(3.63304271630995,-1.,-1.29525810207744));
#39495=CARTESIAN_POINT('Ctrl Pts',(3.62667616004299,-1.,-1.29125046021853));
#39496=CARTESIAN_POINT('Ctrl Pts',(3.62038148492295,-1.,-1.2873375502936));
#39497=CARTESIAN_POINT('Ctrl Pts',(3.61418935913793,-1.,-1.28353255117754));
#39498=CARTESIAN_POINT('Ctrl Pts',(3.60808907746372,-1.,-1.27983492861703));
#39499=CARTESIAN_POINT('Ctrl Pts',(3.60199947736404,-1.,-1.27622049908664));
#39500=CARTESIAN_POINT('Ctrl Pts',(3.59578698050164,-1.,-1.27264798379365));
#39501=CARTESIAN_POINT('Ctrl Pts',(3.5893180784647,-1.,-1.26907758484766));
#39502=CARTESIAN_POINT('Ctrl Pts',(3.58250452868699,-1.,-1.26548706249891));
#39503=CARTESIAN_POINT('Ctrl Pts',(3.5753456065164,-1.,-1.26188667142784));
#39504=CARTESIAN_POINT('Ctrl Pts',(3.56798645995025,-1.,-1.25834000485626));
#39505=CARTESIAN_POINT('Ctrl Pts',(3.56071094990825,-1.,-1.25496090899873));
#39506=CARTESIAN_POINT('Ctrl Pts',(3.5538728741862,-1.,-1.25188792940508));
#39507=CARTESIAN_POINT('Ctrl Pts',(3.54784190282889,-1.,-1.24926408627938));
#39508=CARTESIAN_POINT('Ctrl Pts',(3.54294877426113,-1.,-1.2472164623202));
#39509=CARTESIAN_POINT('Ctrl Pts',(3.53968291129942,-1.,-1.24593497225964));
#39510=CARTESIAN_POINT('Ctrl Pts',(3.53808746578052,-1.,-1.2453920538873));
#39511=CARTESIAN_POINT('Ctrl Pts',(3.53744859265385,-1.,-1.24524498991133));
#39512=CARTESIAN_POINT('Ctrl Pts',(3.53725139174402,-1.,-1.24524838931864));
#39513=CARTESIAN_POINT('Ctrl Pts',(3.5372048861591,-1.,-1.24526366418208));
#39514=CARTESIAN_POINT('',(3.59360648251021,-1.,-1.071677399622));
#39515=CARTESIAN_POINT('Origin',(0.,-1.,0.));
#39516=CARTESIAN_POINT('',(4.06552750530042,-1.,-1.05427041296137));
#39517=CARTESIAN_POINT('Ctrl Pts',(3.59360648251021,-1.,-1.071677399622));
#39518=CARTESIAN_POINT('Ctrl Pts',(3.59363512797985,-1.,-1.07171709254271));
#39519=CARTESIAN_POINT('Ctrl Pts',(3.59379266874663,-1.,-1.07183575450716));
#39520=CARTESIAN_POINT('Ctrl Pts',(3.59439597,-1.,-1.07209229745284));
#39521=CARTESIAN_POINT('Ctrl Pts',(3.59600583195037,-1.,-1.07259084660947));
#39522=CARTESIAN_POINT('Ctrl Pts',(3.59940121154383,-1.,-1.0734737254567));
#39523=CARTESIAN_POINT('Ctrl Pts',(3.6045633988796,-1.,-1.0746932716863));
#39524=CARTESIAN_POINT('Ctrl Pts',(3.61098481349577,-1.,-1.07611545402841));
#39525=CARTESIAN_POINT('Ctrl Pts',(3.61832318504957,-1.,-1.07764868137729));
#39526=CARTESIAN_POINT('Ctrl Pts',(3.62619537902616,-1.,-1.07919137290816));
#39527=CARTESIAN_POINT('Ctrl Pts',(3.63423373196602,-1.,-1.08064765719887));
#39528=CARTESIAN_POINT('Ctrl Pts',(3.64214167843595,-1.,-1.08194278850972));
#39529=CARTESIAN_POINT('Ctrl Pts',(3.64976441208197,-1.,-1.08304289898577));
#39530=CARTESIAN_POINT('Ctrl Pts',(3.65709649161004,-1.,-1.08395671077761));
#39531=CARTESIAN_POINT('Ctrl Pts',(3.66422237895256,-1.,-1.0847180992287));
#39532=CARTESIAN_POINT('Ctrl Pts',(3.67127347729632,-1.,-1.0853733414448));
#39533=CARTESIAN_POINT('Ctrl Pts',(3.67838211685148,-1.,-1.08596755755768));
#39534=CARTESIAN_POINT('Ctrl Pts',(3.68562817420864,-1.,-1.08652888882609));
#39535=CARTESIAN_POINT('Ctrl Pts',(3.69302062410229,-1.,-1.08706319540292));
#39536=CARTESIAN_POINT('Ctrl Pts',(3.70052690909884,-1.,-1.08756311291324));
#39537=CARTESIAN_POINT('Ctrl Pts',(3.70809084139476,-1.,-1.0880136731219));
#39538=CARTESIAN_POINT('Ctrl Pts',(3.71565372339063,-1.,-1.08839887334777));
#39539=CARTESIAN_POINT('Ctrl Pts',(3.72317741369364,-1.,-1.08870887220072));
#39540=CARTESIAN_POINT('Ctrl Pts',(3.73065515162949,-1.,-1.08894337390925));
#39541=CARTESIAN_POINT('Ctrl Pts',(3.73809879348209,-1.,-1.08910769013288));
#39542=CARTESIAN_POINT('Ctrl Pts',(3.74553121371745,-1.,-1.08921040494013));
#39543=CARTESIAN_POINT('Ctrl Pts',(3.75297711748138,-1.,-1.08926054632927));
#39544=CARTESIAN_POINT('Ctrl Pts',(3.76045342580226,-1.,-1.08926462734287));
#39545=CARTESIAN_POINT('Ctrl Pts',(3.76796340094469,-1.,-1.08922484204263));
#39546=CARTESIAN_POINT('Ctrl Pts',(3.7755019940944,-1.,-1.08914072791275));
#39547=CARTESIAN_POINT('Ctrl Pts',(3.78305911299511,-1.,-1.08901018614638));
#39548=CARTESIAN_POINT('Ctrl Pts',(3.79062357974401,-1.,-1.08883071512097));
#39549=CARTESIAN_POINT('Ctrl Pts',(3.79818708705252,-1.,-1.08860064435776));
#39550=CARTESIAN_POINT('Ctrl Pts',(3.80574726657656,-1.,-1.08832009255378));
#39551=CARTESIAN_POINT('Ctrl Pts',(3.81330554446324,-1.,-1.08799030610861));
#39552=CARTESIAN_POINT('Ctrl Pts',(3.82086569676321,-1.,-1.08761321539442));
#39553=CARTESIAN_POINT('Ctrl Pts',(3.82843215316985,-1.,-1.08719091307558));
#39554=CARTESIAN_POINT('Ctrl Pts',(3.83600837071702,-1.,-1.08672515456901));
#39555=CARTESIAN_POINT('Ctrl Pts',(3.84359528764934,-1.,-1.08621688337601));
#39556=CARTESIAN_POINT('Ctrl Pts',(3.85119211322732,-1.,-1.08566647671838));
#39557=CARTESIAN_POINT('Ctrl Pts',(3.85879698702511,-1.,-1.08507395120054));
#39558=CARTESIAN_POINT('Ctrl Pts',(3.86640769434269,-1.,-1.08443918607926));
#39559=CARTESIAN_POINT('Ctrl Pts',(3.87402233722563,-1.,-1.0837621330751));
#39560=CARTESIAN_POINT('Ctrl Pts',(3.88164007721365,-1.,-1.08304304871042));
#39561=CARTESIAN_POINT('Ctrl Pts',(3.88926088975182,-1.,-1.08228241999363));
#39562=CARTESIAN_POINT('Ctrl Pts',(3.89688525098408,-1.,-1.08148086931373));
#39563=CARTESIAN_POINT('Ctrl Pts',(3.90451384092564,-1.,-1.08063906483823));
#39564=CARTESIAN_POINT('Ctrl Pts',(3.91214726022096,-1.,-1.0797576350746));
#39565=CARTESIAN_POINT('Ctrl Pts',(3.91978568924062,-1.,-1.07883706663524));
#39566=CARTESIAN_POINT('Ctrl Pts',(3.92742893349684,-1.,-1.07787771707155));
#39567=CARTESIAN_POINT('Ctrl Pts',(3.93507657572743,-1.,-1.07687985975348));
#39568=CARTESIAN_POINT('Ctrl Pts',(3.94272809633271,-1.,-1.07584371946428));
#39569=CARTESIAN_POINT('Ctrl Pts',(3.95038299600754,-1.,-1.07476950921607));
#39570=CARTESIAN_POINT('Ctrl Pts',(3.95804094429606,-1.,-1.07365747426551));
#39571=CARTESIAN_POINT('Ctrl Pts',(3.96570179322681,-1.,-1.07250789943095));
#39572=CARTESIAN_POINT('Ctrl Pts',(3.97336550222571,-1.,-1.07132109206252));
#39573=CARTESIAN_POINT('Ctrl Pts',(3.98103208801289,-1.,-1.07009737257815));
#39574=CARTESIAN_POINT('Ctrl Pts',(3.98870156857298,-1.,-1.06883706263912));
#39575=CARTESIAN_POINT('Ctrl Pts',(3.99637389919958,-1.,-1.06754047381188));
#39576=CARTESIAN_POINT('Ctrl Pts',(4.00404894951804,-1.,-1.06620789963406));
#39577=CARTESIAN_POINT('Ctrl Pts',(4.0117265418656,-1.,-1.06483961342894));
#39578=CARTESIAN_POINT('Ctrl Pts',(4.0194064749539,-1.,-1.06343586496094));
#39579=CARTESIAN_POINT('Ctrl Pts',(4.02708855235732,-1.,-1.06199687787488));
#39580=CARTESIAN_POINT('Ctrl Pts',(4.03477261142549,-1.,-1.06052284712114));
#39581=CARTESIAN_POINT('Ctrl Pts',(4.04245854429333,-1.,-1.0590139366704));
#39582=CARTESIAN_POINT('Ctrl Pts',(4.05014628387112,-1.,-1.05747027728537));
#39583=CARTESIAN_POINT('Ctrl Pts',(4.05629789308941,-1.,-1.0562076270849));
#39584=CARTESIAN_POINT('Ctrl Pts',(4.06091239150293,-1.,-1.05524507177901));
#39585=CARTESIAN_POINT('Ctrl Pts',(4.06398907542679,-1.,-1.05459645194934));
#39586=CARTESIAN_POINT('Ctrl Pts',(4.06552750530042,-1.,-1.05427041296137));
#39587=CARTESIAN_POINT('',(4.10104028313088,-1.,-0.906349047628866));
#39588=CARTESIAN_POINT('',(4.06552750530042,-1.,-1.05427041296137));
#39589=CARTESIAN_POINT('',(3.68845817949586,-1.,-0.676591647975429));
#39590=CARTESIAN_POINT('Ctrl Pts',(4.10104028313088,-1.,-0.906349047628866));
#39591=CARTESIAN_POINT('Ctrl Pts',(4.09981755067523,-1.,-0.905360112215337));
#39592=CARTESIAN_POINT('Ctrl Pts',(4.09737067245935,-1.,-0.903385402441588));
#39593=CARTESIAN_POINT('Ctrl Pts',(4.09369611522387,-1.,-0.900432820941675));
#39594=CARTESIAN_POINT('Ctrl Pts',(4.08878822246833,-1.,-0.896515019231334));
#39595=CARTESIAN_POINT('Ctrl Pts',(4.08263920304799,-1.,-0.891649447916278));
#39596=CARTESIAN_POINT('Ctrl Pts',(4.07647601773635,-1.,-0.886815658358501));
#39597=CARTESIAN_POINT('Ctrl Pts',(4.07029866694192,-1.,-0.882013797525692));
#39598=CARTESIAN_POINT('Ctrl Pts',(4.06410717232905,-1.,-0.877244060485838));
#39599=CARTESIAN_POINT('Ctrl Pts',(4.0579015903134,-1.,-0.872506694782446));
#39600=CARTESIAN_POINT('Ctrl Pts',(4.05168199437909,-1.,-0.867801988859918));
#39601=CARTESIAN_POINT('Ctrl Pts',(4.04544845048584,-1.,-0.863130256643259));
#39602=CARTESIAN_POINT('Ctrl Pts',(4.03920099284773,-1.,-0.858491822322828));
#39603=CARTESIAN_POINT('Ctrl Pts',(4.03293960436756,-1.,-0.853887006631755));
#39604=CARTESIAN_POINT('Ctrl Pts',(4.02666418343164,-1.,-0.849316107474245));
#39605=CARTESIAN_POINT('Ctrl Pts',(4.02037456798441,-1.,-0.844779403287746));
#39606=CARTESIAN_POINT('Ctrl Pts',(4.01407059766103,-1.,-0.840277171975855));
#39607=CARTESIAN_POINT('Ctrl Pts',(4.00775216907856,-1.,-0.835809705809646));
#39608=CARTESIAN_POINT('Ctrl Pts',(4.00141928477507,-1.,-0.831377325741623));
#39609=CARTESIAN_POINT('Ctrl Pts',(3.99507212784431,-1.,-0.82698040032079));
#39610=CARTESIAN_POINT('Ctrl Pts',(3.98871104646485,-1.,-0.822619346022119));
#39611=CARTESIAN_POINT('Ctrl Pts',(3.98233640155404,-1.,-0.818294599022294));
#39612=CARTESIAN_POINT('Ctrl Pts',(3.97594844078811,-1.,-0.814006592328844));
#39613=CARTESIAN_POINT('Ctrl Pts',(3.96954717513232,-1.,-0.809755732818091));
#39614=CARTESIAN_POINT('Ctrl Pts',(3.96313222295815,-1.,-0.805542372178362));
#39615=CARTESIAN_POINT('Ctrl Pts',(3.95670276375108,-1.,-0.80136679772705));
#39616=CARTESIAN_POINT('Ctrl Pts',(3.95025788827136,-1.,-0.797229296085316));
#39617=CARTESIAN_POINT('Ctrl Pts',(3.94379688971283,-1.,-0.793130205640961));
#39618=CARTESIAN_POINT('Ctrl Pts',(3.93731956885676,-1.,-0.789069971469333));
#39619=CARTESIAN_POINT('Ctrl Pts',(3.93082655631789,-1.,-0.785049202786508));
#39620=CARTESIAN_POINT('Ctrl Pts',(3.92431956510441,-1.,-0.781068718228451));
#39621=CARTESIAN_POINT('Ctrl Pts',(3.9178006233448,-1.,-0.777129415664956));
#39622=CARTESIAN_POINT('Ctrl Pts',(3.91127138115243,-1.,-0.773232154506321));
#39623=CARTESIAN_POINT('Ctrl Pts',(3.90473237182633,-1.,-0.769377629847874));
#39624=CARTESIAN_POINT('Ctrl Pts',(3.89818233104378,-1.,-0.765566256401296));
#39625=CARTESIAN_POINT('Ctrl Pts',(3.89161738162245,-1.,-0.76179802879397));
#39626=CARTESIAN_POINT('Ctrl Pts',(3.88503262662689,-1.,-0.758072800564801));
#39627=CARTESIAN_POINT('Ctrl Pts',(3.87842382520065,-1.,-0.754390577396857));
#39628=CARTESIAN_POINT('Ctrl Pts',(3.87178914078374,-1.,-0.750751822383028));
#39629=CARTESIAN_POINT('Ctrl Pts',(3.86513062969889,-1.,-0.747157716488871));
#39630=CARTESIAN_POINT('Ctrl Pts',(3.85845645217594,-1.,-0.743610542737013));
#39631=CARTESIAN_POINT('Ctrl Pts',(3.85177770351215,-1.,-0.740113146827137));
#39632=CARTESIAN_POINT('Ctrl Pts',(3.84510432881213,-1.,-0.736668240497118));
#39633=CARTESIAN_POINT('Ctrl Pts',(3.83844103658009,-1.,-0.733277703756078));
#39634=CARTESIAN_POINT('Ctrl Pts',(3.83178392403383,-1.,-0.729942010490168));
#39635=CARTESIAN_POINT('Ctrl Pts',(3.82511495756713,-1.,-0.726659281876664));
#39636=CARTESIAN_POINT('Ctrl Pts',(3.81840802610835,-1.,-0.723426346019423));
#39637=CARTESIAN_POINT('Ctrl Pts',(3.81163885127344,-1.,-0.720240466589236));
#39638=CARTESIAN_POINT('Ctrl Pts',(3.80479445759309,-1.,-0.717100993669115));
#39639=CARTESIAN_POINT('Ctrl Pts',(3.79788100314975,-1.,-0.714010733006641));
#39640=CARTESIAN_POINT('Ctrl Pts',(3.79093694007094,-1.,-0.710978231689017));
#39641=CARTESIAN_POINT('Ctrl Pts',(3.78402183336605,-1.,-0.708015879375459));
#39642=CARTESIAN_POINT('Ctrl Pts',(3.77719254217129,-1.,-0.705135847999817));
#39643=CARTESIAN_POINT('Ctrl Pts',(3.77048141872872,-1.,-0.702346356621552));
#39644=CARTESIAN_POINT('Ctrl Pts',(3.76387780603759,-1.,-0.699648552230917));
#39645=CARTESIAN_POINT('Ctrl Pts',(3.75729775767023,-1.,-0.697031245659744));
#39646=CARTESIAN_POINT('Ctrl Pts',(3.75060288243455,-1.,-0.694474562581493));
#39647=CARTESIAN_POINT('Ctrl Pts',(3.74365508986712,-1.,-0.69196008040082));
#39648=CARTESIAN_POINT('Ctrl Pts',(3.73636374475077,-1.,-0.689479637354814));
#39649=CARTESIAN_POINT('Ctrl Pts',(3.72872973554051,-1.,-0.687043475232355));
#39650=CARTESIAN_POINT('Ctrl Pts',(3.7209063713926,-1.,-0.684691698167848));
#39651=CARTESIAN_POINT('Ctrl Pts',(3.71319182789943,-1.,-0.68249234510893));
#39652=CARTESIAN_POINT('Ctrl Pts',(3.70595722031785,-1.,-0.680526909710877));
#39653=CARTESIAN_POINT('Ctrl Pts',(3.69959004073005,-1.,-0.678878822226027));
#39654=CARTESIAN_POINT('Ctrl Pts',(3.69443683573598,-1.,-0.677621861865498));
#39655=CARTESIAN_POINT('Ctrl Pts',(3.69101071175464,-1.,-0.676867042599402));
#39656=CARTESIAN_POINT('Ctrl Pts',(3.68934997767243,-1.,-0.676580391119396));
#39657=CARTESIAN_POINT('Ctrl Pts',(3.68869596425969,-1.,-0.676535079520807));
#39658=CARTESIAN_POINT('Ctrl Pts',(3.68850172300477,-1.,-0.676569286094607));
#39659=CARTESIAN_POINT('Ctrl Pts',(3.68845817949586,-1.,-0.676591647975429));
#39660=CARTESIAN_POINT('',(3.71701050416802,-1.,-0.496319364829374));
#39661=CARTESIAN_POINT('Origin',(0.,-1.,0.));
#39662=CARTESIAN_POINT('',(4.18039834341342,-1.,-0.40530197431835));
#39663=CARTESIAN_POINT('Ctrl Pts',(3.71701050416802,-1.,-0.496319364829374));
#39664=CARTESIAN_POINT('Ctrl Pts',(3.71704500630521,-1.,-0.496354087925646));
#39665=CARTESIAN_POINT('Ctrl Pts',(3.71721917030465,-1.,-0.496446644158827));
#39666=CARTESIAN_POINT('Ctrl Pts',(3.71785517607694,-1.,-0.496605651526314));
#39667=CARTESIAN_POINT('Ctrl Pts',(3.7195232082259,-1.,-0.496846224822535));
#39668=CARTESIAN_POINT('Ctrl Pts',(3.72301489774241,-1.,-0.497187079575795));
#39669=CARTESIAN_POINT('Ctrl Pts',(3.72830430904794,-1.,-0.49758406715328));
#39670=CARTESIAN_POINT('Ctrl Pts',(3.73486914372834,-1.,-0.497984209510496));
#39671=CARTESIAN_POINT('Ctrl Pts',(3.74235701735109,-1.,-0.498350586058176));
#39672=CARTESIAN_POINT('Ctrl Pts',(3.75037362168103,-1.,-0.498642802042929));
#39673=CARTESIAN_POINT('Ctrl Pts',(3.75854082221127,-1.,-0.498823681615513));
#39674=CARTESIAN_POINT('Ctrl Pts',(3.76655401191144,-1.,-0.498865792335185));
#39675=CARTESIAN_POINT('Ctrl Pts',(3.77425499225089,-1.,-0.498759900365687));
#39676=CARTESIAN_POINT('Ctrl Pts',(3.78163975337189,-1.,-0.498515471679379));
#39677=CARTESIAN_POINT('Ctrl Pts',(3.78879701661152,-1.,-0.498152751800819));
#39678=CARTESIAN_POINT('Ctrl Pts',(3.79586380669959,-1.,-0.497696892100581));
#39679=CARTESIAN_POINT('Ctrl Pts',(3.80297788298545,-1.,-0.497171756201091));
#39680=CARTESIAN_POINT('Ctrl Pts',(3.81022254090909,-1.,-0.496592643443789));
#39681=CARTESIAN_POINT('Ctrl Pts',(3.81760756144099,-1.,-0.495963937875572));
#39682=CARTESIAN_POINT('Ctrl Pts',(3.82509963594156,-1.,-0.495283458893903));
#39683=CARTESIAN_POINT('Ctrl Pts',(3.8326409268245,-1.,-0.494545212256426));
#39684=CARTESIAN_POINT('Ctrl Pts',(3.84017095578438,-1.,-0.493742574629117));
#39685=CARTESIAN_POINT('Ctrl Pts',(3.84765051147965,-1.,-0.492871792414095));
#39686=CARTESIAN_POINT('Ctrl Pts',(3.85507287020223,-1.,-0.49193363108376));
#39687=CARTESIAN_POINT('Ctrl Pts',(3.86245057319215,-1.,-0.490931482170849));
#39688=CARTESIAN_POINT('Ctrl Pts',(3.86980755613694,-1.,-0.4898702457049));
#39689=CARTESIAN_POINT('Ctrl Pts',(3.87716963231115,-1.,-0.488754973798281));
#39690=CARTESIAN_POINT('Ctrl Pts',(3.88455453328156,-1.,-0.487589452275179));
#39691=CARTESIAN_POINT('Ctrl Pts',(3.89196582437574,-1.,-0.486375337854134));
#39692=CARTESIAN_POINT('Ctrl Pts',(3.89939844658529,-1.,-0.485112963522246));
#39693=CARTESIAN_POINT('Ctrl Pts',(3.90684210358063,-1.,-0.483801835089161));
#39694=CARTESIAN_POINT('Ctrl Pts',(3.91428536373749,-1.,-0.482441230340709));
#39695=CARTESIAN_POINT('Ctrl Pts',(3.92171976072334,-1.,-0.481030798910735));
#39696=CARTESIAN_POINT('Ctrl Pts',(3.92914297392067,-1.,-0.479571028525566));
#39697=CARTESIAN_POINT('Ctrl Pts',(3.93655660689819,-1.,-0.478062927140957));
#39698=CARTESIAN_POINT('Ctrl Pts',(3.94396469119385,-1.,-0.476507810658535));
#39699=CARTESIAN_POINT('Ctrl Pts',(3.95137192932898,-1.,-0.474907053021791));
#39700=CARTESIAN_POINT('Ctrl Pts',(3.95878201038332,-1.,-0.473261847236296));
#39701=CARTESIAN_POINT('Ctrl Pts',(3.96619600864626,-1.,-0.471572978413494));
#39702=CARTESIAN_POINT('Ctrl Pts',(3.97361320212413,-1.,-0.469840942829878));
#39703=CARTESIAN_POINT('Ctrl Pts',(3.98103175589349,-1.,-0.46806604792014));
#39704=CARTESIAN_POINT('Ctrl Pts',(3.98844946363258,-1.,-0.466248520883035));
#39705=CARTESIAN_POINT('Ctrl Pts',(3.99586444320134,-1.,-0.464388610938995));
#39706=CARTESIAN_POINT('Ctrl Pts',(4.00327590659129,-1.,-0.462486702616252));
#39707=CARTESIAN_POINT('Ctrl Pts',(4.01068390573469,-1.,-0.460543280768577));
#39708=CARTESIAN_POINT('Ctrl Pts',(4.01808900827647,-1.,-0.458558885637001));
#39709=CARTESIAN_POINT('Ctrl Pts',(4.02549199038414,-1.,-0.456534070784968));
#39710=CARTESIAN_POINT('Ctrl Pts',(4.03289354362745,-1.,-0.454469363020496));
#39711=CARTESIAN_POINT('Ctrl Pts',(4.0402939222793,-1.,-0.452365214748779));
#39712=CARTESIAN_POINT('Ctrl Pts',(4.0476929901797,-1.,-0.450222009543774));
#39713=CARTESIAN_POINT('Ctrl Pts',(4.05509037796815,-1.,-0.448040082683977));
#39714=CARTESIAN_POINT('Ctrl Pts',(4.06248560760596,-1.,-0.445819737468478));
#39715=CARTESIAN_POINT('Ctrl Pts',(4.0698782192577,-1.,-0.443561262395408));
#39716=CARTESIAN_POINT('Ctrl Pts',(4.07726792490256,-1.,-0.441264951396587));
#39717=CARTESIAN_POINT('Ctrl Pts',(4.08465462294625,-1.,-0.438931108931614));
#39718=CARTESIAN_POINT('Ctrl Pts',(4.09203832139439,-1.,-0.436560044913814));
#39719=CARTESIAN_POINT('Ctrl Pts',(4.09941908688567,-1.,-0.434152073200643));
#39720=CARTESIAN_POINT('Ctrl Pts',(4.10679698750219,-1.,-0.431707508679772));
#39721=CARTESIAN_POINT('Ctrl Pts',(4.1141720278277,-1.,-0.429226666075373));
#39722=CARTESIAN_POINT('Ctrl Pts',(4.1215441250121,-1.,-0.426709855706243));
#39723=CARTESIAN_POINT('Ctrl Pts',(4.1289131463371,-1.,-0.424157375323155));
#39724=CARTESIAN_POINT('Ctrl Pts',(4.13627893206433,-1.,-0.421569503103971));
#39725=CARTESIAN_POINT('Ctrl Pts',(4.14364132317223,-1.,-0.4189464906678));
#39726=CARTESIAN_POINT('Ctrl Pts',(4.15100018950989,-1.,-0.416288556008986));
#39727=CARTESIAN_POINT('Ctrl Pts',(4.1583554501909,-1.,-0.413595877953269));
#39728=CARTESIAN_POINT('Ctrl Pts',(4.16570705940731,-1.,-0.410868596148614));
#39729=CARTESIAN_POINT('Ctrl Pts',(4.17158541009947,-1.,-0.408659167570153));
#39730=CARTESIAN_POINT('Ctrl Pts',(4.17599251955585,-1.,-0.406986596326603));
#39731=CARTESIAN_POINT('Ctrl Pts',(4.17892985789908,-1.,-0.405864662679631));
#39732=CARTESIAN_POINT('Ctrl Pts',(4.18039834341342,-1.,-0.40530197431835));
#39733=CARTESIAN_POINT('',(4.1923339003649,-1.,-0.253646344052521));
#39734=CARTESIAN_POINT('',(4.18039834341342,-1.,-0.40530197431835));
#39735=CARTESIAN_POINT('',(3.74888939116255,-1.,-0.0912596999166826));
#39736=CARTESIAN_POINT('Ctrl Pts',(4.1923339003649,-1.,-0.253646344052521));
#39737=CARTESIAN_POINT('Ctrl Pts',(4.19097151819241,-1.,-0.252860861572566));
#39738=CARTESIAN_POINT('Ctrl Pts',(4.18824585244066,-1.,-0.251293239837693));
#39739=CARTESIAN_POINT('Ctrl Pts',(4.18415464959491,-1.,-0.248951836910964));
#39740=CARTESIAN_POINT('Ctrl Pts',(4.17869430192868,-1.,-0.245850033418584));
#39741=CARTESIAN_POINT('Ctrl Pts',(4.17185984409533,-1.,-0.242006283923912));
#39742=CARTESIAN_POINT('Ctrl Pts',(4.1650163665385,-1.,-0.238196140933977));
#39743=CARTESIAN_POINT('Ctrl Pts',(4.1581638926525,-1.,-0.234419749543143));
#39744=CARTESIAN_POINT('Ctrl Pts',(4.15130247435029,-1.,-0.230677299028738));
#39745=CARTESIAN_POINT('Ctrl Pts',(4.14443220607733,-1.,-0.226969025061244));
#39746=CARTESIAN_POINT('Ctrl Pts',(4.13755320553563,-1.,-0.223295201038384));
#39747=CARTESIAN_POINT('Ctrl Pts',(4.13066558698156,-1.,-0.219656126701852));
#39748=CARTESIAN_POINT('Ctrl Pts',(4.12376943492249,-1.,-0.216052116898425));
#39749=CARTESIAN_POINT('Ctrl Pts',(4.11686478264545,-1.,-0.212483491087068));
#39750=CARTESIAN_POINT('Ctrl Pts',(4.10995157639026,-1.,-0.208950559400172));
#39751=CARTESIAN_POINT('Ctrl Pts',(4.10302969965374,-1.,-0.205453622198233));
#39752=CARTESIAN_POINT('Ctrl Pts',(4.09609903751912,-1.,-0.201992979049985));
#39753=CARTESIAN_POINT('Ctrl Pts',(4.08915953359753,-1.,-0.198568934800811));
#39754=CARTESIAN_POINT('Ctrl Pts',(4.08221124060385,-1.,-0.195181806054714));
#39755=CARTESIAN_POINT('Ctrl Pts',(4.07525439703137,-1.,-0.191831928181081));
#39756=CARTESIAN_POINT('Ctrl Pts',(4.06828941192308,-1.,-0.188519658060256));
#39757=CARTESIAN_POINT('Ctrl Pts',(4.06131670998589,-1.,-0.185245370038948));
#39758=CARTESIAN_POINT('Ctrl Pts',(4.05433660358402,-1.,-0.18200945304855));
#39759=CARTESIAN_POINT('Ctrl Pts',(4.04734916719722,-1.,-0.178812307240716));
#39760=CARTESIAN_POINT('Ctrl Pts',(4.04035407891161,-1.,-0.175654339673758));
#39761=CARTESIAN_POINT('Ctrl Pts',(4.03335057326093,-1.,-0.172535962484467));
#39762=CARTESIAN_POINT('Ctrl Pts',(4.0263377970371,-1.,-0.169457601001653));
#39763=CARTESIAN_POINT('Ctrl Pts',(4.01931510507143,-1.,-0.166419700015848));
#39764=CARTESIAN_POINT('Ctrl Pts',(4.01228237022301,-1.,-0.163422730287459));
#39765=CARTESIAN_POINT('Ctrl Pts',(4.00524031064509,-1.,-0.160467194882219));
#39766=CARTESIAN_POINT('Ctrl Pts',(3.99819074631874,-1.,-0.15755363438381));
#39767=CARTESIAN_POINT('Ctrl Pts',(3.99113582086059,-1.,-0.154682618338563));
#39768=CARTESIAN_POINT('Ctrl Pts',(3.9840772985098,-1.,-0.151854737441406));
#39769=CARTESIAN_POINT('Ctrl Pts',(3.97701581473643,-1.,-0.149070594803544));
#39770=CARTESIAN_POINT('Ctrl Pts',(3.96995018565891,-1.,-0.146330797814514));
#39771=CARTESIAN_POINT('Ctrl Pts',(3.96287658098896,-1.,-0.143635947692791));
#39772=CARTESIAN_POINT('Ctrl Pts',(3.95579014116899,-1.,-0.140986665829937));
#39773=CARTESIAN_POINT('Ctrl Pts',(3.94868667844355,-1.,-0.138383621255159));
#39774=CARTESIAN_POINT('Ctrl Pts',(3.94156445130744,-1.,-0.135827558661188));
#39775=CARTESIAN_POINT('Ctrl Pts',(3.93442567551035,-1.,-0.13331932279419));
#39776=CARTESIAN_POINT('Ctrl Pts',(3.9272787679596,-1.,-0.130859892027799));
#39777=CARTESIAN_POINT('Ctrl Pts',(3.92013513251642,-1.,-0.128450341339528));
#39778=CARTESIAN_POINT('Ctrl Pts',(3.91300501605392,-1.,-0.126091793324137));
#39779=CARTESIAN_POINT('Ctrl Pts',(3.90589336320508,-1.,-0.123785368272378));
#39780=CARTESIAN_POINT('Ctrl Pts',(3.89879639336952,-1.,-0.121532144765723));
#39781=CARTESIAN_POINT('Ctrl Pts',(3.89169600105201,-1.,-0.119333088190418));
#39782=CARTESIAN_POINT('Ctrl Pts',(3.88456590045767,-1.,-0.117189150373144));
#39783=CARTESIAN_POINT('Ctrl Pts',(3.87738168405343,-1.,-0.11510142664947));
#39784=CARTESIAN_POINT('Ctrl Pts',(3.87013043445014,-1.,-0.113071304914562));
#39785=CARTESIAN_POINT('Ctrl Pts',(3.86281867282965,-1.,-0.111100593036261));
#39786=CARTESIAN_POINT('Ctrl Pts',(3.855485714969,-1.,-0.109191717634944));
#39787=CARTESIAN_POINT('Ctrl Pts',(3.84819233070317,-1.,-0.107347597812184));
#39788=CARTESIAN_POINT('Ctrl Pts',(3.84099658324803,-1.,-0.105571360916569));
#39789=CARTESIAN_POINT('Ctrl Pts',(3.83393171228002,-1.,-0.103866063811623));
#39790=CARTESIAN_POINT('Ctrl Pts',(3.82698737143255,-1.,-0.102234506488457));
#39791=CARTESIAN_POINT('Ctrl Pts',(3.82007889742625,-1.,-0.100678769650632));
#39792=CARTESIAN_POINT('Ctrl Pts',(3.81306649386461,-1.,-0.0992008728096518));
#39793=CARTESIAN_POINT('Ctrl Pts',(3.80581088847809,-1.,-0.0978042222906647));
#39794=CARTESIAN_POINT('Ctrl Pts',(3.79822128513845,-1.,-0.0964949352873135));
#39795=CARTESIAN_POINT('Ctrl Pts',(3.79030016353111,-1.,-0.0952829885100805));
#39796=CARTESIAN_POINT('Ctrl Pts',(3.782205218991,-1.,-0.0941840095090818));
#39797=CARTESIAN_POINT('Ctrl Pts',(3.77424159971059,-1.,-0.0932185546203182));
#39798=CARTESIAN_POINT('Ctrl Pts',(3.76678860031841,-1.,-0.0924090589602695));
#39799=CARTESIAN_POINT('Ctrl Pts',(3.76024199359303,-1.,-0.0917773084998339));
#39800=CARTESIAN_POINT('Ctrl Pts',(3.75495560118212,-1.,-0.0913419622736402));
#39801=CARTESIAN_POINT('Ctrl Pts',(3.75145357872422,-1.,-0.091132399957443));
#39802=CARTESIAN_POINT('Ctrl Pts',(3.74976844886346,-1.,-0.0911090736805514));
#39803=CARTESIAN_POINT('Ctrl Pts',(3.74911539914542,-1.,-0.0911666301812821));
#39804=CARTESIAN_POINT('Ctrl Pts',(3.74892890040974,-1.,-0.0912308016421984));
#39805=CARTESIAN_POINT('Ctrl Pts',(3.74888939116255,-1.,-0.0912596999166826));
#39806=CARTESIAN_POINT('',(3.74888939116259,-1.,0.0912596999148864));
#39807=CARTESIAN_POINT('Origin',(0.,-1.,0.));
#39808=CARTESIAN_POINT('',(4.1923339003649,-1.,0.253646344052522));
#39809=CARTESIAN_POINT('Ctrl Pts',(3.74888939116259,-1.,0.0912596999148864));
#39810=CARTESIAN_POINT('Ctrl Pts',(3.74892890041021,-1.,0.0912308016409238));
#39811=CARTESIAN_POINT('Ctrl Pts',(3.74911539914664,-1.,0.091166630180643));
#39812=CARTESIAN_POINT('Ctrl Pts',(3.74976844886495,-1.,0.0911090736804577));
#39813=CARTESIAN_POINT('Ctrl Pts',(3.75145357872511,-1.,0.0911323999576149));
#39814=CARTESIAN_POINT('Ctrl Pts',(3.75495560118053,-1.,0.0913419622735858));
#39815=CARTESIAN_POINT('Ctrl Pts',(3.76024199359493,-1.,0.0917773084999013));
#39816=CARTESIAN_POINT('Ctrl Pts',(3.76678860032228,-1.,0.092409058960406));
#39817=CARTESIAN_POINT('Ctrl Pts',(3.77424159971456,-1.,0.093218554620458));
#39818=CARTESIAN_POINT('Ctrl Pts',(3.78220521899366,-1.,0.0941840095091749));
#39819=CARTESIAN_POINT('Ctrl Pts',(3.79030016353186,-1.,0.0952829885101074));
#39820=CARTESIAN_POINT('Ctrl Pts',(3.7982212851376,-1.,0.0964949352872849));
#39821=CARTESIAN_POINT('Ctrl Pts',(3.80581088847642,-1.,0.097804222290608));
#39822=CARTESIAN_POINT('Ctrl Pts',(3.81306649386293,-1.,0.0992008728095949));
#39823=CARTESIAN_POINT('Ctrl Pts',(3.82007889742512,-1.,0.100678769650595));
#39824=CARTESIAN_POINT('Ctrl Pts',(3.8269873714322,-1.,0.102234506488446));
#39825=CARTESIAN_POINT('Ctrl Pts',(3.83393171228034,-1.,0.103866063811635));
#39826=CARTESIAN_POINT('Ctrl Pts',(3.84099658324873,-1.,0.105571360916594));
#39827=CARTESIAN_POINT('Ctrl Pts',(3.84819233070391,-1.,0.107347597812209));
#39828=CARTESIAN_POINT('Ctrl Pts',(3.85548571496953,-1.,0.109191717634961));
#39829=CARTESIAN_POINT('Ctrl Pts',(3.86281867282984,-1.,0.111100593036267));
#39830=CARTESIAN_POINT('Ctrl Pts',(3.87013043445001,-1.,0.113071304914559));
#39831=CARTESIAN_POINT('Ctrl Pts',(3.87738168405308,-1.,0.115101426649461));
#39832=CARTESIAN_POINT('Ctrl Pts',(3.88456590045726,-1.,0.117189150373135));
#39833=CARTESIAN_POINT('Ctrl Pts',(3.8916960010517,-1.,0.119333088190411));
#39834=CARTESIAN_POINT('Ctrl Pts',(3.89879639336939,-1.,0.121532144765722));
#39835=CARTESIAN_POINT('Ctrl Pts',(3.90589336320515,-1.,0.12378536827238));
#39836=CARTESIAN_POINT('Ctrl Pts',(3.91300501605411,-1.,0.126091793324141));
#39837=CARTESIAN_POINT('Ctrl Pts',(3.92013513251664,-1.,0.128450341339533));
#39838=CARTESIAN_POINT('Ctrl Pts',(3.92727876795977,-1.,0.130859892027802));
#39839=CARTESIAN_POINT('Ctrl Pts',(3.93442567551042,-1.,0.133319322794191));
#39840=CARTESIAN_POINT('Ctrl Pts',(3.94156445130741,-1.,0.135827558661189));
#39841=CARTESIAN_POINT('Ctrl Pts',(3.94868667844347,-1.,0.138383621255161));
#39842=CARTESIAN_POINT('Ctrl Pts',(3.95579014116894,-1.,0.140986665829942));
#39843=CARTESIAN_POINT('Ctrl Pts',(3.96287658098896,-1.,0.143635947692799));
#39844=CARTESIAN_POINT('Ctrl Pts',(3.96995018565893,-1.,0.146330797814521));
#39845=CARTESIAN_POINT('Ctrl Pts',(3.97701581473644,-1.,0.149070594803545));
#39846=CARTESIAN_POINT('Ctrl Pts',(3.98407729850975,-1.,0.151854737441399));
#39847=CARTESIAN_POINT('Ctrl Pts',(3.99113582086043,-1.,0.154682618338548));
#39848=CARTESIAN_POINT('Ctrl Pts',(3.9981907463185,-1.,0.15755363438379));
#39849=CARTESIAN_POINT('Ctrl Pts',(4.00524031064487,-1.,0.160467194882203));
#39850=CARTESIAN_POINT('Ctrl Pts',(4.01228237022296,-1.,0.163422730287457));
#39851=CARTESIAN_POINT('Ctrl Pts',(4.01931510507167,-1.,0.166419700015866));
#39852=CARTESIAN_POINT('Ctrl Pts',(4.02633779703764,-1.,0.169457601001692));
#39853=CARTESIAN_POINT('Ctrl Pts',(4.03335057326163,-1.,0.172535962484515));
#39854=CARTESIAN_POINT('Ctrl Pts',(4.04035407891222,-1.,0.175654339673798));
#39855=CARTESIAN_POINT('Ctrl Pts',(4.04734916719741,-1.,0.178812307240729));
#39856=CARTESIAN_POINT('Ctrl Pts',(4.05433660358353,-1.,0.18200945304852));
#39857=CARTESIAN_POINT('Ctrl Pts',(4.06131670998469,-1.,0.185245370038874));
#39858=CARTESIAN_POINT('Ctrl Pts',(4.06828941192148,-1.,0.188519658060156));
#39859=CARTESIAN_POINT('Ctrl Pts',(4.07525439702992,-1.,0.191831928180991));
#39860=CARTESIAN_POINT('Ctrl Pts',(4.08221124060322,-1.,0.195181806054676));
#39861=CARTESIAN_POINT('Ctrl Pts',(4.08915953359833,-1.,0.198568934800862));
#39862=CARTESIAN_POINT('Ctrl Pts',(4.09609903752152,-1.,0.201992979050136));
#39863=CARTESIAN_POINT('Ctrl Pts',(4.10302969965728,-1.,0.205453622198455));
#39864=CARTESIAN_POINT('Ctrl Pts',(4.10995157639377,-1.,0.208950559400393));
#39865=CARTESIAN_POINT('Ctrl Pts',(4.11686478264739,-1.,0.21248349108719));
#39866=CARTESIAN_POINT('Ctrl Pts',(4.12376943492132,-1.,0.216052116898353));
#39867=CARTESIAN_POINT('Ctrl Pts',(4.13066558697658,-1.,0.219656126701542));
#39868=CARTESIAN_POINT('Ctrl Pts',(4.13755320552764,-1.,0.223295201037886));
#39869=CARTESIAN_POINT('Ctrl Pts',(4.14443220606869,-1.,0.226969025060706));
#39870=CARTESIAN_POINT('Ctrl Pts',(4.15130247434459,-1.,0.230677299028384));
#39871=CARTESIAN_POINT('Ctrl Pts',(4.15816389265352,-1.,0.234419749543208));
#39872=CARTESIAN_POINT('Ctrl Pts',(4.16501636654877,-1.,0.238196140934617));
#39873=CARTESIAN_POINT('Ctrl Pts',(4.17185984411426,-1.,0.242006283925089));
#39874=CARTESIAN_POINT('Ctrl Pts',(4.1786943019518,-1.,0.24585003342002));
#39875=CARTESIAN_POINT('Ctrl Pts',(4.18415464961466,-1.,0.248951836912189));
#39876=CARTESIAN_POINT('Ctrl Pts',(4.18824585245272,-1.,0.251293239838441));
#39877=CARTESIAN_POINT('Ctrl Pts',(4.19097151819684,-1.,0.252860861572841));
#39878=CARTESIAN_POINT('Ctrl Pts',(4.1923339003649,-1.,0.253646344052522));
#39879=CARTESIAN_POINT('',(4.18039834341342,-1.,0.405301974318351));
#39880=CARTESIAN_POINT('',(4.1923339003649,-1.,0.253646344052522));
#39881=CARTESIAN_POINT('Ctrl Pts',(4.18039834341342,-1.,0.405301974318351));
#39882=CARTESIAN_POINT('Ctrl Pts',(4.17892985789466,-1.,0.40586466267921));
#39883=CARTESIAN_POINT('Ctrl Pts',(4.17599251954382,-1.,0.406986596325455));
#39884=CARTESIAN_POINT('Ctrl Pts',(4.17158541007977,-1.,0.408659167568273));
#39885=CARTESIAN_POINT('Ctrl Pts',(4.16570705938425,-1.,0.410868596146415));
#39886=CARTESIAN_POINT('Ctrl Pts',(4.15835545017202,-1.,0.413595877951471));
#39887=CARTESIAN_POINT('Ctrl Pts',(4.15100018949965,-1.,0.416288556008012));
#39888=CARTESIAN_POINT('Ctrl Pts',(4.14364132317121,-1.,0.418946490667703));
#39889=CARTESIAN_POINT('Ctrl Pts',(4.13627893207002,-1.,0.421569503104513));
#39890=CARTESIAN_POINT('Ctrl Pts',(4.12891314634572,-1.,0.424157375323976));
#39891=CARTESIAN_POINT('Ctrl Pts',(4.12154412502007,-1.,0.426709855707001));
#39892=CARTESIAN_POINT('Ctrl Pts',(4.11417202783267,-1.,0.429226666075845));
#39893=CARTESIAN_POINT('Ctrl Pts',(4.10679698750336,-1.,0.431707508679884));
#39894=CARTESIAN_POINT('Ctrl Pts',(4.09941908688373,-1.,0.434152073200461));
#39895=CARTESIAN_POINT('Ctrl Pts',(4.09203832139089,-1.,0.436560044913483));
#39896=CARTESIAN_POINT('Ctrl Pts',(4.08465462294273,-1.,0.43893110893128));
#39897=CARTESIAN_POINT('Ctrl Pts',(4.07726792490016,-1.,0.441264951396361));
#39898=CARTESIAN_POINT('Ctrl Pts',(4.0698782192569,-1.,0.443561262395333));
#39899=CARTESIAN_POINT('Ctrl Pts',(4.06248560760659,-1.,0.445819737468538));
#39900=CARTESIAN_POINT('Ctrl Pts',(4.0550903779696,-1.,0.448040082684115));
#39901=CARTESIAN_POINT('Ctrl Pts',(4.0476929901813,-1.,0.450222009543927));
#39902=CARTESIAN_POINT('Ctrl Pts',(4.04029392228049,-1.,0.452365214748893));
#39903=CARTESIAN_POINT('Ctrl Pts',(4.03289354362794,-1.,0.454469363020542));
#39904=CARTESIAN_POINT('Ctrl Pts',(4.02549199038394,-1.,0.456534070784951));
#39905=CARTESIAN_POINT('Ctrl Pts',(4.01808900827587,-1.,0.458558885636946));
#39906=CARTESIAN_POINT('Ctrl Pts',(4.01068390573399,-1.,0.460543280768515));
#39907=CARTESIAN_POINT('Ctrl Pts',(4.00327590659075,-1.,0.462486702616205));
#39908=CARTESIAN_POINT('Ctrl Pts',(3.9958644432011,-1.,0.464388610938976));
#39909=CARTESIAN_POINT('Ctrl Pts',(3.98844946363262,-1.,0.46624852088304));
#39910=CARTESIAN_POINT('Ctrl Pts',(3.98103175589371,-1.,0.468066047920158));
#39911=CARTESIAN_POINT('Ctrl Pts',(3.97361320212436,-1.,0.469840942829896));
#39912=CARTESIAN_POINT('Ctrl Pts',(3.96619600864643,-1.,0.471572978413504));
#39913=CARTESIAN_POINT('Ctrl Pts',(3.95878201038338,-1.,0.473261847236298));
#39914=CARTESIAN_POINT('Ctrl Pts',(3.95137192932897,-1.,0.474907053021791));
#39915=CARTESIAN_POINT('Ctrl Pts',(3.94396469119383,-1.,0.476507810658538));
#39916=CARTESIAN_POINT('Ctrl Pts',(3.93655660689819,-1.,0.478062927140965));
#39917=CARTESIAN_POINT('Ctrl Pts',(3.92914297392071,-1.,0.479571028525579));
#39918=CARTESIAN_POINT('Ctrl Pts',(3.92171976072341,-1.,0.481030798910749));
#39919=CARTESIAN_POINT('Ctrl Pts',(3.91428536373751,-1.,0.482441230340714));
#39920=CARTESIAN_POINT('Ctrl Pts',(3.90684210358056,-1.,0.48380183508915));
#39921=CARTESIAN_POINT('Ctrl Pts',(3.89939844658513,-1.,0.485112963522223));
#39922=CARTESIAN_POINT('Ctrl Pts',(3.89196582437552,-1.,0.486375337854104));
#39923=CARTESIAN_POINT('Ctrl Pts',(3.88455453328138,-1.,0.487589452275155));
#39924=CARTESIAN_POINT('Ctrl Pts',(3.87716963231109,-1.,0.488754973798274));
#39925=CARTESIAN_POINT('Ctrl Pts',(3.86980755613707,-1.,0.489870245704918));
#39926=CARTESIAN_POINT('Ctrl Pts',(3.86245057319246,-1.,0.490931482170891));
#39927=CARTESIAN_POINT('Ctrl Pts',(3.85507287020263,-1.,0.491933631083814));
#39928=CARTESIAN_POINT('Ctrl Pts',(3.84765051147999,-1.,0.492871792414141));
#39929=CARTESIAN_POINT('Ctrl Pts',(3.84017095578451,-1.,0.493742574629135));
#39930=CARTESIAN_POINT('Ctrl Pts',(3.83264092682431,-1.,0.494545212256402));
#39931=CARTESIAN_POINT('Ctrl Pts',(3.82509963594103,-1.,0.495283458893838));
#39932=CARTESIAN_POINT('Ctrl Pts',(3.81760756144025,-1.,0.49596393787548));
#39933=CARTESIAN_POINT('Ctrl Pts',(3.81022254090839,-1.,0.496592643443704));
#39934=CARTESIAN_POINT('Ctrl Pts',(3.80297788298514,-1.,0.497171756201052));
#39935=CARTESIAN_POINT('Ctrl Pts',(3.79586380669994,-1.,0.497696892100625));
#39936=CARTESIAN_POINT('Ctrl Pts',(3.78879701661264,-1.,0.498152751800959));
#39937=CARTESIAN_POINT('Ctrl Pts',(3.78163975337356,-1.,0.498515471679585));
#39938=CARTESIAN_POINT('Ctrl Pts',(3.77425499225255,-1.,0.498759900365892));
#39939=CARTESIAN_POINT('Ctrl Pts',(3.76655401191229,-1.,0.498865792335291));
#39940=CARTESIAN_POINT('Ctrl Pts',(3.75854082221053,-1.,0.498823681615422));
#39941=CARTESIAN_POINT('Ctrl Pts',(3.75037362167839,-1.,0.498642802042606));
#39942=CARTESIAN_POINT('Ctrl Pts',(3.74235701734714,-1.,0.498350586057693));
#39943=CARTESIAN_POINT('Ctrl Pts',(3.73486914372449,-1.,0.497984209510025));
#39944=CARTESIAN_POINT('Ctrl Pts',(3.72830430904606,-1.,0.49758406715305));
#39945=CARTESIAN_POINT('Ctrl Pts',(3.72301489774398,-1.,0.497187079575988));
#39946=CARTESIAN_POINT('Ctrl Pts',(3.71952320822499,-1.,0.496846224822564));
#39947=CARTESIAN_POINT('Ctrl Pts',(3.71785517607549,-1.,0.496605651525989));
#39948=CARTESIAN_POINT('Ctrl Pts',(3.71721917030355,-1.,0.496446644158006));
#39949=CARTESIAN_POINT('Ctrl Pts',(3.71704500630494,-1.,0.496354087924313));
#39950=CARTESIAN_POINT('Ctrl Pts',(3.71701050416825,-1.,0.496319364827592));
#39951=CARTESIAN_POINT('Origin',(0.,-1.,0.));
#39952=CARTESIAN_POINT('Origin',(0.,0.,0.));
#39953=CARTESIAN_POINT('Origin',(0.,2.2,0.));
#39954=CARTESIAN_POINT('Origin',(0.,1.,0.));
#39955=CARTESIAN_POINT('',(-1.99383466746626,2.2,0.15691819145569));
#39956=CARTESIAN_POINT('Origin',(0.,2.2,0.));
#39957=CARTESIAN_POINT('',(-1.99383466746626,1.,0.15691819145569));
#39958=CARTESIAN_POINT('',(-1.99383466746626,1.,0.15691819145569));
#39959=CARTESIAN_POINT('Origin',(0.,1.,0.));
#39960=CARTESIAN_POINT('Origin',(0.,2.2,0.));
#39961=CARTESIAN_POINT('Ctrl Pts',(4.1923339003649,-1.,0.253646344052522));
#39962=CARTESIAN_POINT('Ctrl Pts',(4.1923339003649,1.,0.253646344052522));
#39963=CARTESIAN_POINT('Ctrl Pts',(4.19097151819684,-1.,0.252860861572841));
#39964=CARTESIAN_POINT('Ctrl Pts',(4.19097151819684,1.,0.252860861572841));
#39965=CARTESIAN_POINT('Ctrl Pts',(4.18824585245272,-1.,0.251293239838441));
#39966=CARTESIAN_POINT('Ctrl Pts',(4.18824585245272,1.,0.251293239838441));
#39967=CARTESIAN_POINT('Ctrl Pts',(4.18415464961466,-1.,0.248951836912189));
#39968=CARTESIAN_POINT('Ctrl Pts',(4.18415464961466,1.,0.248951836912189));
#39969=CARTESIAN_POINT('Ctrl Pts',(4.1786943019518,-1.,0.24585003342002));
#39970=CARTESIAN_POINT('Ctrl Pts',(4.1786943019518,1.,0.24585003342002));
#39971=CARTESIAN_POINT('Ctrl Pts',(4.17185984411426,-1.,0.242006283925089));
#39972=CARTESIAN_POINT('Ctrl Pts',(4.17185984411426,1.,0.242006283925089));
#39973=CARTESIAN_POINT('Ctrl Pts',(4.16501636654877,-1.,0.238196140934617));
#39974=CARTESIAN_POINT('Ctrl Pts',(4.16501636654877,1.,0.238196140934617));
#39975=CARTESIAN_POINT('Ctrl Pts',(4.15816389265352,-1.,0.234419749543208));
#39976=CARTESIAN_POINT('Ctrl Pts',(4.15816389265352,1.,0.234419749543208));
#39977=CARTESIAN_POINT('Ctrl Pts',(4.15130247434459,-1.,0.230677299028384));
#39978=CARTESIAN_POINT('Ctrl Pts',(4.15130247434459,1.,0.230677299028384));
#39979=CARTESIAN_POINT('Ctrl Pts',(4.14443220606869,-1.,0.226969025060706));
#39980=CARTESIAN_POINT('Ctrl Pts',(4.14443220606869,1.,0.226969025060706));
#39981=CARTESIAN_POINT('Ctrl Pts',(4.13755320552764,-1.,0.223295201037886));
#39982=CARTESIAN_POINT('Ctrl Pts',(4.13755320552764,1.,0.223295201037886));
#39983=CARTESIAN_POINT('Ctrl Pts',(4.13066558697658,-1.,0.219656126701542));
#39984=CARTESIAN_POINT('Ctrl Pts',(4.13066558697658,1.,0.219656126701542));
#39985=CARTESIAN_POINT('Ctrl Pts',(4.12376943492132,-1.,0.216052116898353));
#39986=CARTESIAN_POINT('Ctrl Pts',(4.12376943492132,1.,0.216052116898353));
#39987=CARTESIAN_POINT('Ctrl Pts',(4.11686478264739,-1.,0.21248349108719));
#39988=CARTESIAN_POINT('Ctrl Pts',(4.11686478264739,1.,0.21248349108719));
#39989=CARTESIAN_POINT('Ctrl Pts',(4.10995157639377,-1.,0.208950559400393));
#39990=CARTESIAN_POINT('Ctrl Pts',(4.10995157639377,1.,0.208950559400393));
#39991=CARTESIAN_POINT('Ctrl Pts',(4.10302969965728,-1.,0.205453622198455));
#39992=CARTESIAN_POINT('Ctrl Pts',(4.10302969965728,1.,0.205453622198455));
#39993=CARTESIAN_POINT('Ctrl Pts',(4.09609903752152,-1.,0.201992979050136));
#39994=CARTESIAN_POINT('Ctrl Pts',(4.09609903752152,1.,0.201992979050136));
#39995=CARTESIAN_POINT('Ctrl Pts',(4.08915953359833,-1.,0.198568934800862));
#39996=CARTESIAN_POINT('Ctrl Pts',(4.08915953359833,1.,0.198568934800862));
#39997=CARTESIAN_POINT('Ctrl Pts',(4.08221124060322,-1.,0.195181806054676));
#39998=CARTESIAN_POINT('Ctrl Pts',(4.08221124060322,1.,0.195181806054676));
#39999=CARTESIAN_POINT('Ctrl Pts',(4.07525439702992,-1.,0.191831928180991));
#40000=CARTESIAN_POINT('Ctrl Pts',(4.07525439702992,1.,0.191831928180991));
#40001=CARTESIAN_POINT('Ctrl Pts',(4.06828941192148,-1.,0.188519658060156));
#40002=CARTESIAN_POINT('Ctrl Pts',(4.06828941192148,1.,0.188519658060156));
#40003=CARTESIAN_POINT('Ctrl Pts',(4.06131670998469,-1.,0.185245370038874));
#40004=CARTESIAN_POINT('Ctrl Pts',(4.06131670998469,1.,0.185245370038874));
#40005=CARTESIAN_POINT('Ctrl Pts',(4.05433660358353,-1.,0.18200945304852));
#40006=CARTESIAN_POINT('Ctrl Pts',(4.05433660358353,1.,0.18200945304852));
#40007=CARTESIAN_POINT('Ctrl Pts',(4.04734916719741,-1.,0.178812307240729));
#40008=CARTESIAN_POINT('Ctrl Pts',(4.04734916719741,1.,0.178812307240729));
#40009=CARTESIAN_POINT('Ctrl Pts',(4.04035407891222,-1.,0.175654339673798));
#40010=CARTESIAN_POINT('Ctrl Pts',(4.04035407891222,1.,0.175654339673798));
#40011=CARTESIAN_POINT('Ctrl Pts',(4.03335057326163,-1.,0.172535962484515));
#40012=CARTESIAN_POINT('Ctrl Pts',(4.03335057326163,1.,0.172535962484515));
#40013=CARTESIAN_POINT('Ctrl Pts',(4.02633779703764,-1.,0.169457601001692));
#40014=CARTESIAN_POINT('Ctrl Pts',(4.02633779703764,1.,0.169457601001692));
#40015=CARTESIAN_POINT('Ctrl Pts',(4.01931510507167,-1.,0.166419700015866));
#40016=CARTESIAN_POINT('Ctrl Pts',(4.01931510507167,1.,0.166419700015866));
#40017=CARTESIAN_POINT('Ctrl Pts',(4.01228237022296,-1.,0.163422730287457));
#40018=CARTESIAN_POINT('Ctrl Pts',(4.01228237022296,1.,0.163422730287457));
#40019=CARTESIAN_POINT('Ctrl Pts',(4.00524031064487,-1.,0.160467194882203));
#40020=CARTESIAN_POINT('Ctrl Pts',(4.00524031064487,1.,0.160467194882203));
#40021=CARTESIAN_POINT('Ctrl Pts',(3.9981907463185,-1.,0.15755363438379));
#40022=CARTESIAN_POINT('Ctrl Pts',(3.9981907463185,1.,0.15755363438379));
#40023=CARTESIAN_POINT('Ctrl Pts',(3.99113582086043,-1.,0.154682618338548));
#40024=CARTESIAN_POINT('Ctrl Pts',(3.99113582086043,1.,0.154682618338548));
#40025=CARTESIAN_POINT('Ctrl Pts',(3.98407729850975,-1.,0.151854737441399));
#40026=CARTESIAN_POINT('Ctrl Pts',(3.98407729850975,1.,0.151854737441399));
#40027=CARTESIAN_POINT('Ctrl Pts',(3.97701581473644,-1.,0.149070594803545));
#40028=CARTESIAN_POINT('Ctrl Pts',(3.97701581473644,1.,0.149070594803545));
#40029=CARTESIAN_POINT('Ctrl Pts',(3.96995018565893,-1.,0.146330797814521));
#40030=CARTESIAN_POINT('Ctrl Pts',(3.96995018565893,1.,0.146330797814521));
#40031=CARTESIAN_POINT('Ctrl Pts',(3.96287658098896,-1.,0.143635947692799));
#40032=CARTESIAN_POINT('Ctrl Pts',(3.96287658098896,1.,0.143635947692799));
#40033=CARTESIAN_POINT('Ctrl Pts',(3.95579014116894,-1.,0.140986665829942));
#40034=CARTESIAN_POINT('Ctrl Pts',(3.95579014116894,1.,0.140986665829942));
#40035=CARTESIAN_POINT('Ctrl Pts',(3.94868667844347,-1.,0.138383621255161));
#40036=CARTESIAN_POINT('Ctrl Pts',(3.94868667844347,1.,0.138383621255161));
#40037=CARTESIAN_POINT('Ctrl Pts',(3.94156445130741,-1.,0.135827558661189));
#40038=CARTESIAN_POINT('Ctrl Pts',(3.94156445130741,1.,0.135827558661189));
#40039=CARTESIAN_POINT('Ctrl Pts',(3.93442567551042,-1.,0.133319322794191));
#40040=CARTESIAN_POINT('Ctrl Pts',(3.93442567551042,1.,0.133319322794191));
#40041=CARTESIAN_POINT('Ctrl Pts',(3.92727876795977,-1.,0.130859892027802));
#40042=CARTESIAN_POINT('Ctrl Pts',(3.92727876795977,1.,0.130859892027802));
#40043=CARTESIAN_POINT('Ctrl Pts',(3.92013513251664,-1.,0.128450341339533));
#40044=CARTESIAN_POINT('Ctrl Pts',(3.92013513251664,1.,0.128450341339533));
#40045=CARTESIAN_POINT('Ctrl Pts',(3.91300501605411,-1.,0.126091793324141));
#40046=CARTESIAN_POINT('Ctrl Pts',(3.91300501605411,1.,0.126091793324141));
#40047=CARTESIAN_POINT('Ctrl Pts',(3.90589336320515,-1.,0.12378536827238));
#40048=CARTESIAN_POINT('Ctrl Pts',(3.90589336320515,1.,0.12378536827238));
#40049=CARTESIAN_POINT('Ctrl Pts',(3.89879639336939,-1.,0.121532144765722));
#40050=CARTESIAN_POINT('Ctrl Pts',(3.89879639336939,1.,0.121532144765722));
#40051=CARTESIAN_POINT('Ctrl Pts',(3.8916960010517,-1.,0.119333088190411));
#40052=CARTESIAN_POINT('Ctrl Pts',(3.8916960010517,1.,0.119333088190411));
#40053=CARTESIAN_POINT('Ctrl Pts',(3.88456590045726,-1.,0.117189150373135));
#40054=CARTESIAN_POINT('Ctrl Pts',(3.88456590045726,1.,0.117189150373135));
#40055=CARTESIAN_POINT('Ctrl Pts',(3.87738168405308,-1.,0.115101426649461));
#40056=CARTESIAN_POINT('Ctrl Pts',(3.87738168405308,1.,0.115101426649461));
#40057=CARTESIAN_POINT('Ctrl Pts',(3.87013043445001,-1.,0.113071304914559));
#40058=CARTESIAN_POINT('Ctrl Pts',(3.87013043445001,1.,0.113071304914559));
#40059=CARTESIAN_POINT('Ctrl Pts',(3.86281867282984,-1.,0.111100593036267));
#40060=CARTESIAN_POINT('Ctrl Pts',(3.86281867282984,1.,0.111100593036267));
#40061=CARTESIAN_POINT('Ctrl Pts',(3.85548571496953,-1.,0.109191717634961));
#40062=CARTESIAN_POINT('Ctrl Pts',(3.85548571496953,1.,0.109191717634961));
#40063=CARTESIAN_POINT('Ctrl Pts',(3.84819233070391,-1.,0.107347597812209));
#40064=CARTESIAN_POINT('Ctrl Pts',(3.84819233070391,1.,0.107347597812209));
#40065=CARTESIAN_POINT('Ctrl Pts',(3.84099658324873,-1.,0.105571360916594));
#40066=CARTESIAN_POINT('Ctrl Pts',(3.84099658324873,1.,0.105571360916594));
#40067=CARTESIAN_POINT('Ctrl Pts',(3.83393171228034,-1.,0.103866063811635));
#40068=CARTESIAN_POINT('Ctrl Pts',(3.83393171228034,1.,0.103866063811635));
#40069=CARTESIAN_POINT('Ctrl Pts',(3.8269873714322,-1.,0.102234506488446));
#40070=CARTESIAN_POINT('Ctrl Pts',(3.8269873714322,1.,0.102234506488446));
#40071=CARTESIAN_POINT('Ctrl Pts',(3.82007889742512,-1.,0.100678769650595));
#40072=CARTESIAN_POINT('Ctrl Pts',(3.82007889742512,1.,0.100678769650595));
#40073=CARTESIAN_POINT('Ctrl Pts',(3.81306649386293,-1.,0.0992008728095949));
#40074=CARTESIAN_POINT('Ctrl Pts',(3.81306649386293,1.,0.0992008728095949));
#40075=CARTESIAN_POINT('Ctrl Pts',(3.80581088847642,-1.,0.097804222290608));
#40076=CARTESIAN_POINT('Ctrl Pts',(3.80581088847642,1.,0.097804222290608));
#40077=CARTESIAN_POINT('Ctrl Pts',(3.7982212851376,-1.,0.0964949352872849));
#40078=CARTESIAN_POINT('Ctrl Pts',(3.7982212851376,1.,0.0964949352872849));
#40079=CARTESIAN_POINT('Ctrl Pts',(3.79030016353186,-1.,0.0952829885101074));
#40080=CARTESIAN_POINT('Ctrl Pts',(3.79030016353186,1.,0.0952829885101074));
#40081=CARTESIAN_POINT('Ctrl Pts',(3.78220521899366,-1.,0.0941840095091749));
#40082=CARTESIAN_POINT('Ctrl Pts',(3.78220521899366,1.,0.0941840095091749));
#40083=CARTESIAN_POINT('Ctrl Pts',(3.77424159971456,-1.,0.093218554620458));
#40084=CARTESIAN_POINT('Ctrl Pts',(3.77424159971456,1.,0.093218554620458));
#40085=CARTESIAN_POINT('Ctrl Pts',(3.76678860032228,-1.,0.092409058960406));
#40086=CARTESIAN_POINT('Ctrl Pts',(3.76678860032228,1.,0.092409058960406));
#40087=CARTESIAN_POINT('Ctrl Pts',(3.76024199359493,-1.,0.0917773084999013));
#40088=CARTESIAN_POINT('Ctrl Pts',(3.76024199359493,1.,0.0917773084999013));
#40089=CARTESIAN_POINT('Ctrl Pts',(3.75495560118053,-1.,0.0913419622735858));
#40090=CARTESIAN_POINT('Ctrl Pts',(3.75495560118053,1.,0.0913419622735858));
#40091=CARTESIAN_POINT('Ctrl Pts',(3.75116949194125,-1.,0.0911154000996411));
#40092=CARTESIAN_POINT('Ctrl Pts',(3.75116949194125,1.,0.0911154000996411));
#40093=CARTESIAN_POINT('Ctrl Pts',(3.74943097853257,-1.,0.0911057547504666));
#40094=CARTESIAN_POINT('Ctrl Pts',(3.74943097853257,1.,0.0911057547504666));
#40095=CARTESIAN_POINT('Ctrl Pts',(3.7488701717383,-1.,0.0911958743733931));
#40096=CARTESIAN_POINT('Ctrl Pts',(3.7488701717383,1.,0.0911958743733931));
#40097=CARTESIAN_POINT('Ctrl Pts',(3.74882632118923,-1.,0.0912992005792096));
#40098=CARTESIAN_POINT('Ctrl Pts',(3.74882632118923,1.,0.0912992005792096));
#40099=CARTESIAN_POINT('Ctrl Pts',(3.74888690736767,-1.,0.0913616755937434));
#40100=CARTESIAN_POINT('Ctrl Pts',(3.74888690736767,1.,0.0913616755937434));
#40101=CARTESIAN_POINT('',(3.74888939116259,1.,0.0912596999148864));
#40102=CARTESIAN_POINT('Ctrl Pts',(3.74888939116259,1.,0.0912596999148864));
#40103=CARTESIAN_POINT('Ctrl Pts',(3.74888939116259,0.666666666666667,0.0912596999148864));
#40104=CARTESIAN_POINT('Ctrl Pts',(3.74888939116259,0.333333333333333,0.0912596999148864));
#40105=CARTESIAN_POINT('Ctrl Pts',(3.74888939116259,-0.333333333333333,
0.0912596999148864));
#40106=CARTESIAN_POINT('Ctrl Pts',(3.74888939116259,-0.666666666666667,
0.0912596999148867));
#40107=CARTESIAN_POINT('Ctrl Pts',(3.74888939116259,-1.,0.0912596999148867));
#40108=CARTESIAN_POINT('',(4.1923339003649,1.,0.253646344052522));
#40109=CARTESIAN_POINT('Ctrl Pts',(4.1923339003649,1.,0.253646344052522));
#40110=CARTESIAN_POINT('Ctrl Pts',(4.19097151819684,1.,0.252860861572841));
#40111=CARTESIAN_POINT('Ctrl Pts',(4.18824585245272,1.,0.251293239838441));
#40112=CARTESIAN_POINT('Ctrl Pts',(4.18415464961466,1.,0.248951836912189));
#40113=CARTESIAN_POINT('Ctrl Pts',(4.1786943019518,1.,0.24585003342002));
#40114=CARTESIAN_POINT('Ctrl Pts',(4.17185984411426,1.,0.242006283925089));
#40115=CARTESIAN_POINT('Ctrl Pts',(4.16501636654877,1.,0.238196140934617));
#40116=CARTESIAN_POINT('Ctrl Pts',(4.15816389265352,1.,0.234419749543208));
#40117=CARTESIAN_POINT('Ctrl Pts',(4.15130247434459,1.,0.230677299028384));
#40118=CARTESIAN_POINT('Ctrl Pts',(4.14443220606869,1.,0.226969025060706));
#40119=CARTESIAN_POINT('Ctrl Pts',(4.13755320552764,1.,0.223295201037886));
#40120=CARTESIAN_POINT('Ctrl Pts',(4.13066558697658,1.,0.219656126701542));
#40121=CARTESIAN_POINT('Ctrl Pts',(4.12376943492132,1.,0.216052116898353));
#40122=CARTESIAN_POINT('Ctrl Pts',(4.11686478264739,1.,0.21248349108719));
#40123=CARTESIAN_POINT('Ctrl Pts',(4.10995157639377,1.,0.208950559400393));
#40124=CARTESIAN_POINT('Ctrl Pts',(4.10302969965728,1.,0.205453622198455));
#40125=CARTESIAN_POINT('Ctrl Pts',(4.09609903752152,1.,0.201992979050136));
#40126=CARTESIAN_POINT('Ctrl Pts',(4.08915953359833,1.,0.198568934800862));
#40127=CARTESIAN_POINT('Ctrl Pts',(4.08221124060322,1.,0.195181806054676));
#40128=CARTESIAN_POINT('Ctrl Pts',(4.07525439702992,1.,0.191831928180991));
#40129=CARTESIAN_POINT('Ctrl Pts',(4.06828941192148,1.,0.188519658060156));
#40130=CARTESIAN_POINT('Ctrl Pts',(4.06131670998469,1.,0.185245370038874));
#40131=CARTESIAN_POINT('Ctrl Pts',(4.05433660358353,1.,0.18200945304852));
#40132=CARTESIAN_POINT('Ctrl Pts',(4.04734916719741,1.,0.178812307240729));
#40133=CARTESIAN_POINT('Ctrl Pts',(4.04035407891222,1.,0.175654339673798));
#40134=CARTESIAN_POINT('Ctrl Pts',(4.03335057326163,1.,0.172535962484515));
#40135=CARTESIAN_POINT('Ctrl Pts',(4.02633779703764,1.,0.169457601001692));
#40136=CARTESIAN_POINT('Ctrl Pts',(4.01931510507167,1.,0.166419700015866));
#40137=CARTESIAN_POINT('Ctrl Pts',(4.01228237022296,1.,0.163422730287457));
#40138=CARTESIAN_POINT('Ctrl Pts',(4.00524031064487,1.,0.160467194882203));
#40139=CARTESIAN_POINT('Ctrl Pts',(3.9981907463185,1.,0.15755363438379));
#40140=CARTESIAN_POINT('Ctrl Pts',(3.99113582086043,1.,0.154682618338548));
#40141=CARTESIAN_POINT('Ctrl Pts',(3.98407729850975,1.,0.151854737441399));
#40142=CARTESIAN_POINT('Ctrl Pts',(3.97701581473644,1.,0.149070594803545));
#40143=CARTESIAN_POINT('Ctrl Pts',(3.96995018565893,1.,0.146330797814521));
#40144=CARTESIAN_POINT('Ctrl Pts',(3.96287658098896,1.,0.143635947692799));
#40145=CARTESIAN_POINT('Ctrl Pts',(3.95579014116894,1.,0.140986665829942));
#40146=CARTESIAN_POINT('Ctrl Pts',(3.94868667844347,1.,0.138383621255161));
#40147=CARTESIAN_POINT('Ctrl Pts',(3.94156445130741,1.,0.135827558661189));
#40148=CARTESIAN_POINT('Ctrl Pts',(3.93442567551042,1.,0.133319322794191));
#40149=CARTESIAN_POINT('Ctrl Pts',(3.92727876795977,1.,0.130859892027802));
#40150=CARTESIAN_POINT('Ctrl Pts',(3.92013513251664,1.,0.128450341339533));
#40151=CARTESIAN_POINT('Ctrl Pts',(3.91300501605411,1.,0.126091793324141));
#40152=CARTESIAN_POINT('Ctrl Pts',(3.90589336320515,1.,0.12378536827238));
#40153=CARTESIAN_POINT('Ctrl Pts',(3.89879639336939,1.,0.121532144765722));
#40154=CARTESIAN_POINT('Ctrl Pts',(3.8916960010517,1.,0.119333088190411));
#40155=CARTESIAN_POINT('Ctrl Pts',(3.88456590045726,1.,0.117189150373135));
#40156=CARTESIAN_POINT('Ctrl Pts',(3.87738168405308,1.,0.115101426649461));
#40157=CARTESIAN_POINT('Ctrl Pts',(3.87013043445001,1.,0.113071304914559));
#40158=CARTESIAN_POINT('Ctrl Pts',(3.86281867282984,1.,0.111100593036267));
#40159=CARTESIAN_POINT('Ctrl Pts',(3.85548571496953,1.,0.109191717634961));
#40160=CARTESIAN_POINT('Ctrl Pts',(3.84819233070391,1.,0.107347597812209));
#40161=CARTESIAN_POINT('Ctrl Pts',(3.84099658324873,1.,0.105571360916594));
#40162=CARTESIAN_POINT('Ctrl Pts',(3.83393171228034,1.,0.103866063811635));
#40163=CARTESIAN_POINT('Ctrl Pts',(3.8269873714322,1.,0.102234506488446));
#40164=CARTESIAN_POINT('Ctrl Pts',(3.82007889742512,1.,0.100678769650595));
#40165=CARTESIAN_POINT('Ctrl Pts',(3.81306649386293,1.,0.0992008728095949));
#40166=CARTESIAN_POINT('Ctrl Pts',(3.80581088847642,1.,0.097804222290608));
#40167=CARTESIAN_POINT('Ctrl Pts',(3.7982212851376,1.,0.0964949352872849));
#40168=CARTESIAN_POINT('Ctrl Pts',(3.79030016353186,1.,0.0952829885101074));
#40169=CARTESIAN_POINT('Ctrl Pts',(3.78220521899366,1.,0.0941840095091749));
#40170=CARTESIAN_POINT('Ctrl Pts',(3.77424159971456,1.,0.093218554620458));
#40171=CARTESIAN_POINT('Ctrl Pts',(3.76678860032228,1.,0.092409058960406));
#40172=CARTESIAN_POINT('Ctrl Pts',(3.76024199359493,1.,0.0917773084999013));
#40173=CARTESIAN_POINT('Ctrl Pts',(3.75495560118053,1.,0.0913419622735858));
#40174=CARTESIAN_POINT('Ctrl Pts',(3.75145357872511,1.,0.0911323999576148));
#40175=CARTESIAN_POINT('Ctrl Pts',(3.74976844886495,1.,0.0911090736804576));
#40176=CARTESIAN_POINT('Ctrl Pts',(3.74911539914664,1.,0.091166630180643));
#40177=CARTESIAN_POINT('Ctrl Pts',(3.74892890041021,1.,0.0912308016409239));
#40178=CARTESIAN_POINT('Ctrl Pts',(3.74888939116259,1.,0.0912596999148865));
#40179=CARTESIAN_POINT('',(4.1923339003649,0.,0.253646344052522));
#40180=CARTESIAN_POINT('Ctrl Pts',(3.71702400346349,-1.,0.496218256089213));
#40181=CARTESIAN_POINT('Ctrl Pts',(3.71702400346349,1.,0.496218256089213));
#40182=CARTESIAN_POINT('Ctrl Pts',(3.7169543899574,-1.,0.496270484166409));
#40183=CARTESIAN_POINT('Ctrl Pts',(3.7169543899574,1.,0.496270484166409));
#40184=CARTESIAN_POINT('Ctrl Pts',(3.71698153685602,-1.,0.49637939799264));
#40185=CARTESIAN_POINT('Ctrl Pts',(3.71698153685602,1.,0.49637939799264));
#40186=CARTESIAN_POINT('Ctrl Pts',(3.71752134137482,-1.,0.496556137604533));
#40187=CARTESIAN_POINT('Ctrl Pts',(3.71752134137482,1.,0.496556137604533));
#40188=CARTESIAN_POINT('Ctrl Pts',(3.71923995966302,-1.,0.496818574420596));
#40189=CARTESIAN_POINT('Ctrl Pts',(3.71923995966302,1.,0.496818574420596));
#40190=CARTESIAN_POINT('Ctrl Pts',(3.72301489774398,-1.,0.497187079575988));
#40191=CARTESIAN_POINT('Ctrl Pts',(3.72301489774398,1.,0.497187079575988));
#40192=CARTESIAN_POINT('Ctrl Pts',(3.72830430904606,-1.,0.49758406715305));
#40193=CARTESIAN_POINT('Ctrl Pts',(3.72830430904606,1.,0.49758406715305));
#40194=CARTESIAN_POINT('Ctrl Pts',(3.73486914372449,-1.,0.497984209510025));
#40195=CARTESIAN_POINT('Ctrl Pts',(3.73486914372449,1.,0.497984209510025));
#40196=CARTESIAN_POINT('Ctrl Pts',(3.74235701734714,-1.,0.498350586057693));
#40197=CARTESIAN_POINT('Ctrl Pts',(3.74235701734714,1.,0.498350586057693));
#40198=CARTESIAN_POINT('Ctrl Pts',(3.75037362167839,-1.,0.498642802042606));
#40199=CARTESIAN_POINT('Ctrl Pts',(3.75037362167839,1.,0.498642802042606));
#40200=CARTESIAN_POINT('Ctrl Pts',(3.75854082221053,-1.,0.498823681615422));
#40201=CARTESIAN_POINT('Ctrl Pts',(3.75854082221053,1.,0.498823681615422));
#40202=CARTESIAN_POINT('Ctrl Pts',(3.76655401191229,-1.,0.498865792335291));
#40203=CARTESIAN_POINT('Ctrl Pts',(3.76655401191229,1.,0.498865792335291));
#40204=CARTESIAN_POINT('Ctrl Pts',(3.77425499225255,-1.,0.498759900365892));
#40205=CARTESIAN_POINT('Ctrl Pts',(3.77425499225255,1.,0.498759900365892));
#40206=CARTESIAN_POINT('Ctrl Pts',(3.78163975337356,-1.,0.498515471679585));
#40207=CARTESIAN_POINT('Ctrl Pts',(3.78163975337356,1.,0.498515471679585));
#40208=CARTESIAN_POINT('Ctrl Pts',(3.78879701661264,-1.,0.498152751800959));
#40209=CARTESIAN_POINT('Ctrl Pts',(3.78879701661264,1.,0.498152751800959));
#40210=CARTESIAN_POINT('Ctrl Pts',(3.79586380669994,-1.,0.497696892100625));
#40211=CARTESIAN_POINT('Ctrl Pts',(3.79586380669994,1.,0.497696892100625));
#40212=CARTESIAN_POINT('Ctrl Pts',(3.80297788298514,-1.,0.497171756201052));
#40213=CARTESIAN_POINT('Ctrl Pts',(3.80297788298514,1.,0.497171756201052));
#40214=CARTESIAN_POINT('Ctrl Pts',(3.81022254090839,-1.,0.496592643443704));
#40215=CARTESIAN_POINT('Ctrl Pts',(3.81022254090839,1.,0.496592643443704));
#40216=CARTESIAN_POINT('Ctrl Pts',(3.81760756144025,-1.,0.49596393787548));
#40217=CARTESIAN_POINT('Ctrl Pts',(3.81760756144025,1.,0.49596393787548));
#40218=CARTESIAN_POINT('Ctrl Pts',(3.82509963594103,-1.,0.495283458893838));
#40219=CARTESIAN_POINT('Ctrl Pts',(3.82509963594103,1.,0.495283458893838));
#40220=CARTESIAN_POINT('Ctrl Pts',(3.83264092682431,-1.,0.494545212256402));
#40221=CARTESIAN_POINT('Ctrl Pts',(3.83264092682431,1.,0.494545212256402));
#40222=CARTESIAN_POINT('Ctrl Pts',(3.84017095578451,-1.,0.493742574629135));
#40223=CARTESIAN_POINT('Ctrl Pts',(3.84017095578451,1.,0.493742574629135));
#40224=CARTESIAN_POINT('Ctrl Pts',(3.84765051147999,-1.,0.492871792414141));
#40225=CARTESIAN_POINT('Ctrl Pts',(3.84765051147999,1.,0.492871792414141));
#40226=CARTESIAN_POINT('Ctrl Pts',(3.85507287020263,-1.,0.491933631083814));
#40227=CARTESIAN_POINT('Ctrl Pts',(3.85507287020263,1.,0.491933631083814));
#40228=CARTESIAN_POINT('Ctrl Pts',(3.86245057319246,-1.,0.490931482170891));
#40229=CARTESIAN_POINT('Ctrl Pts',(3.86245057319246,1.,0.490931482170891));
#40230=CARTESIAN_POINT('Ctrl Pts',(3.86980755613707,-1.,0.489870245704918));
#40231=CARTESIAN_POINT('Ctrl Pts',(3.86980755613707,1.,0.489870245704918));
#40232=CARTESIAN_POINT('Ctrl Pts',(3.87716963231109,-1.,0.488754973798274));
#40233=CARTESIAN_POINT('Ctrl Pts',(3.87716963231109,1.,0.488754973798274));
#40234=CARTESIAN_POINT('Ctrl Pts',(3.88455453328138,-1.,0.487589452275155));
#40235=CARTESIAN_POINT('Ctrl Pts',(3.88455453328138,1.,0.487589452275155));
#40236=CARTESIAN_POINT('Ctrl Pts',(3.89196582437552,-1.,0.486375337854104));
#40237=CARTESIAN_POINT('Ctrl Pts',(3.89196582437552,1.,0.486375337854104));
#40238=CARTESIAN_POINT('Ctrl Pts',(3.89939844658513,-1.,0.485112963522223));
#40239=CARTESIAN_POINT('Ctrl Pts',(3.89939844658513,1.,0.485112963522223));
#40240=CARTESIAN_POINT('Ctrl Pts',(3.90684210358056,-1.,0.48380183508915));
#40241=CARTESIAN_POINT('Ctrl Pts',(3.90684210358056,1.,0.48380183508915));
#40242=CARTESIAN_POINT('Ctrl Pts',(3.91428536373751,-1.,0.482441230340714));
#40243=CARTESIAN_POINT('Ctrl Pts',(3.91428536373751,1.,0.482441230340714));
#40244=CARTESIAN_POINT('Ctrl Pts',(3.92171976072341,-1.,0.481030798910749));
#40245=CARTESIAN_POINT('Ctrl Pts',(3.92171976072341,1.,0.481030798910749));
#40246=CARTESIAN_POINT('Ctrl Pts',(3.92914297392071,-1.,0.479571028525579));
#40247=CARTESIAN_POINT('Ctrl Pts',(3.92914297392071,1.,0.479571028525579));
#40248=CARTESIAN_POINT('Ctrl Pts',(3.93655660689819,-1.,0.478062927140965));
#40249=CARTESIAN_POINT('Ctrl Pts',(3.93655660689819,1.,0.478062927140965));
#40250=CARTESIAN_POINT('Ctrl Pts',(3.94396469119383,-1.,0.476507810658538));
#40251=CARTESIAN_POINT('Ctrl Pts',(3.94396469119383,1.,0.476507810658538));
#40252=CARTESIAN_POINT('Ctrl Pts',(3.95137192932897,-1.,0.474907053021791));
#40253=CARTESIAN_POINT('Ctrl Pts',(3.95137192932897,1.,0.474907053021791));
#40254=CARTESIAN_POINT('Ctrl Pts',(3.95878201038338,-1.,0.473261847236298));
#40255=CARTESIAN_POINT('Ctrl Pts',(3.95878201038338,1.,0.473261847236298));
#40256=CARTESIAN_POINT('Ctrl Pts',(3.96619600864643,-1.,0.471572978413504));
#40257=CARTESIAN_POINT('Ctrl Pts',(3.96619600864643,1.,0.471572978413504));
#40258=CARTESIAN_POINT('Ctrl Pts',(3.97361320212436,-1.,0.469840942829896));
#40259=CARTESIAN_POINT('Ctrl Pts',(3.97361320212436,1.,0.469840942829896));
#40260=CARTESIAN_POINT('Ctrl Pts',(3.98103175589371,-1.,0.468066047920158));
#40261=CARTESIAN_POINT('Ctrl Pts',(3.98103175589371,1.,0.468066047920158));
#40262=CARTESIAN_POINT('Ctrl Pts',(3.98844946363262,-1.,0.46624852088304));
#40263=CARTESIAN_POINT('Ctrl Pts',(3.98844946363262,1.,0.46624852088304));
#40264=CARTESIAN_POINT('Ctrl Pts',(3.9958644432011,-1.,0.464388610938976));
#40265=CARTESIAN_POINT('Ctrl Pts',(3.9958644432011,1.,0.464388610938976));
#40266=CARTESIAN_POINT('Ctrl Pts',(4.00327590659075,-1.,0.462486702616205));
#40267=CARTESIAN_POINT('Ctrl Pts',(4.00327590659075,1.,0.462486702616205));
#40268=CARTESIAN_POINT('Ctrl Pts',(4.01068390573399,-1.,0.460543280768515));
#40269=CARTESIAN_POINT('Ctrl Pts',(4.01068390573399,1.,0.460543280768515));
#40270=CARTESIAN_POINT('Ctrl Pts',(4.01808900827587,-1.,0.458558885636946));
#40271=CARTESIAN_POINT('Ctrl Pts',(4.01808900827587,1.,0.458558885636946));
#40272=CARTESIAN_POINT('Ctrl Pts',(4.02549199038394,-1.,0.456534070784951));
#40273=CARTESIAN_POINT('Ctrl Pts',(4.02549199038394,1.,0.456534070784951));
#40274=CARTESIAN_POINT('Ctrl Pts',(4.03289354362794,-1.,0.454469363020542));
#40275=CARTESIAN_POINT('Ctrl Pts',(4.03289354362794,1.,0.454469363020542));
#40276=CARTESIAN_POINT('Ctrl Pts',(4.04029392228049,-1.,0.452365214748893));
#40277=CARTESIAN_POINT('Ctrl Pts',(4.04029392228049,1.,0.452365214748893));
#40278=CARTESIAN_POINT('Ctrl Pts',(4.0476929901813,-1.,0.450222009543927));
#40279=CARTESIAN_POINT('Ctrl Pts',(4.0476929901813,1.,0.450222009543927));
#40280=CARTESIAN_POINT('Ctrl Pts',(4.0550903779696,-1.,0.448040082684115));
#40281=CARTESIAN_POINT('Ctrl Pts',(4.0550903779696,1.,0.448040082684115));
#40282=CARTESIAN_POINT('Ctrl Pts',(4.06248560760659,-1.,0.445819737468538));
#40283=CARTESIAN_POINT('Ctrl Pts',(4.06248560760659,1.,0.445819737468538));
#40284=CARTESIAN_POINT('Ctrl Pts',(4.0698782192569,-1.,0.443561262395333));
#40285=CARTESIAN_POINT('Ctrl Pts',(4.0698782192569,1.,0.443561262395333));
#40286=CARTESIAN_POINT('Ctrl Pts',(4.07726792490016,-1.,0.441264951396361));
#40287=CARTESIAN_POINT('Ctrl Pts',(4.07726792490016,1.,0.441264951396361));
#40288=CARTESIAN_POINT('Ctrl Pts',(4.08465462294273,-1.,0.43893110893128));
#40289=CARTESIAN_POINT('Ctrl Pts',(4.08465462294273,1.,0.43893110893128));
#40290=CARTESIAN_POINT('Ctrl Pts',(4.09203832139089,-1.,0.436560044913483));
#40291=CARTESIAN_POINT('Ctrl Pts',(4.09203832139089,1.,0.436560044913483));
#40292=CARTESIAN_POINT('Ctrl Pts',(4.09941908688373,-1.,0.434152073200461));
#40293=CARTESIAN_POINT('Ctrl Pts',(4.09941908688373,1.,0.434152073200461));
#40294=CARTESIAN_POINT('Ctrl Pts',(4.10679698750336,-1.,0.431707508679884));
#40295=CARTESIAN_POINT('Ctrl Pts',(4.10679698750336,1.,0.431707508679884));
#40296=CARTESIAN_POINT('Ctrl Pts',(4.11417202783267,-1.,0.429226666075845));
#40297=CARTESIAN_POINT('Ctrl Pts',(4.11417202783267,1.,0.429226666075845));
#40298=CARTESIAN_POINT('Ctrl Pts',(4.12154412502007,-1.,0.426709855707001));
#40299=CARTESIAN_POINT('Ctrl Pts',(4.12154412502007,1.,0.426709855707001));
#40300=CARTESIAN_POINT('Ctrl Pts',(4.12891314634572,-1.,0.424157375323976));
#40301=CARTESIAN_POINT('Ctrl Pts',(4.12891314634572,1.,0.424157375323976));
#40302=CARTESIAN_POINT('Ctrl Pts',(4.13627893207002,-1.,0.421569503104513));
#40303=CARTESIAN_POINT('Ctrl Pts',(4.13627893207002,1.,0.421569503104513));
#40304=CARTESIAN_POINT('Ctrl Pts',(4.14364132317121,-1.,0.418946490667703));
#40305=CARTESIAN_POINT('Ctrl Pts',(4.14364132317121,1.,0.418946490667703));
#40306=CARTESIAN_POINT('Ctrl Pts',(4.15100018949965,-1.,0.416288556008012));
#40307=CARTESIAN_POINT('Ctrl Pts',(4.15100018949965,1.,0.416288556008012));
#40308=CARTESIAN_POINT('Ctrl Pts',(4.15835545017202,-1.,0.413595877951471));
#40309=CARTESIAN_POINT('Ctrl Pts',(4.15835545017202,1.,0.413595877951471));
#40310=CARTESIAN_POINT('Ctrl Pts',(4.16570705938425,-1.,0.410868596146415));
#40311=CARTESIAN_POINT('Ctrl Pts',(4.16570705938425,1.,0.410868596146415));
#40312=CARTESIAN_POINT('Ctrl Pts',(4.17158541007977,-1.,0.408659167568273));
#40313=CARTESIAN_POINT('Ctrl Pts',(4.17158541007977,1.,0.408659167568273));
#40314=CARTESIAN_POINT('Ctrl Pts',(4.17599251954382,-1.,0.406986596325455));
#40315=CARTESIAN_POINT('Ctrl Pts',(4.17599251954382,1.,0.406986596325455));
#40316=CARTESIAN_POINT('Ctrl Pts',(4.17892985789466,-1.,0.40586466267921));
#40317=CARTESIAN_POINT('Ctrl Pts',(4.17892985789466,1.,0.40586466267921));
#40318=CARTESIAN_POINT('Ctrl Pts',(4.18039834341342,-1.,0.405301974318351));
#40319=CARTESIAN_POINT('Ctrl Pts',(4.18039834341342,1.,0.405301974318351));
#40320=CARTESIAN_POINT('',(3.71701050416825,1.,0.496319364827592));
#40321=CARTESIAN_POINT('Ctrl Pts',(3.71701050416825,-1.,0.496319364827593));
#40322=CARTESIAN_POINT('Ctrl Pts',(3.71701050416825,-0.666666666666667,
0.496319364827593));
#40323=CARTESIAN_POINT('Ctrl Pts',(3.71701050416825,-0.333333333333333,
0.496319364827593));
#40324=CARTESIAN_POINT('Ctrl Pts',(3.71701050416825,0.333333333333333,0.496319364827593));
#40325=CARTESIAN_POINT('Ctrl Pts',(3.71701050416825,0.666666666666667,0.496319364827593));
#40326=CARTESIAN_POINT('Ctrl Pts',(3.71701050416825,1.,0.496319364827593));
#40327=CARTESIAN_POINT('',(4.18039834341342,1.,0.405301974318351));
#40328=CARTESIAN_POINT('',(4.18039834341342,0.,0.405301974318351));
#40329=CARTESIAN_POINT('Ctrl Pts',(3.71701050416825,1.,0.496319364827592));
#40330=CARTESIAN_POINT('Ctrl Pts',(3.71704500630494,1.,0.496354087924312));
#40331=CARTESIAN_POINT('Ctrl Pts',(3.71721917030355,1.,0.496446644158006));
#40332=CARTESIAN_POINT('Ctrl Pts',(3.71785517607548,1.,0.496605651525989));
#40333=CARTESIAN_POINT('Ctrl Pts',(3.71952320822499,1.,0.496846224822564));
#40334=CARTESIAN_POINT('Ctrl Pts',(3.72301489774398,1.,0.497187079575988));
#40335=CARTESIAN_POINT('Ctrl Pts',(3.72830430904606,1.,0.49758406715305));
#40336=CARTESIAN_POINT('Ctrl Pts',(3.73486914372449,1.,0.497984209510025));
#40337=CARTESIAN_POINT('Ctrl Pts',(3.74235701734714,1.,0.498350586057693));
#40338=CARTESIAN_POINT('Ctrl Pts',(3.75037362167839,1.,0.498642802042606));
#40339=CARTESIAN_POINT('Ctrl Pts',(3.75854082221053,1.,0.498823681615422));
#40340=CARTESIAN_POINT('Ctrl Pts',(3.76655401191229,1.,0.498865792335291));
#40341=CARTESIAN_POINT('Ctrl Pts',(3.77425499225255,1.,0.498759900365892));
#40342=CARTESIAN_POINT('Ctrl Pts',(3.78163975337356,1.,0.498515471679585));
#40343=CARTESIAN_POINT('Ctrl Pts',(3.78879701661264,1.,0.498152751800959));
#40344=CARTESIAN_POINT('Ctrl Pts',(3.79586380669994,1.,0.497696892100625));
#40345=CARTESIAN_POINT('Ctrl Pts',(3.80297788298514,1.,0.497171756201052));
#40346=CARTESIAN_POINT('Ctrl Pts',(3.81022254090839,1.,0.496592643443704));
#40347=CARTESIAN_POINT('Ctrl Pts',(3.81760756144025,1.,0.49596393787548));
#40348=CARTESIAN_POINT('Ctrl Pts',(3.82509963594103,1.,0.495283458893838));
#40349=CARTESIAN_POINT('Ctrl Pts',(3.83264092682431,1.,0.494545212256402));
#40350=CARTESIAN_POINT('Ctrl Pts',(3.84017095578451,1.,0.493742574629135));
#40351=CARTESIAN_POINT('Ctrl Pts',(3.84765051147999,1.,0.492871792414141));
#40352=CARTESIAN_POINT('Ctrl Pts',(3.85507287020263,1.,0.491933631083814));
#40353=CARTESIAN_POINT('Ctrl Pts',(3.86245057319246,1.,0.490931482170891));
#40354=CARTESIAN_POINT('Ctrl Pts',(3.86980755613707,1.,0.489870245704918));
#40355=CARTESIAN_POINT('Ctrl Pts',(3.87716963231109,1.,0.488754973798274));
#40356=CARTESIAN_POINT('Ctrl Pts',(3.88455453328138,1.,0.487589452275155));
#40357=CARTESIAN_POINT('Ctrl Pts',(3.89196582437552,1.,0.486375337854104));
#40358=CARTESIAN_POINT('Ctrl Pts',(3.89939844658513,1.,0.485112963522223));
#40359=CARTESIAN_POINT('Ctrl Pts',(3.90684210358056,1.,0.48380183508915));
#40360=CARTESIAN_POINT('Ctrl Pts',(3.91428536373751,1.,0.482441230340714));
#40361=CARTESIAN_POINT('Ctrl Pts',(3.92171976072341,1.,0.481030798910749));
#40362=CARTESIAN_POINT('Ctrl Pts',(3.92914297392071,1.,0.479571028525579));
#40363=CARTESIAN_POINT('Ctrl Pts',(3.93655660689819,1.,0.478062927140965));
#40364=CARTESIAN_POINT('Ctrl Pts',(3.94396469119383,1.,0.476507810658538));
#40365=CARTESIAN_POINT('Ctrl Pts',(3.95137192932897,1.,0.474907053021791));
#40366=CARTESIAN_POINT('Ctrl Pts',(3.95878201038338,1.,0.473261847236298));
#40367=CARTESIAN_POINT('Ctrl Pts',(3.96619600864643,1.,0.471572978413504));
#40368=CARTESIAN_POINT('Ctrl Pts',(3.97361320212436,1.,0.469840942829896));
#40369=CARTESIAN_POINT('Ctrl Pts',(3.98103175589371,1.,0.468066047920158));
#40370=CARTESIAN_POINT('Ctrl Pts',(3.98844946363262,1.,0.46624852088304));
#40371=CARTESIAN_POINT('Ctrl Pts',(3.9958644432011,1.,0.464388610938976));
#40372=CARTESIAN_POINT('Ctrl Pts',(4.00327590659075,1.,0.462486702616205));
#40373=CARTESIAN_POINT('Ctrl Pts',(4.01068390573399,1.,0.460543280768515));
#40374=CARTESIAN_POINT('Ctrl Pts',(4.01808900827587,1.,0.458558885636946));
#40375=CARTESIAN_POINT('Ctrl Pts',(4.02549199038394,1.,0.456534070784951));
#40376=CARTESIAN_POINT('Ctrl Pts',(4.03289354362794,1.,0.454469363020542));
#40377=CARTESIAN_POINT('Ctrl Pts',(4.04029392228049,1.,0.452365214748893));
#40378=CARTESIAN_POINT('Ctrl Pts',(4.0476929901813,1.,0.450222009543927));
#40379=CARTESIAN_POINT('Ctrl Pts',(4.0550903779696,1.,0.448040082684115));
#40380=CARTESIAN_POINT('Ctrl Pts',(4.06248560760659,1.,0.445819737468538));
#40381=CARTESIAN_POINT('Ctrl Pts',(4.0698782192569,1.,0.443561262395333));
#40382=CARTESIAN_POINT('Ctrl Pts',(4.07726792490016,1.,0.441264951396361));
#40383=CARTESIAN_POINT('Ctrl Pts',(4.08465462294273,1.,0.43893110893128));
#40384=CARTESIAN_POINT('Ctrl Pts',(4.09203832139089,1.,0.436560044913483));
#40385=CARTESIAN_POINT('Ctrl Pts',(4.09941908688373,1.,0.434152073200461));
#40386=CARTESIAN_POINT('Ctrl Pts',(4.10679698750336,1.,0.431707508679884));
#40387=CARTESIAN_POINT('Ctrl Pts',(4.11417202783267,1.,0.429226666075845));
#40388=CARTESIAN_POINT('Ctrl Pts',(4.12154412502007,1.,0.426709855707001));
#40389=CARTESIAN_POINT('Ctrl Pts',(4.12891314634572,1.,0.424157375323976));
#40390=CARTESIAN_POINT('Ctrl Pts',(4.13627893207002,1.,0.421569503104513));
#40391=CARTESIAN_POINT('Ctrl Pts',(4.14364132317121,1.,0.418946490667703));
#40392=CARTESIAN_POINT('Ctrl Pts',(4.15100018949965,1.,0.416288556008012));
#40393=CARTESIAN_POINT('Ctrl Pts',(4.15835545017202,1.,0.413595877951471));
#40394=CARTESIAN_POINT('Ctrl Pts',(4.16570705938425,1.,0.410868596146415));
#40395=CARTESIAN_POINT('Ctrl Pts',(4.17158541007977,1.,0.408659167568273));
#40396=CARTESIAN_POINT('Ctrl Pts',(4.17599251954382,1.,0.406986596325455));
#40397=CARTESIAN_POINT('Ctrl Pts',(4.17892985789466,1.,0.40586466267921));
#40398=CARTESIAN_POINT('Ctrl Pts',(4.18039834341342,1.,0.405301974318351));
#40399=CARTESIAN_POINT('Origin',(4.18039834341342,0.,0.405301974318351));
#40400=CARTESIAN_POINT('',(4.1923339003649,1.,0.253646344052522));
#40401=CARTESIAN_POINT('Origin',(0.,0.,0.));
#40402=CARTESIAN_POINT('',(3.68845817949618,1.,0.676591647973661));
#40403=CARTESIAN_POINT('Origin',(0.,1.,0.));
#40404=CARTESIAN_POINT('Ctrl Pts',(3.68845817949618,1.,0.676591647973661));
#40405=CARTESIAN_POINT('Ctrl Pts',(3.68845817949618,0.666666666666667,0.676591647973661));
#40406=CARTESIAN_POINT('Ctrl Pts',(3.68845817949618,0.333333333333333,0.676591647973661));
#40407=CARTESIAN_POINT('Ctrl Pts',(3.68845817949618,-0.333333333333333,
0.676591647973661));
#40408=CARTESIAN_POINT('Ctrl Pts',(3.68845817949618,-0.666666666666667,
0.676591647973662));
#40409=CARTESIAN_POINT('Ctrl Pts',(3.68845817949618,-1.,0.676591647973662));
#40410=CARTESIAN_POINT('Ctrl Pts',(4.10104028313088,-1.,0.906349047628867));
#40411=CARTESIAN_POINT('Ctrl Pts',(4.10104028313088,1.,0.906349047628867));
#40412=CARTESIAN_POINT('Ctrl Pts',(4.09981755067956,-1.,0.905360112216302));
#40413=CARTESIAN_POINT('Ctrl Pts',(4.09981755067956,1.,0.905360112216302));
#40414=CARTESIAN_POINT('Ctrl Pts',(4.09737067247114,-1.,0.903385402444213));
#40415=CARTESIAN_POINT('Ctrl Pts',(4.09737067247114,1.,0.903385402444213));
#40416=CARTESIAN_POINT('Ctrl Pts',(4.09369611524319,-1.,0.900432820945976));
#40417=CARTESIAN_POINT('Ctrl Pts',(4.09369611524319,1.,0.900432820945976));
#40418=CARTESIAN_POINT('Ctrl Pts',(4.08878822249095,-1.,0.896515019236369));
#40419=CARTESIAN_POINT('Ctrl Pts',(4.08878822249095,1.,0.896515019236369));
#40420=CARTESIAN_POINT('Ctrl Pts',(4.08263920306651,-1.,0.891649447920402));
#40421=CARTESIAN_POINT('Ctrl Pts',(4.08263920306651,1.,0.891649447920402));
#40422=CARTESIAN_POINT('Ctrl Pts',(4.07647601774639,-1.,0.886815658360739));
#40423=CARTESIAN_POINT('Ctrl Pts',(4.07647601774639,1.,0.886815658360739));
#40424=CARTESIAN_POINT('Ctrl Pts',(4.07029866694292,-1.,0.882013797525917));
#40425=CARTESIAN_POINT('Ctrl Pts',(4.07029866694292,1.,0.882013797525917));
#40426=CARTESIAN_POINT('Ctrl Pts',(4.06410717232347,-1.,0.877244060484596));
#40427=CARTESIAN_POINT('Ctrl Pts',(4.06410717232347,1.,0.877244060484596));
#40428=CARTESIAN_POINT('Ctrl Pts',(4.05790159030495,-1.,0.872506694780564));
#40429=CARTESIAN_POINT('Ctrl Pts',(4.05790159030495,1.,0.872506694780564));
#40430=CARTESIAN_POINT('Ctrl Pts',(4.05168199437128,-1.,0.867801988858176));
#40431=CARTESIAN_POINT('Ctrl Pts',(4.05168199437128,1.,0.867801988858176));
#40432=CARTESIAN_POINT('Ctrl Pts',(4.04544845048097,-1.,0.863130256642174));
#40433=CARTESIAN_POINT('Ctrl Pts',(4.04544845048097,1.,0.863130256642174));
#40434=CARTESIAN_POINT('Ctrl Pts',(4.03920099284658,-1.,0.858491822322572));
#40435=CARTESIAN_POINT('Ctrl Pts',(4.03920099284658,1.,0.858491822322572));
#40436=CARTESIAN_POINT('Ctrl Pts',(4.03293960436945,-1.,0.853887006632179));
#40437=CARTESIAN_POINT('Ctrl Pts',(4.03293960436945,1.,0.853887006632179));
#40438=CARTESIAN_POINT('Ctrl Pts',(4.02666418343508,-1.,0.849316107475013));
#40439=CARTESIAN_POINT('Ctrl Pts',(4.02666418343508,1.,0.849316107475013));
#40440=CARTESIAN_POINT('Ctrl Pts',(4.02037456798787,-1.,0.844779403288517));
#40441=CARTESIAN_POINT('Ctrl Pts',(4.02037456798787,1.,0.844779403288517));
#40442=CARTESIAN_POINT('Ctrl Pts',(4.01407059766338,-1.,0.840277171976381));
#40443=CARTESIAN_POINT('Ctrl Pts',(4.01407059766338,1.,0.840277171976381));
#40444=CARTESIAN_POINT('Ctrl Pts',(4.00775216907934,-1.,0.835809705809822));
#40445=CARTESIAN_POINT('Ctrl Pts',(4.00775216907934,1.,0.835809705809822));
#40446=CARTESIAN_POINT('Ctrl Pts',(4.00141928477447,-1.,0.831377325741487));
#40447=CARTESIAN_POINT('Ctrl Pts',(4.00141928477447,1.,0.831377325741487));
#40448=CARTESIAN_POINT('Ctrl Pts',(3.99507212784289,-1.,0.826980400320474));
#40449=CARTESIAN_POINT('Ctrl Pts',(3.99507212784289,1.,0.826980400320474));
#40450=CARTESIAN_POINT('Ctrl Pts',(3.98871104646328,-1.,0.82261934602177));
#40451=CARTESIAN_POINT('Ctrl Pts',(3.98871104646328,1.,0.82261934602177));
#40452=CARTESIAN_POINT('Ctrl Pts',(3.98233640155287,-1.,0.818294599022034));
#40453=CARTESIAN_POINT('Ctrl Pts',(3.98233640155287,1.,0.818294599022034));
#40454=CARTESIAN_POINT('Ctrl Pts',(3.97594844078763,-1.,0.814006592328738));
#40455=CARTESIAN_POINT('Ctrl Pts',(3.97594844078763,1.,0.814006592328738));
#40456=CARTESIAN_POINT('Ctrl Pts',(3.96954717513251,-1.,0.809755732818134));
#40457=CARTESIAN_POINT('Ctrl Pts',(3.96954717513251,1.,0.809755732818134));
#40458=CARTESIAN_POINT('Ctrl Pts',(3.96313222295874,-1.,0.805542372178496));
#40459=CARTESIAN_POINT('Ctrl Pts',(3.96313222295874,1.,0.805542372178496));
#40460=CARTESIAN_POINT('Ctrl Pts',(3.95670276375176,-1.,0.801366797727206));
#40461=CARTESIAN_POINT('Ctrl Pts',(3.95670276375176,1.,0.801366797727206));
#40462=CARTESIAN_POINT('Ctrl Pts',(3.95025788827189,-1.,0.797229296085439));
#40463=CARTESIAN_POINT('Ctrl Pts',(3.95025788827189,1.,0.797229296085439));
#40464=CARTESIAN_POINT('Ctrl Pts',(3.94379688971307,-1.,0.793130205641017));
#40465=CARTESIAN_POINT('Ctrl Pts',(3.94379688971307,1.,0.793130205641017));
#40466=CARTESIAN_POINT('Ctrl Pts',(3.93731956885671,-1.,0.789069971469324));
#40467=CARTESIAN_POINT('Ctrl Pts',(3.93731956885671,1.,0.789069971469324));
#40468=CARTESIAN_POINT('Ctrl Pts',(3.93082655631768,-1.,0.785049202786459));
#40469=CARTESIAN_POINT('Ctrl Pts',(3.93082655631768,1.,0.785049202786459));
#40470=CARTESIAN_POINT('Ctrl Pts',(3.92431956510418,-1.,0.781068718228395));
#40471=CARTESIAN_POINT('Ctrl Pts',(3.92431956510418,1.,0.781068718228395));
#40472=CARTESIAN_POINT('Ctrl Pts',(3.91780062334464,-1.,0.777129415664915));
#40473=CARTESIAN_POINT('Ctrl Pts',(3.91780062334464,1.,0.777129415664915));
#40474=CARTESIAN_POINT('Ctrl Pts',(3.91127138115238,-1.,0.773232154506306));
#40475=CARTESIAN_POINT('Ctrl Pts',(3.91127138115238,1.,0.773232154506306));
#40476=CARTESIAN_POINT('Ctrl Pts',(3.90473237182634,-1.,0.769377629847877));
#40477=CARTESIAN_POINT('Ctrl Pts',(3.90473237182634,1.,0.769377629847877));
#40478=CARTESIAN_POINT('Ctrl Pts',(3.89818233104381,-1.,0.765566256401307));
#40479=CARTESIAN_POINT('Ctrl Pts',(3.89818233104381,1.,0.765566256401307));
#40480=CARTESIAN_POINT('Ctrl Pts',(3.89161738162245,-1.,0.761798028793978));
#40481=CARTESIAN_POINT('Ctrl Pts',(3.89161738162245,1.,0.761798028793978));
#40482=CARTESIAN_POINT('Ctrl Pts',(3.88503262662684,-1.,0.758072800564799));
#40483=CARTESIAN_POINT('Ctrl Pts',(3.88503262662684,1.,0.758072800564799));
#40484=CARTESIAN_POINT('Ctrl Pts',(3.87842382520058,-1.,0.754390577396847));
#40485=CARTESIAN_POINT('Ctrl Pts',(3.87842382520058,1.,0.754390577396847));
#40486=CARTESIAN_POINT('Ctrl Pts',(3.87178914078372,-1.,0.750751822383024));
#40487=CARTESIAN_POINT('Ctrl Pts',(3.87178914078372,1.,0.750751822383024));
#40488=CARTESIAN_POINT('Ctrl Pts',(3.86513062969896,-1.,0.747157716488884));
#40489=CARTESIAN_POINT('Ctrl Pts',(3.86513062969896,1.,0.747157716488884));
#40490=CARTESIAN_POINT('Ctrl Pts',(3.85845645217611,-1.,0.743610542737042));
#40491=CARTESIAN_POINT('Ctrl Pts',(3.85845645217611,1.,0.743610542737042));
#40492=CARTESIAN_POINT('Ctrl Pts',(3.85177770351237,-1.,0.740113146827177));
#40493=CARTESIAN_POINT('Ctrl Pts',(3.85177770351237,1.,0.740113146827177));
#40494=CARTESIAN_POINT('Ctrl Pts',(3.84510432881231,-1.,0.736668240497151));
#40495=CARTESIAN_POINT('Ctrl Pts',(3.84510432881231,1.,0.736668240497151));
#40496=CARTESIAN_POINT('Ctrl Pts',(3.83844103658016,-1.,0.733277703756091));
#40497=CARTESIAN_POINT('Ctrl Pts',(3.83844103658016,1.,0.733277703756091));
#40498=CARTESIAN_POINT('Ctrl Pts',(3.8317839240337,-1.,0.729942010490146));
#40499=CARTESIAN_POINT('Ctrl Pts',(3.8317839240337,1.,0.729942010490146));
#40500=CARTESIAN_POINT('Ctrl Pts',(3.82511495756682,-1.,0.726659281876608));
#40501=CARTESIAN_POINT('Ctrl Pts',(3.82511495756682,1.,0.726659281876608));
#40502=CARTESIAN_POINT('Ctrl Pts',(3.81840802610795,-1.,0.72342634601935));
#40503=CARTESIAN_POINT('Ctrl Pts',(3.81840802610795,1.,0.72342634601935));
#40504=CARTESIAN_POINT('Ctrl Pts',(3.81163885127309,-1.,0.720240466589173));
#40505=CARTESIAN_POINT('Ctrl Pts',(3.81163885127309,1.,0.720240466589173));
#40506=CARTESIAN_POINT('Ctrl Pts',(3.80479445759296,-1.,0.717100993669091));
#40507=CARTESIAN_POINT('Ctrl Pts',(3.80479445759296,1.,0.717100993669091));
#40508=CARTESIAN_POINT('Ctrl Pts',(3.79788100314994,-1.,0.714010733006678));
#40509=CARTESIAN_POINT('Ctrl Pts',(3.79788100314994,1.,0.714010733006678));
#40510=CARTESIAN_POINT('Ctrl Pts',(3.79093694007146,-1.,0.710978231689118));
#40511=CARTESIAN_POINT('Ctrl Pts',(3.79093694007146,1.,0.710978231689118));
#40512=CARTESIAN_POINT('Ctrl Pts',(3.78402183336678,-1.,0.7080158793756));
#40513=CARTESIAN_POINT('Ctrl Pts',(3.78402183336678,1.,0.7080158793756));
#40514=CARTESIAN_POINT('Ctrl Pts',(3.77719254217197,-1.,0.70513584799995));
#40515=CARTESIAN_POINT('Ctrl Pts',(3.77719254217197,1.,0.70513584799995));
#40516=CARTESIAN_POINT('Ctrl Pts',(3.77048141872904,-1.,0.702346356621614));
#40517=CARTESIAN_POINT('Ctrl Pts',(3.77048141872904,1.,0.702346356621614));
#40518=CARTESIAN_POINT('Ctrl Pts',(3.76387780603725,-1.,0.699648552230851));
#40519=CARTESIAN_POINT('Ctrl Pts',(3.76387780603725,1.,0.699648552230851));
#40520=CARTESIAN_POINT('Ctrl Pts',(3.75729775766913,-1.,0.69703124565953));
#40521=CARTESIAN_POINT('Ctrl Pts',(3.75729775766913,1.,0.69703124565953));
#40522=CARTESIAN_POINT('Ctrl Pts',(3.7506028824329,-1.,0.694474562581174));
#40523=CARTESIAN_POINT('Ctrl Pts',(3.7506028824329,1.,0.694474562581174));
#40524=CARTESIAN_POINT('Ctrl Pts',(3.74365508986548,-1.,0.691960080400503));
#40525=CARTESIAN_POINT('Ctrl Pts',(3.74365508986548,1.,0.691960080400503));
#40526=CARTESIAN_POINT('Ctrl Pts',(3.73636374474993,-1.,0.689479637354652));
#40527=CARTESIAN_POINT('Ctrl Pts',(3.73636374474993,1.,0.689479637354652));
#40528=CARTESIAN_POINT('Ctrl Pts',(3.72872973554125,-1.,0.687043475232499));
#40529=CARTESIAN_POINT('Ctrl Pts',(3.72872973554125,1.,0.687043475232499));
#40530=CARTESIAN_POINT('Ctrl Pts',(3.7209063713952,-1.,0.684691698168356));
#40531=CARTESIAN_POINT('Ctrl Pts',(3.7209063713952,1.,0.684691698168356));
#40532=CARTESIAN_POINT('Ctrl Pts',(3.71319182790334,-1.,0.68249234510969));
#40533=CARTESIAN_POINT('Ctrl Pts',(3.71319182790334,1.,0.68249234510969));
#40534=CARTESIAN_POINT('Ctrl Pts',(3.70595722032165,-1.,0.680526909711618));
#40535=CARTESIAN_POINT('Ctrl Pts',(3.70595722032165,1.,0.680526909711618));
#40536=CARTESIAN_POINT('Ctrl Pts',(3.69959004073192,-1.,0.67887882222639));
#40537=CARTESIAN_POINT('Ctrl Pts',(3.69959004073192,1.,0.67887882222639));
#40538=CARTESIAN_POINT('Ctrl Pts',(3.69443683573443,-1.,0.677621861865197));
#40539=CARTESIAN_POINT('Ctrl Pts',(3.69443683573443,1.,0.677621861865197));
#40540=CARTESIAN_POINT('Ctrl Pts',(3.69073278191505,-1.,0.676805811074141));
#40541=CARTESIAN_POINT('Ctrl Pts',(3.69073278191505,1.,0.676805811074141));
#40542=CARTESIAN_POINT('Ctrl Pts',(3.68901718135636,-1.,0.676524321060167));
#40543=CARTESIAN_POINT('Ctrl Pts',(3.68901718135636,1.,0.676524321060167));
#40544=CARTESIAN_POINT('Ctrl Pts',(3.68844918120934,-1.,0.676525601650139));
#40545=CARTESIAN_POINT('Ctrl Pts',(3.68844918120934,1.,0.676525601650139));
#40546=CARTESIAN_POINT('Ctrl Pts',(3.68838970675356,-1.,0.676620796001717));
#40547=CARTESIAN_POINT('Ctrl Pts',(3.68838970675356,1.,0.676620796001717));
#40548=CARTESIAN_POINT('Ctrl Pts',(3.68843977377012,-1.,0.676691979611562));
#40549=CARTESIAN_POINT('Ctrl Pts',(3.68843977377012,1.,0.676691979611562));
#40550=CARTESIAN_POINT('',(4.10104028313088,1.,0.906349047628867));
#40551=CARTESIAN_POINT('Ctrl Pts',(4.10104028313088,1.,0.906349047628867));
#40552=CARTESIAN_POINT('Ctrl Pts',(4.09981755067956,1.,0.905360112216302));
#40553=CARTESIAN_POINT('Ctrl Pts',(4.09737067247114,1.,0.903385402444213));
#40554=CARTESIAN_POINT('Ctrl Pts',(4.09369611524319,1.,0.900432820945976));
#40555=CARTESIAN_POINT('Ctrl Pts',(4.08878822249095,1.,0.896515019236369));
#40556=CARTESIAN_POINT('Ctrl Pts',(4.08263920306651,1.,0.891649447920402));
#40557=CARTESIAN_POINT('Ctrl Pts',(4.07647601774639,1.,0.886815658360739));
#40558=CARTESIAN_POINT('Ctrl Pts',(4.07029866694292,1.,0.882013797525917));
#40559=CARTESIAN_POINT('Ctrl Pts',(4.06410717232347,1.,0.877244060484596));
#40560=CARTESIAN_POINT('Ctrl Pts',(4.05790159030495,1.,0.872506694780564));
#40561=CARTESIAN_POINT('Ctrl Pts',(4.05168199437128,1.,0.867801988858176));
#40562=CARTESIAN_POINT('Ctrl Pts',(4.04544845048097,1.,0.863130256642174));
#40563=CARTESIAN_POINT('Ctrl Pts',(4.03920099284658,1.,0.858491822322572));
#40564=CARTESIAN_POINT('Ctrl Pts',(4.03293960436945,1.,0.853887006632179));
#40565=CARTESIAN_POINT('Ctrl Pts',(4.02666418343508,1.,0.849316107475013));
#40566=CARTESIAN_POINT('Ctrl Pts',(4.02037456798787,1.,0.844779403288517));
#40567=CARTESIAN_POINT('Ctrl Pts',(4.01407059766338,1.,0.840277171976381));
#40568=CARTESIAN_POINT('Ctrl Pts',(4.00775216907934,1.,0.835809705809822));
#40569=CARTESIAN_POINT('Ctrl Pts',(4.00141928477447,1.,0.831377325741487));
#40570=CARTESIAN_POINT('Ctrl Pts',(3.99507212784289,1.,0.826980400320474));
#40571=CARTESIAN_POINT('Ctrl Pts',(3.98871104646328,1.,0.82261934602177));
#40572=CARTESIAN_POINT('Ctrl Pts',(3.98233640155287,1.,0.818294599022034));
#40573=CARTESIAN_POINT('Ctrl Pts',(3.97594844078763,1.,0.814006592328738));
#40574=CARTESIAN_POINT('Ctrl Pts',(3.96954717513251,1.,0.809755732818134));
#40575=CARTESIAN_POINT('Ctrl Pts',(3.96313222295874,1.,0.805542372178496));
#40576=CARTESIAN_POINT('Ctrl Pts',(3.95670276375176,1.,0.801366797727206));
#40577=CARTESIAN_POINT('Ctrl Pts',(3.95025788827189,1.,0.797229296085439));
#40578=CARTESIAN_POINT('Ctrl Pts',(3.94379688971307,1.,0.793130205641017));
#40579=CARTESIAN_POINT('Ctrl Pts',(3.93731956885671,1.,0.789069971469324));
#40580=CARTESIAN_POINT('Ctrl Pts',(3.93082655631768,1.,0.785049202786459));
#40581=CARTESIAN_POINT('Ctrl Pts',(3.92431956510418,1.,0.781068718228395));
#40582=CARTESIAN_POINT('Ctrl Pts',(3.91780062334464,1.,0.777129415664915));
#40583=CARTESIAN_POINT('Ctrl Pts',(3.91127138115238,1.,0.773232154506306));
#40584=CARTESIAN_POINT('Ctrl Pts',(3.90473237182634,1.,0.769377629847877));
#40585=CARTESIAN_POINT('Ctrl Pts',(3.89818233104381,1.,0.765566256401307));
#40586=CARTESIAN_POINT('Ctrl Pts',(3.89161738162245,1.,0.761798028793978));
#40587=CARTESIAN_POINT('Ctrl Pts',(3.88503262662684,1.,0.758072800564799));
#40588=CARTESIAN_POINT('Ctrl Pts',(3.87842382520058,1.,0.754390577396847));
#40589=CARTESIAN_POINT('Ctrl Pts',(3.87178914078372,1.,0.750751822383024));
#40590=CARTESIAN_POINT('Ctrl Pts',(3.86513062969896,1.,0.747157716488884));
#40591=CARTESIAN_POINT('Ctrl Pts',(3.85845645217611,1.,0.743610542737042));
#40592=CARTESIAN_POINT('Ctrl Pts',(3.85177770351237,1.,0.740113146827177));
#40593=CARTESIAN_POINT('Ctrl Pts',(3.84510432881231,1.,0.736668240497151));
#40594=CARTESIAN_POINT('Ctrl Pts',(3.83844103658016,1.,0.733277703756091));
#40595=CARTESIAN_POINT('Ctrl Pts',(3.8317839240337,1.,0.729942010490146));
#40596=CARTESIAN_POINT('Ctrl Pts',(3.82511495756682,1.,0.726659281876608));
#40597=CARTESIAN_POINT('Ctrl Pts',(3.81840802610795,1.,0.72342634601935));
#40598=CARTESIAN_POINT('Ctrl Pts',(3.81163885127309,1.,0.720240466589173));
#40599=CARTESIAN_POINT('Ctrl Pts',(3.80479445759296,1.,0.717100993669091));
#40600=CARTESIAN_POINT('Ctrl Pts',(3.79788100314994,1.,0.714010733006678));
#40601=CARTESIAN_POINT('Ctrl Pts',(3.79093694007146,1.,0.710978231689118));
#40602=CARTESIAN_POINT('Ctrl Pts',(3.78402183336678,1.,0.7080158793756));
#40603=CARTESIAN_POINT('Ctrl Pts',(3.77719254217197,1.,0.70513584799995));
#40604=CARTESIAN_POINT('Ctrl Pts',(3.77048141872904,1.,0.702346356621614));
#40605=CARTESIAN_POINT('Ctrl Pts',(3.76387780603725,1.,0.699648552230851));
#40606=CARTESIAN_POINT('Ctrl Pts',(3.75729775766913,1.,0.69703124565953));
#40607=CARTESIAN_POINT('Ctrl Pts',(3.7506028824329,1.,0.694474562581174));
#40608=CARTESIAN_POINT('Ctrl Pts',(3.74365508986548,1.,0.691960080400503));
#40609=CARTESIAN_POINT('Ctrl Pts',(3.73636374474993,1.,0.689479637354652));
#40610=CARTESIAN_POINT('Ctrl Pts',(3.72872973554125,1.,0.687043475232499));
#40611=CARTESIAN_POINT('Ctrl Pts',(3.7209063713952,1.,0.684691698168356));
#40612=CARTESIAN_POINT('Ctrl Pts',(3.71319182790334,1.,0.68249234510969));
#40613=CARTESIAN_POINT('Ctrl Pts',(3.70595722032165,1.,0.680526909711618));
#40614=CARTESIAN_POINT('Ctrl Pts',(3.69959004073192,1.,0.67887882222639));
#40615=CARTESIAN_POINT('Ctrl Pts',(3.69443683573443,1.,0.677621861865197));
#40616=CARTESIAN_POINT('Ctrl Pts',(3.6910107117555,1.,0.676867042599712));
#40617=CARTESIAN_POINT('Ctrl Pts',(3.68934997767391,1.,0.676580391119535));
#40618=CARTESIAN_POINT('Ctrl Pts',(3.68869596426099,1.,0.676535079520366));
#40619=CARTESIAN_POINT('Ctrl Pts',(3.68850172300543,1.,0.67656928609342));
#40620=CARTESIAN_POINT('Ctrl Pts',(3.68845817949618,1.,0.676591647973661));
#40621=CARTESIAN_POINT('',(4.10104028313088,0.,0.906349047628867));
#40622=CARTESIAN_POINT('Ctrl Pts',(3.59363563249864,-1.,1.07157964745328));
#40623=CARTESIAN_POINT('Ctrl Pts',(3.59363563249864,1.,1.07157964745328));
#40624=CARTESIAN_POINT('Ctrl Pts',(3.59355870577901,-1.,1.07162034256459));
#40625=CARTESIAN_POINT('Ctrl Pts',(3.59355870577901,1.,1.07162034256459));
#40626=CARTESIAN_POINT('Ctrl Pts',(3.59356848057812,-1.,1.07173216219145));
#40627=CARTESIAN_POINT('Ctrl Pts',(3.59356848057812,1.,1.07173216219145));
#40628=CARTESIAN_POINT('Ctrl Pts',(3.5940739910409,-1.,1.07199116987656));
#40629=CARTESIAN_POINT('Ctrl Pts',(3.5940739910409,1.,1.07199116987656));
#40630=CARTESIAN_POINT('Ctrl Pts',(3.59573039612316,-1.,1.07251922679245));
#40631=CARTESIAN_POINT('Ctrl Pts',(3.59573039612316,1.,1.07251922679245));
#40632=CARTESIAN_POINT('Ctrl Pts',(3.59940121154535,-1.,1.07347372545714));
#40633=CARTESIAN_POINT('Ctrl Pts',(3.59940121154535,1.,1.07347372545714));
#40634=CARTESIAN_POINT('Ctrl Pts',(3.60456339887778,-1.,1.07469327168578));
#40635=CARTESIAN_POINT('Ctrl Pts',(3.60456339887778,1.,1.07469327168578));
#40636=CARTESIAN_POINT('Ctrl Pts',(3.61098481349204,-1.,1.07611545402734));
#40637=CARTESIAN_POINT('Ctrl Pts',(3.61098481349204,1.,1.07611545402734));
#40638=CARTESIAN_POINT('Ctrl Pts',(3.61832318504574,-1.,1.07764868137619));
#40639=CARTESIAN_POINT('Ctrl Pts',(3.61832318504574,1.,1.07764868137619));
#40640=CARTESIAN_POINT('Ctrl Pts',(3.62619537902361,-1.,1.07919137290742));
#40641=CARTESIAN_POINT('Ctrl Pts',(3.62619537902361,1.,1.07919137290742));
#40642=CARTESIAN_POINT('Ctrl Pts',(3.63423373196529,-1.,1.08064765719867));
#40643=CARTESIAN_POINT('Ctrl Pts',(3.63423373196529,1.,1.08064765719867));
#40644=CARTESIAN_POINT('Ctrl Pts',(3.64214167843677,-1.,1.08194278850996));
#40645=CARTESIAN_POINT('Ctrl Pts',(3.64214167843677,1.,1.08194278850996));
#40646=CARTESIAN_POINT('Ctrl Pts',(3.64976441208358,-1.,1.08304289898623));
#40647=CARTESIAN_POINT('Ctrl Pts',(3.64976441208358,1.,1.08304289898623));
#40648=CARTESIAN_POINT('Ctrl Pts',(3.65709649161166,-1.,1.08395671077807));
#40649=CARTESIAN_POINT('Ctrl Pts',(3.65709649161166,1.,1.08395671077807));
#40650=CARTESIAN_POINT('Ctrl Pts',(3.66422237895365,-1.,1.08471809922901));
#40651=CARTESIAN_POINT('Ctrl Pts',(3.66422237895365,1.,1.08471809922901));
#40652=CARTESIAN_POINT('Ctrl Pts',(3.67127347729666,-1.,1.0853733414449));
#40653=CARTESIAN_POINT('Ctrl Pts',(3.67127347729666,1.,1.0853733414449));
#40654=CARTESIAN_POINT('Ctrl Pts',(3.67838211685117,-1.,1.0859675575576));
#40655=CARTESIAN_POINT('Ctrl Pts',(3.67838211685117,1.,1.0859675575576));
#40656=CARTESIAN_POINT('Ctrl Pts',(3.68562817420797,-1.,1.0865288888259));
#40657=CARTESIAN_POINT('Ctrl Pts',(3.68562817420797,1.,1.0865288888259));
#40658=CARTESIAN_POINT('Ctrl Pts',(3.69302062410157,-1.,1.08706319540271));
#40659=CARTESIAN_POINT('Ctrl Pts',(3.69302062410157,1.,1.08706319540271));
#40660=CARTESIAN_POINT('Ctrl Pts',(3.70052690909833,-1.,1.08756311291309));
#40661=CARTESIAN_POINT('Ctrl Pts',(3.70052690909833,1.,1.08756311291309));
#40662=CARTESIAN_POINT('Ctrl Pts',(3.70809084139457,-1.,1.08801367312185));
#40663=CARTESIAN_POINT('Ctrl Pts',(3.70809084139457,1.,1.08801367312185));
#40664=CARTESIAN_POINT('Ctrl Pts',(3.71565372339075,-1.,1.0883988733478));
#40665=CARTESIAN_POINT('Ctrl Pts',(3.71565372339075,1.,1.0883988733478));
#40666=CARTESIAN_POINT('Ctrl Pts',(3.72317741369398,-1.,1.08870887220082));
#40667=CARTESIAN_POINT('Ctrl Pts',(3.72317741369398,1.,1.08870887220082));
#40668=CARTESIAN_POINT('Ctrl Pts',(3.73065515162988,-1.,1.08894337390937));
#40669=CARTESIAN_POINT('Ctrl Pts',(3.73065515162988,1.,1.08894337390937));
#40670=CARTESIAN_POINT('Ctrl Pts',(3.73809879348239,-1.,1.08910769013298));
#40671=CARTESIAN_POINT('Ctrl Pts',(3.73809879348239,1.,1.08910769013298));
#40672=CARTESIAN_POINT('Ctrl Pts',(3.74553121371757,-1.,1.08921040494017));
#40673=CARTESIAN_POINT('Ctrl Pts',(3.74553121371757,1.,1.08921040494017));
#40674=CARTESIAN_POINT('Ctrl Pts',(3.75297711748132,-1.,1.08926054632925));
#40675=CARTESIAN_POINT('Ctrl Pts',(3.75297711748132,1.,1.08926054632925));
#40676=CARTESIAN_POINT('Ctrl Pts',(3.76045342580208,-1.,1.08926462734282));
#40677=CARTESIAN_POINT('Ctrl Pts',(3.76045342580208,1.,1.08926462734282));
#40678=CARTESIAN_POINT('Ctrl Pts',(3.76796340094448,-1.,1.08922484204256));
#40679=CARTESIAN_POINT('Ctrl Pts',(3.76796340094448,1.,1.08922484204256));
#40680=CARTESIAN_POINT('Ctrl Pts',(3.77550199409424,-1.,1.0891407279127));
#40681=CARTESIAN_POINT('Ctrl Pts',(3.77550199409424,1.,1.0891407279127));
#40682=CARTESIAN_POINT('Ctrl Pts',(3.78305911299504,-1.,1.08901018614636));
#40683=CARTESIAN_POINT('Ctrl Pts',(3.78305911299504,1.,1.08901018614636));
#40684=CARTESIAN_POINT('Ctrl Pts',(3.79062357974404,-1.,1.08883071512098));
#40685=CARTESIAN_POINT('Ctrl Pts',(3.79062357974404,1.,1.08883071512098));
#40686=CARTESIAN_POINT('Ctrl Pts',(3.79818708705259,-1.,1.08860064435778));
#40687=CARTESIAN_POINT('Ctrl Pts',(3.79818708705259,1.,1.08860064435778));
#40688=CARTESIAN_POINT('Ctrl Pts',(3.8057472665766,-1.,1.0883200925538));
#40689=CARTESIAN_POINT('Ctrl Pts',(3.8057472665766,1.,1.0883200925538));
#40690=CARTESIAN_POINT('Ctrl Pts',(3.81330554446323,-1.,1.08799030610862));
#40691=CARTESIAN_POINT('Ctrl Pts',(3.81330554446323,1.,1.08799030610862));
#40692=CARTESIAN_POINT('Ctrl Pts',(3.82086569676319,-1.,1.08761321539442));
#40693=CARTESIAN_POINT('Ctrl Pts',(3.82086569676319,1.,1.08761321539442));
#40694=CARTESIAN_POINT('Ctrl Pts',(3.82843215316984,-1.,1.08719091307558));
#40695=CARTESIAN_POINT('Ctrl Pts',(3.82843215316984,1.,1.08719091307558));
#40696=CARTESIAN_POINT('Ctrl Pts',(3.83600837071708,-1.,1.08672515456902));
#40697=CARTESIAN_POINT('Ctrl Pts',(3.83600837071708,1.,1.08672515456902));
#40698=CARTESIAN_POINT('Ctrl Pts',(3.8435952876495,-1.,1.08621688337604));
#40699=CARTESIAN_POINT('Ctrl Pts',(3.8435952876495,1.,1.08621688337604));
#40700=CARTESIAN_POINT('Ctrl Pts',(3.85119211322755,-1.,1.08566647671844));
#40701=CARTESIAN_POINT('Ctrl Pts',(3.85119211322755,1.,1.08566647671844));
#40702=CARTESIAN_POINT('Ctrl Pts',(3.85879698702532,-1.,1.08507395120059));
#40703=CARTESIAN_POINT('Ctrl Pts',(3.85879698702532,1.,1.08507395120059));
#40704=CARTESIAN_POINT('Ctrl Pts',(3.86640769434274,-1.,1.08443918607927));
#40705=CARTESIAN_POINT('Ctrl Pts',(3.86640769434274,1.,1.08443918607927));
#40706=CARTESIAN_POINT('Ctrl Pts',(3.8740223372254,-1.,1.08376213307504));
#40707=CARTESIAN_POINT('Ctrl Pts',(3.8740223372254,1.,1.08376213307504));
#40708=CARTESIAN_POINT('Ctrl Pts',(3.88164007721312,-1.,1.08304304871029));
#40709=CARTESIAN_POINT('Ctrl Pts',(3.88164007721312,1.,1.08304304871029));
#40710=CARTESIAN_POINT('Ctrl Pts',(3.88926088975114,-1.,1.08228241999346));
#40711=CARTESIAN_POINT('Ctrl Pts',(3.88926088975114,1.,1.08228241999346));
#40712=CARTESIAN_POINT('Ctrl Pts',(3.8968852509835,-1.,1.08148086931358));
#40713=CARTESIAN_POINT('Ctrl Pts',(3.8968852509835,1.,1.08148086931358));
#40714=CARTESIAN_POINT('Ctrl Pts',(3.90451384092545,-1.,1.08063906483818));
#40715=CARTESIAN_POINT('Ctrl Pts',(3.90451384092545,1.,1.08063906483818));
#40716=CARTESIAN_POINT('Ctrl Pts',(3.91214726022143,-1.,1.07975763507473));
#40717=CARTESIAN_POINT('Ctrl Pts',(3.91214726022143,1.,1.07975763507473));
#40718=CARTESIAN_POINT('Ctrl Pts',(3.91978568924178,-1.,1.07883706663554));
#40719=CARTESIAN_POINT('Ctrl Pts',(3.91978568924178,1.,1.07883706663554));
#40720=CARTESIAN_POINT('Ctrl Pts',(3.9274289334984,-1.,1.07787771707195));
#40721=CARTESIAN_POINT('Ctrl Pts',(3.9274289334984,1.,1.07787771707195));
#40722=CARTESIAN_POINT('Ctrl Pts',(3.93507657572883,-1.,1.07687985975384));
#40723=CARTESIAN_POINT('Ctrl Pts',(3.93507657572883,1.,1.07687985975384));
#40724=CARTESIAN_POINT('Ctrl Pts',(3.94272809633331,-1.,1.07584371946443));
#40725=CARTESIAN_POINT('Ctrl Pts',(3.94272809633331,1.,1.07584371946443));
#40726=CARTESIAN_POINT('Ctrl Pts',(3.95038299600676,-1.,1.07476950921587));
#40727=CARTESIAN_POINT('Ctrl Pts',(3.95038299600676,1.,1.07476950921587));
#40728=CARTESIAN_POINT('Ctrl Pts',(3.95804094429373,-1.,1.07365747426491));
#40729=CARTESIAN_POINT('Ctrl Pts',(3.95804094429373,1.,1.07365747426491));
#40730=CARTESIAN_POINT('Ctrl Pts',(3.96570179322338,-1.,1.07250789943007));
#40731=CARTESIAN_POINT('Ctrl Pts',(3.96570179322338,1.,1.07250789943007));
#40732=CARTESIAN_POINT('Ctrl Pts',(3.9733655022223,-1.,1.07132109206164));
#40733=CARTESIAN_POINT('Ctrl Pts',(3.9733655022223,1.,1.07132109206164));
#40734=CARTESIAN_POINT('Ctrl Pts',(3.98103208801101,-1.,1.07009737257767));
#40735=CARTESIAN_POINT('Ctrl Pts',(3.98103208801101,1.,1.07009737257767));
#40736=CARTESIAN_POINT('Ctrl Pts',(3.98870156857412,-1.,1.06883706263942));
#40737=CARTESIAN_POINT('Ctrl Pts',(3.98870156857412,1.,1.06883706263942));
#40738=CARTESIAN_POINT('Ctrl Pts',(3.99637389920441,-1.,1.06754047381312));
#40739=CARTESIAN_POINT('Ctrl Pts',(3.99637389920441,1.,1.06754047381312));
#40740=CARTESIAN_POINT('Ctrl Pts',(4.00404894952579,-1.,1.06620789963606));
#40741=CARTESIAN_POINT('Ctrl Pts',(4.00404894952579,1.,1.06620789963606));
#40742=CARTESIAN_POINT('Ctrl Pts',(4.01172654187398,-1.,1.0648396134311));
#40743=CARTESIAN_POINT('Ctrl Pts',(4.01172654187398,1.,1.0648396134311));
#40744=CARTESIAN_POINT('Ctrl Pts',(4.01940647495943,-1.,1.06343586496236));
#40745=CARTESIAN_POINT('Ctrl Pts',(4.01940647495943,1.,1.06343586496236));
#40746=CARTESIAN_POINT('Ctrl Pts',(4.02708855235633,-1.,1.06199687787462));
#40747=CARTESIAN_POINT('Ctrl Pts',(4.02708855235633,1.,1.06199687787462));
#40748=CARTESIAN_POINT('Ctrl Pts',(4.03477261141553,-1.,1.06052284711857));
#40749=CARTESIAN_POINT('Ctrl Pts',(4.03477261141553,1.,1.06052284711857));
#40750=CARTESIAN_POINT('Ctrl Pts',(4.04245854427496,-1.,1.05901393666567));
#40751=CARTESIAN_POINT('Ctrl Pts',(4.04245854427496,1.,1.05901393666567));
#40752=CARTESIAN_POINT('Ctrl Pts',(4.05014628384869,-1.,1.05747027727959));
#40753=CARTESIAN_POINT('Ctrl Pts',(4.05014628384869,1.,1.05747027727959));
#40754=CARTESIAN_POINT('Ctrl Pts',(4.05629789307025,-1.,1.05620762707996));
#40755=CARTESIAN_POINT('Ctrl Pts',(4.05629789307025,1.,1.05620762707996));
#40756=CARTESIAN_POINT('Ctrl Pts',(4.06091239149123,-1.,1.055245071776));
#40757=CARTESIAN_POINT('Ctrl Pts',(4.06091239149123,1.,1.055245071776));
#40758=CARTESIAN_POINT('Ctrl Pts',(4.06398907542249,-1.,1.05459645194823));
#40759=CARTESIAN_POINT('Ctrl Pts',(4.06398907542249,1.,1.05459645194823));
#40760=CARTESIAN_POINT('Ctrl Pts',(4.06552750530042,-1.,1.05427041296137));
#40761=CARTESIAN_POINT('Ctrl Pts',(4.06552750530042,1.,1.05427041296137));
#40762=CARTESIAN_POINT('',(3.59360648251073,1.,1.07167739962028));
#40763=CARTESIAN_POINT('Ctrl Pts',(3.59360648251073,-1.,1.07167739962028));
#40764=CARTESIAN_POINT('Ctrl Pts',(3.59360648251073,-0.666666666666667,
1.07167739962028));
#40765=CARTESIAN_POINT('Ctrl Pts',(3.59360648251073,-0.333333333333333,
1.07167739962028));
#40766=CARTESIAN_POINT('Ctrl Pts',(3.59360648251073,0.333333333333333,1.07167739962028));
#40767=CARTESIAN_POINT('Ctrl Pts',(3.59360648251073,0.666666666666667,1.07167739962028));
#40768=CARTESIAN_POINT('Ctrl Pts',(3.59360648251073,1.,1.07167739962028));
#40769=CARTESIAN_POINT('',(4.06552750530042,1.,1.05427041296137));
#40770=CARTESIAN_POINT('',(4.06552750530042,0.,1.05427041296137));
#40771=CARTESIAN_POINT('Ctrl Pts',(3.59360648251073,1.,1.07167739962028));
#40772=CARTESIAN_POINT('Ctrl Pts',(3.5936351279798,1.,1.07171709254135));
#40773=CARTESIAN_POINT('Ctrl Pts',(3.59379266874567,1.,1.07183575450617));
#40774=CARTESIAN_POINT('Ctrl Pts',(3.59439596999862,1.,1.07209229745229));
#40775=CARTESIAN_POINT('Ctrl Pts',(3.59600583194946,1.,1.07259084660936));
#40776=CARTESIAN_POINT('Ctrl Pts',(3.59940121154535,1.,1.07347372545714));
#40777=CARTESIAN_POINT('Ctrl Pts',(3.60456339887778,1.,1.07469327168578));
#40778=CARTESIAN_POINT('Ctrl Pts',(3.61098481349204,1.,1.07611545402734));
#40779=CARTESIAN_POINT('Ctrl Pts',(3.61832318504574,1.,1.07764868137619));
#40780=CARTESIAN_POINT('Ctrl Pts',(3.62619537902361,1.,1.07919137290742));
#40781=CARTESIAN_POINT('Ctrl Pts',(3.63423373196529,1.,1.08064765719867));
#40782=CARTESIAN_POINT('Ctrl Pts',(3.64214167843677,1.,1.08194278850996));
#40783=CARTESIAN_POINT('Ctrl Pts',(3.64976441208358,1.,1.08304289898623));
#40784=CARTESIAN_POINT('Ctrl Pts',(3.65709649161166,1.,1.08395671077807));
#40785=CARTESIAN_POINT('Ctrl Pts',(3.66422237895365,1.,1.08471809922901));
#40786=CARTESIAN_POINT('Ctrl Pts',(3.67127347729666,1.,1.0853733414449));
#40787=CARTESIAN_POINT('Ctrl Pts',(3.67838211685117,1.,1.0859675575576));
#40788=CARTESIAN_POINT('Ctrl Pts',(3.68562817420797,1.,1.0865288888259));
#40789=CARTESIAN_POINT('Ctrl Pts',(3.69302062410157,1.,1.08706319540271));
#40790=CARTESIAN_POINT('Ctrl Pts',(3.70052690909833,1.,1.08756311291309));
#40791=CARTESIAN_POINT('Ctrl Pts',(3.70809084139457,1.,1.08801367312185));
#40792=CARTESIAN_POINT('Ctrl Pts',(3.71565372339075,1.,1.0883988733478));
#40793=CARTESIAN_POINT('Ctrl Pts',(3.72317741369398,1.,1.08870887220082));
#40794=CARTESIAN_POINT('Ctrl Pts',(3.73065515162988,1.,1.08894337390937));
#40795=CARTESIAN_POINT('Ctrl Pts',(3.73809879348239,1.,1.08910769013298));
#40796=CARTESIAN_POINT('Ctrl Pts',(3.74553121371757,1.,1.08921040494017));
#40797=CARTESIAN_POINT('Ctrl Pts',(3.75297711748132,1.,1.08926054632925));
#40798=CARTESIAN_POINT('Ctrl Pts',(3.76045342580208,1.,1.08926462734282));
#40799=CARTESIAN_POINT('Ctrl Pts',(3.76796340094448,1.,1.08922484204256));
#40800=CARTESIAN_POINT('Ctrl Pts',(3.77550199409424,1.,1.0891407279127));
#40801=CARTESIAN_POINT('Ctrl Pts',(3.78305911299504,1.,1.08901018614636));
#40802=CARTESIAN_POINT('Ctrl Pts',(3.79062357974404,1.,1.08883071512098));
#40803=CARTESIAN_POINT('Ctrl Pts',(3.79818708705259,1.,1.08860064435778));
#40804=CARTESIAN_POINT('Ctrl Pts',(3.8057472665766,1.,1.0883200925538));
#40805=CARTESIAN_POINT('Ctrl Pts',(3.81330554446323,1.,1.08799030610862));
#40806=CARTESIAN_POINT('Ctrl Pts',(3.82086569676319,1.,1.08761321539442));
#40807=CARTESIAN_POINT('Ctrl Pts',(3.82843215316984,1.,1.08719091307558));
#40808=CARTESIAN_POINT('Ctrl Pts',(3.83600837071708,1.,1.08672515456902));
#40809=CARTESIAN_POINT('Ctrl Pts',(3.8435952876495,1.,1.08621688337604));
#40810=CARTESIAN_POINT('Ctrl Pts',(3.85119211322755,1.,1.08566647671844));
#40811=CARTESIAN_POINT('Ctrl Pts',(3.85879698702532,1.,1.08507395120059));
#40812=CARTESIAN_POINT('Ctrl Pts',(3.86640769434274,1.,1.08443918607927));
#40813=CARTESIAN_POINT('Ctrl Pts',(3.8740223372254,1.,1.08376213307504));
#40814=CARTESIAN_POINT('Ctrl Pts',(3.88164007721312,1.,1.08304304871029));
#40815=CARTESIAN_POINT('Ctrl Pts',(3.88926088975114,1.,1.08228241999346));
#40816=CARTESIAN_POINT('Ctrl Pts',(3.8968852509835,1.,1.08148086931358));
#40817=CARTESIAN_POINT('Ctrl Pts',(3.90451384092545,1.,1.08063906483818));
#40818=CARTESIAN_POINT('Ctrl Pts',(3.91214726022143,1.,1.07975763507473));
#40819=CARTESIAN_POINT('Ctrl Pts',(3.91978568924178,1.,1.07883706663554));
#40820=CARTESIAN_POINT('Ctrl Pts',(3.9274289334984,1.,1.07787771707195));
#40821=CARTESIAN_POINT('Ctrl Pts',(3.93507657572883,1.,1.07687985975384));
#40822=CARTESIAN_POINT('Ctrl Pts',(3.94272809633331,1.,1.07584371946443));
#40823=CARTESIAN_POINT('Ctrl Pts',(3.95038299600676,1.,1.07476950921587));
#40824=CARTESIAN_POINT('Ctrl Pts',(3.95804094429373,1.,1.07365747426491));
#40825=CARTESIAN_POINT('Ctrl Pts',(3.96570179322338,1.,1.07250789943007));
#40826=CARTESIAN_POINT('Ctrl Pts',(3.9733655022223,1.,1.07132109206164));
#40827=CARTESIAN_POINT('Ctrl Pts',(3.98103208801101,1.,1.07009737257767));
#40828=CARTESIAN_POINT('Ctrl Pts',(3.98870156857412,1.,1.06883706263942));
#40829=CARTESIAN_POINT('Ctrl Pts',(3.99637389920441,1.,1.06754047381312));
#40830=CARTESIAN_POINT('Ctrl Pts',(4.00404894952579,1.,1.06620789963606));
#40831=CARTESIAN_POINT('Ctrl Pts',(4.01172654187398,1.,1.0648396134311));
#40832=CARTESIAN_POINT('Ctrl Pts',(4.01940647495943,1.,1.06343586496236));
#40833=CARTESIAN_POINT('Ctrl Pts',(4.02708855235633,1.,1.06199687787462));
#40834=CARTESIAN_POINT('Ctrl Pts',(4.03477261141553,1.,1.06052284711857));
#40835=CARTESIAN_POINT('Ctrl Pts',(4.04245854427496,1.,1.05901393666567));
#40836=CARTESIAN_POINT('Ctrl Pts',(4.05014628384869,1.,1.05747027727959));
#40837=CARTESIAN_POINT('Ctrl Pts',(4.05629789307025,1.,1.05620762707996));
#40838=CARTESIAN_POINT('Ctrl Pts',(4.06091239149123,1.,1.055245071776));
#40839=CARTESIAN_POINT('Ctrl Pts',(4.06398907542249,1.,1.05459645194823));
#40840=CARTESIAN_POINT('Ctrl Pts',(4.06552750530042,1.,1.05427041296137));
#40841=CARTESIAN_POINT('Origin',(4.06552750530042,0.,1.05427041296137));
#40842=CARTESIAN_POINT('',(4.10104028313088,1.,0.906349047628867));
#40843=CARTESIAN_POINT('Origin',(0.,0.,0.));
#40844=CARTESIAN_POINT('',(3.5372048861597,1.,1.24526366418038));
#40845=CARTESIAN_POINT('Origin',(0.,1.,0.));
#40846=CARTESIAN_POINT('Ctrl Pts',(3.5372048861597,1.,1.24526366418038));
#40847=CARTESIAN_POINT('Ctrl Pts',(3.5372048861597,0.666666666666667,1.24526366418038));
#40848=CARTESIAN_POINT('Ctrl Pts',(3.5372048861597,0.333333333333333,1.24526366418038));
#40849=CARTESIAN_POINT('Ctrl Pts',(3.5372048861597,-0.333333333333333,1.24526366418038));
#40850=CARTESIAN_POINT('Ctrl Pts',(3.5372048861597,-0.666666666666667,1.24526366418038));
#40851=CARTESIAN_POINT('Ctrl Pts',(3.5372048861597,-1.,1.24526366418038));
#40852=CARTESIAN_POINT('Ctrl Pts',(3.90876544355381,-1.,1.53673442965256));
#40853=CARTESIAN_POINT('Ctrl Pts',(3.90876544355381,1.,1.53673442965256));
#40854=CARTESIAN_POINT('Ctrl Pts',(3.90771246855019,-1.,1.53556639217905));
#40855=CARTESIAN_POINT('Ctrl Pts',(3.90771246855019,1.,1.53556639217905));
#40856=CARTESIAN_POINT('Ctrl Pts',(3.90560462813969,-1.,1.53323321827755));
#40857=CARTESIAN_POINT('Ctrl Pts',(3.90560462813969,1.,1.53323321827755));
#40858=CARTESIAN_POINT('Ctrl Pts',(3.90243719631596,-1.,1.52974216056287));
#40859=CARTESIAN_POINT('Ctrl Pts',(3.90243719631596,1.,1.52974216056287));
#40860=CARTESIAN_POINT('Ctrl Pts',(3.89820260708225,-1.,1.52510482991635));
#40861=CARTESIAN_POINT('Ctrl Pts',(3.89820260708225,1.,1.52510482991635));
#40862=CARTESIAN_POINT('Ctrl Pts',(3.89289043533657,-1.,1.51933724329306));
#40863=CARTESIAN_POINT('Ctrl Pts',(3.89289043533657,1.,1.51933724329306));
#40864=CARTESIAN_POINT('Ctrl Pts',(3.88755930033884,-1.,1.51359883110559));
#40865=CARTESIAN_POINT('Ctrl Pts',(3.88755930033884,1.,1.51359883110559));
#40866=CARTESIAN_POINT('Ctrl Pts',(3.88220917950538,-1.,1.50788973857757));
#40867=CARTESIAN_POINT('Ctrl Pts',(3.88220917950538,1.,1.50788973857757));
#40868=CARTESIAN_POINT('Ctrl Pts',(3.87684006372134,-1.,1.50221016176556));
#40869=CARTESIAN_POINT('Ctrl Pts',(3.87684006372134,1.,1.50221016176556));
#40870=CARTESIAN_POINT('Ctrl Pts',(3.87145196998465,-1.,1.49656035399122));
#40871=CARTESIAN_POINT('Ctrl Pts',(3.87145196998465,1.,1.49656035399122));
#40872=CARTESIAN_POINT('Ctrl Pts',(3.86604492575189,-1.,1.4909406116431));
#40873=CARTESIAN_POINT('Ctrl Pts',(3.86604492575189,1.,1.4909406116431));
#40874=CARTESIAN_POINT('Ctrl Pts',(3.86061894706087,-1.,1.48535125509919));
#40875=CARTESIAN_POINT('Ctrl Pts',(3.86061894706087,1.,1.48535125509919));
#40876=CARTESIAN_POINT('Ctrl Pts',(3.85517401698843,-1.,1.4797926099102));
#40877=CARTESIAN_POINT('Ctrl Pts',(3.85517401698843,1.,1.4797926099102));
#40878=CARTESIAN_POINT('Ctrl Pts',(3.84971006847277,-1.,1.47426499018538));
#40879=CARTESIAN_POINT('Ctrl Pts',(3.84971006847277,1.,1.47426499018538));
#40880=CARTESIAN_POINT('Ctrl Pts',(3.84422695454796,-1.,1.46876867426504));
#40881=CARTESIAN_POINT('Ctrl Pts',(3.84422695454796,1.,1.46876867426504));
#40882=CARTESIAN_POINT('Ctrl Pts',(3.83872447159639,-1.,1.46330391180752));
#40883=CARTESIAN_POINT('Ctrl Pts',(3.83872447159639,1.,1.46330391180752));
#40884=CARTESIAN_POINT('Ctrl Pts',(3.83320241775423,-1.,1.45787095220852));
#40885=CARTESIAN_POINT('Ctrl Pts',(3.83320241775423,1.,1.45787095220852));
#40886=CARTESIAN_POINT('Ctrl Pts',(3.82766064519074,-1.,1.45247006796836));
#40887=CARTESIAN_POINT('Ctrl Pts',(3.82766064519074,1.,1.45247006796836));
#40888=CARTESIAN_POINT('Ctrl Pts',(3.82209910620533,-1.,1.44710157648539));
#40889=CARTESIAN_POINT('Ctrl Pts',(3.82209910620533,1.,1.44710157648539));
#40890=CARTESIAN_POINT('Ctrl Pts',(3.81651792398414,-1.,1.44176587041347));
#40891=CARTESIAN_POINT('Ctrl Pts',(3.81651792398414,1.,1.44176587041347));
#40892=CARTESIAN_POINT('Ctrl Pts',(3.81091737726815,-1.,1.43646341556724));
#40893=CARTESIAN_POINT('Ctrl Pts',(3.81091737726815,1.,1.43646341556724));
#40894=CARTESIAN_POINT('Ctrl Pts',(3.80529775429805,-1.,1.4311946992132));
#40895=CARTESIAN_POINT('Ctrl Pts',(3.80529775429805,1.,1.4311946992132));
#40896=CARTESIAN_POINT('Ctrl Pts',(3.7996592319632,-1.,1.42596018777283));
#40897=CARTESIAN_POINT('Ctrl Pts',(3.7996592319632,1.,1.42596018777283));
#40898=CARTESIAN_POINT('Ctrl Pts',(3.79400175744408,-1.,1.42076028482836));
#40899=CARTESIAN_POINT('Ctrl Pts',(3.79400175744408,1.,1.42076028482836));
#40900=CARTESIAN_POINT('Ctrl Pts',(3.78832489879426,-1.,1.4155952780383));
#40901=CARTESIAN_POINT('Ctrl Pts',(3.78832489879426,1.,1.4155952780383));
#40902=CARTESIAN_POINT('Ctrl Pts',(3.78262780065471,-1.,1.41046532282593));
#40903=CARTESIAN_POINT('Ctrl Pts',(3.78262780065471,1.,1.41046532282593));
#40904=CARTESIAN_POINT('Ctrl Pts',(3.77690952014259,-1.,1.40537056004722));
#40905=CARTESIAN_POINT('Ctrl Pts',(3.77690952014259,1.,1.40537056004722));
#40906=CARTESIAN_POINT('Ctrl Pts',(3.77116930621827,-1.,1.40031121335505));
#40907=CARTESIAN_POINT('Ctrl Pts',(3.77116930621827,1.,1.40031121335505));
#40908=CARTESIAN_POINT('Ctrl Pts',(3.76540689249074,-1.,1.39528769118052));
#40909=CARTESIAN_POINT('Ctrl Pts',(3.76540689249074,1.,1.39528769118052));
#40910=CARTESIAN_POINT('Ctrl Pts',(3.75962280650855,-1.,1.39030069388918));
#40911=CARTESIAN_POINT('Ctrl Pts',(3.75962280650855,1.,1.39030069388918));
#40912=CARTESIAN_POINT('Ctrl Pts',(3.75381861212707,-1.,1.38535129801176));
#40913=CARTESIAN_POINT('Ctrl Pts',(3.75381861212707,1.,1.38535129801176));
#40914=CARTESIAN_POINT('Ctrl Pts',(3.74799617204729,-1.,1.38044070763295));
#40915=CARTESIAN_POINT('Ctrl Pts',(3.74799617204729,1.,1.38044070763295));
#40916=CARTESIAN_POINT('Ctrl Pts',(3.74215698162555,-1.,1.37557002971687));
#40917=CARTESIAN_POINT('Ctrl Pts',(3.74215698162555,1.,1.37557002971687));
#40918=CARTESIAN_POINT('Ctrl Pts',(3.7363014588581,-1.,1.37074003422739));
#40919=CARTESIAN_POINT('Ctrl Pts',(3.7363014588581,1.,1.37074003422739));
#40920=CARTESIAN_POINT('Ctrl Pts',(3.73042829011295,-1.,1.36595093298676));
#40921=CARTESIAN_POINT('Ctrl Pts',(3.73042829011295,1.,1.36595093298676));
#40922=CARTESIAN_POINT('Ctrl Pts',(3.72453364678279,-1.,1.36120211416354));
#40923=CARTESIAN_POINT('Ctrl Pts',(3.72453364678279,1.,1.36120211416354));
#40924=CARTESIAN_POINT('Ctrl Pts',(3.71861271513313,-1.,1.35649266705037));
#40925=CARTESIAN_POINT('Ctrl Pts',(3.71861271513313,1.,1.35649266705037));
#40926=CARTESIAN_POINT('Ctrl Pts',(3.71266130563054,-1.,1.35182193384424));
#40927=CARTESIAN_POINT('Ctrl Pts',(3.71266130563054,1.,1.35182193384424));
#40928=CARTESIAN_POINT('Ctrl Pts',(3.70667753188248,-1.,1.34719008463534));
#40929=CARTESIAN_POINT('Ctrl Pts',(3.70667753188248,1.,1.34719008463534));
#40930=CARTESIAN_POINT('Ctrl Pts',(3.70066324015119,-1.,1.34259860752933));
#40931=CARTESIAN_POINT('Ctrl Pts',(3.70066324015119,1.,1.34259860752933));
#40932=CARTESIAN_POINT('Ctrl Pts',(3.69462613305708,-1.,1.3380510339822));
#40933=CARTESIAN_POINT('Ctrl Pts',(3.69462613305708,1.,1.3380510339822));
#40934=CARTESIAN_POINT('Ctrl Pts',(3.68857672413033,-1.,1.33355191034523));
#40935=CARTESIAN_POINT('Ctrl Pts',(3.68857672413033,1.,1.33355191034523));
#40936=CARTESIAN_POINT('Ctrl Pts',(3.68252441182551,-1.,1.3291054707274));
#40937=CARTESIAN_POINT('Ctrl Pts',(3.68252441182551,1.,1.3291054707274));
#40938=CARTESIAN_POINT('Ctrl Pts',(3.67647355257912,-1.,1.32471430856415));
#40939=CARTESIAN_POINT('Ctrl Pts',(3.67647355257912,1.,1.32471430856415));
#40940=CARTESIAN_POINT('Ctrl Pts',(3.67042021752656,-1.,1.32037828137766));
#40941=CARTESIAN_POINT('Ctrl Pts',(3.67042021752656,1.,1.32037828137766));
#40942=CARTESIAN_POINT('Ctrl Pts',(3.66434688899793,-1.,1.31609271239911));
#40943=CARTESIAN_POINT('Ctrl Pts',(3.66434688899793,1.,1.31609271239911));
#40944=CARTESIAN_POINT('Ctrl Pts',(3.65822827358617,-1.,1.31185038411218));
#40945=CARTESIAN_POINT('Ctrl Pts',(3.65822827358617,1.,1.31185038411218));
#40946=CARTESIAN_POINT('Ctrl Pts',(3.65204081987068,-1.,1.30764479590039));
#40947=CARTESIAN_POINT('Ctrl Pts',(3.65204081987068,1.,1.30764479590039));
#40948=CARTESIAN_POINT('Ctrl Pts',(3.64577181380113,-1.,1.30347327603774));
#40949=CARTESIAN_POINT('Ctrl Pts',(3.64577181380113,1.,1.30347327603774));
#40950=CARTESIAN_POINT('Ctrl Pts',(3.63942689872808,-1.,1.2993395590647));
#40951=CARTESIAN_POINT('Ctrl Pts',(3.63942689872808,1.,1.2993395590647));
#40952=CARTESIAN_POINT('Ctrl Pts',(3.63304271631046,-1.,1.29525810207762));
#40953=CARTESIAN_POINT('Ctrl Pts',(3.63304271631046,1.,1.29525810207762));
#40954=CARTESIAN_POINT('Ctrl Pts',(3.62667616004369,-1.,1.29125046021878));
#40955=CARTESIAN_POINT('Ctrl Pts',(3.62667616004369,1.,1.29125046021878));
#40956=CARTESIAN_POINT('Ctrl Pts',(3.6203814849236,-1.,1.28733755029384));
#40957=CARTESIAN_POINT('Ctrl Pts',(3.6203814849236,1.,1.28733755029384));
#40958=CARTESIAN_POINT('Ctrl Pts',(3.61418935913823,-1.,1.28353255117765));
#40959=CARTESIAN_POINT('Ctrl Pts',(3.61418935913823,1.,1.28353255117765));
#40960=CARTESIAN_POINT('Ctrl Pts',(3.60808907746339,-1.,1.27983492861691));
#40961=CARTESIAN_POINT('Ctrl Pts',(3.60808907746339,1.,1.27983492861691));
#40962=CARTESIAN_POINT('Ctrl Pts',(3.60199947736298,-1.,1.27622049908625));
#40963=CARTESIAN_POINT('Ctrl Pts',(3.60199947736298,1.,1.27622049908625));
#40964=CARTESIAN_POINT('Ctrl Pts',(3.59578698050006,-1.,1.27264798379307));
#40965=CARTESIAN_POINT('Ctrl Pts',(3.59578698050006,1.,1.27264798379307));
#40966=CARTESIAN_POINT('Ctrl Pts',(3.58931807846313,-1.,1.26907758484709));
#40967=CARTESIAN_POINT('Ctrl Pts',(3.58931807846313,1.,1.26907758484709));
#40968=CARTESIAN_POINT('Ctrl Pts',(3.58250452868618,-1.,1.26548706249862));
#40969=CARTESIAN_POINT('Ctrl Pts',(3.58250452868618,1.,1.26548706249862));
#40970=CARTESIAN_POINT('Ctrl Pts',(3.5753456065171,-1.,1.2618866714281));
#40971=CARTESIAN_POINT('Ctrl Pts',(3.5753456065171,1.,1.2618866714281));
#40972=CARTESIAN_POINT('Ctrl Pts',(3.56798645995275,-1.,1.25834000485716));
#40973=CARTESIAN_POINT('Ctrl Pts',(3.56798645995275,1.,1.25834000485716));
#40974=CARTESIAN_POINT('Ctrl Pts',(3.56071094991199,-1.,1.25496090900009));
#40975=CARTESIAN_POINT('Ctrl Pts',(3.56071094991199,1.,1.25496090900009));
#40976=CARTESIAN_POINT('Ctrl Pts',(3.55387287418985,-1.,1.2518879294064));
#40977=CARTESIAN_POINT('Ctrl Pts',(3.55387287418985,1.,1.2518879294064));
#40978=CARTESIAN_POINT('Ctrl Pts',(3.54784190283068,-1.,1.24926408628003));
#40979=CARTESIAN_POINT('Ctrl Pts',(3.54784190283068,1.,1.24926408628003));
#40980=CARTESIAN_POINT('Ctrl Pts',(3.54294877425964,-1.,1.24721646231966));
#40981=CARTESIAN_POINT('Ctrl Pts',(3.54294877425964,1.,1.24721646231966));
#40982=CARTESIAN_POINT('Ctrl Pts',(3.53941798195825,-1.,1.24583101679029));
#40983=CARTESIAN_POINT('Ctrl Pts',(3.53941798195825,1.,1.24583101679029));
#40984=CARTESIAN_POINT('Ctrl Pts',(3.53776753802906,-1.,1.24528461332987));
#40985=CARTESIAN_POINT('Ctrl Pts',(3.53776753802906,1.,1.24528461332987));
#40986=CARTESIAN_POINT('Ctrl Pts',(3.53720633057798,-1.,1.24519702335451));
#40987=CARTESIAN_POINT('Ctrl Pts',(3.53720633057798,1.,1.24519702335451));
#40988=CARTESIAN_POINT('Ctrl Pts',(3.53713269667399,-1.,1.24528174185098));
#40989=CARTESIAN_POINT('Ctrl Pts',(3.53713269667399,1.,1.24528174185098));
#40990=CARTESIAN_POINT('Ctrl Pts',(3.53717101171257,-1.,1.24535988127942));
#40991=CARTESIAN_POINT('Ctrl Pts',(3.53717101171257,1.,1.24535988127942));
#40992=CARTESIAN_POINT('',(3.90876544355381,1.,1.53673442965256));
#40993=CARTESIAN_POINT('Ctrl Pts',(3.90876544355381,1.,1.53673442965256));
#40994=CARTESIAN_POINT('Ctrl Pts',(3.90771246855019,1.,1.53556639217905));
#40995=CARTESIAN_POINT('Ctrl Pts',(3.90560462813969,1.,1.53323321827755));
#40996=CARTESIAN_POINT('Ctrl Pts',(3.90243719631596,1.,1.52974216056287));
#40997=CARTESIAN_POINT('Ctrl Pts',(3.89820260708225,1.,1.52510482991635));
#40998=CARTESIAN_POINT('Ctrl Pts',(3.89289043533657,1.,1.51933724329306));
#40999=CARTESIAN_POINT('Ctrl Pts',(3.88755930033884,1.,1.51359883110559));
#41000=CARTESIAN_POINT('Ctrl Pts',(3.88220917950538,1.,1.50788973857757));
#41001=CARTESIAN_POINT('Ctrl Pts',(3.87684006372134,1.,1.50221016176556));
#41002=CARTESIAN_POINT('Ctrl Pts',(3.87145196998465,1.,1.49656035399122));
#41003=CARTESIAN_POINT('Ctrl Pts',(3.86604492575189,1.,1.4909406116431));
#41004=CARTESIAN_POINT('Ctrl Pts',(3.86061894706087,1.,1.48535125509919));
#41005=CARTESIAN_POINT('Ctrl Pts',(3.85517401698843,1.,1.4797926099102));
#41006=CARTESIAN_POINT('Ctrl Pts',(3.84971006847277,1.,1.47426499018538));
#41007=CARTESIAN_POINT('Ctrl Pts',(3.84422695454796,1.,1.46876867426504));
#41008=CARTESIAN_POINT('Ctrl Pts',(3.83872447159639,1.,1.46330391180752));
#41009=CARTESIAN_POINT('Ctrl Pts',(3.83320241775423,1.,1.45787095220852));
#41010=CARTESIAN_POINT('Ctrl Pts',(3.82766064519074,1.,1.45247006796836));
#41011=CARTESIAN_POINT('Ctrl Pts',(3.82209910620533,1.,1.44710157648539));
#41012=CARTESIAN_POINT('Ctrl Pts',(3.81651792398414,1.,1.44176587041347));
#41013=CARTESIAN_POINT('Ctrl Pts',(3.81091737726815,1.,1.43646341556724));
#41014=CARTESIAN_POINT('Ctrl Pts',(3.80529775429805,1.,1.4311946992132));
#41015=CARTESIAN_POINT('Ctrl Pts',(3.7996592319632,1.,1.42596018777283));
#41016=CARTESIAN_POINT('Ctrl Pts',(3.79400175744408,1.,1.42076028482836));
#41017=CARTESIAN_POINT('Ctrl Pts',(3.78832489879426,1.,1.4155952780383));
#41018=CARTESIAN_POINT('Ctrl Pts',(3.78262780065471,1.,1.41046532282593));
#41019=CARTESIAN_POINT('Ctrl Pts',(3.77690952014259,1.,1.40537056004722));
#41020=CARTESIAN_POINT('Ctrl Pts',(3.77116930621827,1.,1.40031121335505));
#41021=CARTESIAN_POINT('Ctrl Pts',(3.76540689249074,1.,1.39528769118052));
#41022=CARTESIAN_POINT('Ctrl Pts',(3.75962280650855,1.,1.39030069388918));
#41023=CARTESIAN_POINT('Ctrl Pts',(3.75381861212707,1.,1.38535129801176));
#41024=CARTESIAN_POINT('Ctrl Pts',(3.74799617204729,1.,1.38044070763295));
#41025=CARTESIAN_POINT('Ctrl Pts',(3.74215698162555,1.,1.37557002971687));
#41026=CARTESIAN_POINT('Ctrl Pts',(3.7363014588581,1.,1.37074003422739));
#41027=CARTESIAN_POINT('Ctrl Pts',(3.73042829011295,1.,1.36595093298676));
#41028=CARTESIAN_POINT('Ctrl Pts',(3.72453364678279,1.,1.36120211416354));
#41029=CARTESIAN_POINT('Ctrl Pts',(3.71861271513313,1.,1.35649266705037));
#41030=CARTESIAN_POINT('Ctrl Pts',(3.71266130563054,1.,1.35182193384424));
#41031=CARTESIAN_POINT('Ctrl Pts',(3.70667753188248,1.,1.34719008463534));
#41032=CARTESIAN_POINT('Ctrl Pts',(3.70066324015119,1.,1.34259860752933));
#41033=CARTESIAN_POINT('Ctrl Pts',(3.69462613305708,1.,1.3380510339822));
#41034=CARTESIAN_POINT('Ctrl Pts',(3.68857672413033,1.,1.33355191034523));
#41035=CARTESIAN_POINT('Ctrl Pts',(3.68252441182551,1.,1.3291054707274));
#41036=CARTESIAN_POINT('Ctrl Pts',(3.67647355257912,1.,1.32471430856415));
#41037=CARTESIAN_POINT('Ctrl Pts',(3.67042021752656,1.,1.32037828137766));
#41038=CARTESIAN_POINT('Ctrl Pts',(3.66434688899793,1.,1.31609271239911));
#41039=CARTESIAN_POINT('Ctrl Pts',(3.65822827358617,1.,1.31185038411218));
#41040=CARTESIAN_POINT('Ctrl Pts',(3.65204081987068,1.,1.30764479590039));
#41041=CARTESIAN_POINT('Ctrl Pts',(3.64577181380113,1.,1.30347327603774));
#41042=CARTESIAN_POINT('Ctrl Pts',(3.63942689872808,1.,1.2993395590647));
#41043=CARTESIAN_POINT('Ctrl Pts',(3.63304271631046,1.,1.29525810207762));
#41044=CARTESIAN_POINT('Ctrl Pts',(3.62667616004369,1.,1.29125046021878));
#41045=CARTESIAN_POINT('Ctrl Pts',(3.6203814849236,1.,1.28733755029384));
#41046=CARTESIAN_POINT('Ctrl Pts',(3.61418935913823,1.,1.28353255117765));
#41047=CARTESIAN_POINT('Ctrl Pts',(3.60808907746339,1.,1.27983492861691));
#41048=CARTESIAN_POINT('Ctrl Pts',(3.60199947736298,1.,1.27622049908625));
#41049=CARTESIAN_POINT('Ctrl Pts',(3.59578698050006,1.,1.27264798379307));
#41050=CARTESIAN_POINT('Ctrl Pts',(3.58931807846313,1.,1.26907758484709));
#41051=CARTESIAN_POINT('Ctrl Pts',(3.58250452868618,1.,1.26548706249862));
#41052=CARTESIAN_POINT('Ctrl Pts',(3.5753456065171,1.,1.2618866714281));
#41053=CARTESIAN_POINT('Ctrl Pts',(3.56798645995275,1.,1.25834000485716));
#41054=CARTESIAN_POINT('Ctrl Pts',(3.56071094991199,1.,1.25496090900009));
#41055=CARTESIAN_POINT('Ctrl Pts',(3.55387287418985,1.,1.2518879294064));
#41056=CARTESIAN_POINT('Ctrl Pts',(3.54784190283068,1.,1.24926408628003));
#41057=CARTESIAN_POINT('Ctrl Pts',(3.54294877425964,1.,1.24721646231966));
#41058=CARTESIAN_POINT('Ctrl Pts',(3.53968291130022,1.,1.24593497226008));
#41059=CARTESIAN_POINT('Ctrl Pts',(3.53808746578196,1.,1.24539205388767));
#41060=CARTESIAN_POINT('Ctrl Pts',(3.5374485926552,1.,1.2452449899111));
#41061=CARTESIAN_POINT('Ctrl Pts',(3.53725139174486,1.,1.24524838931757));
#41062=CARTESIAN_POINT('Ctrl Pts',(3.5372048861597,1.,1.24526366418038));
#41063=CARTESIAN_POINT('',(3.90876544355381,0.,1.53673442965256));
#41064=CARTESIAN_POINT('Ctrl Pts',(3.38176002566879,-1.,1.62055519152809));
#41065=CARTESIAN_POINT('Ctrl Pts',(3.38176002566879,1.,1.62055519152809));
#41066=CARTESIAN_POINT('Ctrl Pts',(3.38167767992676,-1.,1.62058335162482));
#41067=CARTESIAN_POINT('Ctrl Pts',(3.38167767992676,1.,1.62058335162482));
#41068=CARTESIAN_POINT('Ctrl Pts',(3.38166984193836,-1.,1.62069532368199));
#41069=CARTESIAN_POINT('Ctrl Pts',(3.38166984193836,1.,1.62069532368199));
#41070=CARTESIAN_POINT('Ctrl Pts',(3.38212861099983,-1.,1.62103022181151));
#41071=CARTESIAN_POINT('Ctrl Pts',(3.38212861099983,1.,1.62103022181151));
#41072=CARTESIAN_POINT('Ctrl Pts',(3.38368201668574,-1.,1.62181089631344));
#41073=CARTESIAN_POINT('Ctrl Pts',(3.38368201668574,1.,1.62181089631344));
#41074=CARTESIAN_POINT('Ctrl Pts',(3.38715832179072,-1.,1.6233278855625));
#41075=CARTESIAN_POINT('Ctrl Pts',(3.38715832179072,1.,1.6233278855625));
#41076=CARTESIAN_POINT('Ctrl Pts',(3.39206617496906,-1.,1.62533996116713));
#41077=CARTESIAN_POINT('Ctrl Pts',(3.39206617496906,1.,1.62533996116713));
#41078=CARTESIAN_POINT('Ctrl Pts',(3.39818605297991,-1.,1.62774916464408));
#41079=CARTESIAN_POINT('Ctrl Pts',(3.39818605297991,1.,1.62774916464408));
#41080=CARTESIAN_POINT('Ctrl Pts',(3.40519422740235,-1.,1.63041148964828));
#41081=CARTESIAN_POINT('Ctrl Pts',(3.40519422740235,1.,1.63041148964828));
#41082=CARTESIAN_POINT('Ctrl Pts',(3.41272817148478,-1.,1.63316667054044));
#41083=CARTESIAN_POINT('Ctrl Pts',(3.41272817148478,1.,1.63316667054044));
#41084=CARTESIAN_POINT('Ctrl Pts',(3.42043974590882,-1.,1.63586250099773));
#41085=CARTESIAN_POINT('Ctrl Pts',(3.42043974590882,1.,1.63586250099773));
#41086=CARTESIAN_POINT('Ctrl Pts',(3.42804772926291,-1.,1.63837876246926));
#41087=CARTESIAN_POINT('Ctrl Pts',(3.42804772926291,1.,1.63837876246926));
#41088=CARTESIAN_POINT('Ctrl Pts',(3.43540451921548,-1.,1.64065778702023));
#41089=CARTESIAN_POINT('Ctrl Pts',(3.43540451921548,1.,1.64065778702023));
#41090=CARTESIAN_POINT('Ctrl Pts',(3.44250337701888,-1.,1.64270733821113));
#41091=CARTESIAN_POINT('Ctrl Pts',(3.44250337701888,1.,1.64270733821113));
#41092=CARTESIAN_POINT('Ctrl Pts',(3.44942242546795,-1.,1.64457408708107));
#41093=CARTESIAN_POINT('Ctrl Pts',(3.44942242546795,1.,1.64457408708107));
#41094=CARTESIAN_POINT('Ctrl Pts',(3.45628421062422,-1.,1.64632429697521));
#41095=CARTESIAN_POINT('Ctrl Pts',(3.45628421062422,1.,1.64632429697521));
#41096=CARTESIAN_POINT('Ctrl Pts',(3.46321237515,-1.,1.64802323352738));
#41097=CARTESIAN_POINT('Ctrl Pts',(3.46321237515,1.,1.64802323352738));
#41098=CARTESIAN_POINT('Ctrl Pts',(3.47028140995992,-1.,1.64971118698256));
#41099=CARTESIAN_POINT('Ctrl Pts',(3.47028140995992,1.,1.64971118698256));
#41100=CARTESIAN_POINT('Ctrl Pts',(3.47749926256476,-1.,1.65139534930322));
#41101=CARTESIAN_POINT('Ctrl Pts',(3.47749926256476,1.,1.65139534930322));
#41102=CARTESIAN_POINT('Ctrl Pts',(3.48483492840894,-1.,1.65306335367739));
#41103=CARTESIAN_POINT('Ctrl Pts',(3.48483492840894,1.,1.65306335367739));
#41104=CARTESIAN_POINT('Ctrl Pts',(3.49223525300176,-1.,1.65469162644468));
#41105=CARTESIAN_POINT('Ctrl Pts',(3.49223525300176,1.,1.65469162644468));
#41106=CARTESIAN_POINT('Ctrl Pts',(3.4996447647794,-1.,1.65625517961588));
#41107=CARTESIAN_POINT('Ctrl Pts',(3.4996447647794,1.,1.65625517961588));
#41108=CARTESIAN_POINT('Ctrl Pts',(3.50702733146542,-1.,1.65773832633632));
#41109=CARTESIAN_POINT('Ctrl Pts',(3.50702733146542,1.,1.65773832633632));
#41110=CARTESIAN_POINT('Ctrl Pts',(3.5143763218894,-1.,1.65913971687342));
#41111=CARTESIAN_POINT('Ctrl Pts',(3.5143763218894,1.,1.65913971687342));
#41112=CARTESIAN_POINT('Ctrl Pts',(3.52170261543815,-1.,1.66046645222279));
#41113=CARTESIAN_POINT('Ctrl Pts',(3.52170261543815,1.,1.66046645222279));
#41114=CARTESIAN_POINT('Ctrl Pts',(3.52902746211093,-1.,1.66173058912371));
#41115=CARTESIAN_POINT('Ctrl Pts',(3.52902746211093,1.,1.66173058912371));
#41116=CARTESIAN_POINT('Ctrl Pts',(3.5363738506022,-1.,1.66294490916111));
#41117=CARTESIAN_POINT('Ctrl Pts',(3.5363738506022,1.,1.66294490916111));
#41118=CARTESIAN_POINT('Ctrl Pts',(3.54375747475014,-1.,1.66411849222326));
#41119=CARTESIAN_POINT('Ctrl Pts',(3.54375747475014,1.,1.66411849222326));
#41120=CARTESIAN_POINT('Ctrl Pts',(3.55118121342861,-1.,1.66525401568994));
#41121=CARTESIAN_POINT('Ctrl Pts',(3.55118121342861,1.,1.66525401568994));
#41122=CARTESIAN_POINT('Ctrl Pts',(3.55864015233602,-1.,1.66635023293114));
#41123=CARTESIAN_POINT('Ctrl Pts',(3.55864015233602,1.,1.66635023293114));
#41124=CARTESIAN_POINT('Ctrl Pts',(3.56612465179422,-1.,1.66740349220305));
#41125=CARTESIAN_POINT('Ctrl Pts',(3.56612465179422,1.,1.66740349220305));
#41126=CARTESIAN_POINT('Ctrl Pts',(3.57362406285887,-1.,1.668409574073));
#41127=CARTESIAN_POINT('Ctrl Pts',(3.57362406285887,1.,1.668409574073));
#41128=CARTESIAN_POINT('Ctrl Pts',(3.58113044183829,-1.,1.66936552908232));
#41129=CARTESIAN_POINT('Ctrl Pts',(3.58113044183829,1.,1.66936552908232));
#41130=CARTESIAN_POINT('Ctrl Pts',(3.58864143097834,-1.,1.67027110397604));
#41131=CARTESIAN_POINT('Ctrl Pts',(3.58864143097834,1.,1.67027110397604));
#41132=CARTESIAN_POINT('Ctrl Pts',(3.59615824388807,-1.,1.67112775290707));
#41133=CARTESIAN_POINT('Ctrl Pts',(3.59615824388807,1.,1.67112775290707));
#41134=CARTESIAN_POINT('Ctrl Pts',(3.603684308152,-1.,1.67193797318597));
#41135=CARTESIAN_POINT('Ctrl Pts',(3.603684308152,1.,1.67193797318597));
#41136=CARTESIAN_POINT('Ctrl Pts',(3.61122367156181,-1.,1.67270452466968));
#41137=CARTESIAN_POINT('Ctrl Pts',(3.61122367156181,1.,1.67270452466968));
#41138=CARTESIAN_POINT('Ctrl Pts',(3.61877947398184,-1.,1.67342968196224));
#41139=CARTESIAN_POINT('Ctrl Pts',(3.61877947398184,1.,1.67342968196224));
#41140=CARTESIAN_POINT('Ctrl Pts',(3.62635249450923,-1.,1.67411452372271));
#41141=CARTESIAN_POINT('Ctrl Pts',(3.62635249450923,1.,1.67411452372271));
#41142=CARTESIAN_POINT('Ctrl Pts',(3.63394189312924,-1.,1.67475929882971));
#41143=CARTESIAN_POINT('Ctrl Pts',(3.63394189312924,1.,1.67475929882971));
#41144=CARTESIAN_POINT('Ctrl Pts',(3.6415458297234,-1.,1.67536373264848));
#41145=CARTESIAN_POINT('Ctrl Pts',(3.6415458297234,1.,1.67536373264848));
#41146=CARTESIAN_POINT('Ctrl Pts',(3.64916213574667,-1.,1.67592735946692));
#41147=CARTESIAN_POINT('Ctrl Pts',(3.64916213574667,1.,1.67592735946692));
#41148=CARTESIAN_POINT('Ctrl Pts',(3.6567889441642,-1.,1.6764498346945));
#41149=CARTESIAN_POINT('Ctrl Pts',(3.6567889441642,1.,1.6764498346945));
#41150=CARTESIAN_POINT('Ctrl Pts',(3.66442538670968,-1.,1.67693128053132));
#41151=CARTESIAN_POINT('Ctrl Pts',(3.66442538670968,1.,1.67693128053132));
#41152=CARTESIAN_POINT('Ctrl Pts',(3.67207136294575,-1.,1.67737217414874));
#41153=CARTESIAN_POINT('Ctrl Pts',(3.67207136294575,1.,1.67737217414874));
#41154=CARTESIAN_POINT('Ctrl Pts',(3.67972724579124,-1.,1.67777320475848));
#41155=CARTESIAN_POINT('Ctrl Pts',(3.67972724579124,1.,1.67777320475848));
#41156=CARTESIAN_POINT('Ctrl Pts',(3.68739360236487,-1.,1.67813513867965));
#41157=CARTESIAN_POINT('Ctrl Pts',(3.68739360236487,1.,1.67813513867965));
#41158=CARTESIAN_POINT('Ctrl Pts',(3.6950709275959,-1.,1.67845869064323));
#41159=CARTESIAN_POINT('Ctrl Pts',(3.6950709275959,1.,1.67845869064323));
#41160=CARTESIAN_POINT('Ctrl Pts',(3.70275932351108,-1.,1.67874436948667));
#41161=CARTESIAN_POINT('Ctrl Pts',(3.70275932351108,1.,1.67874436948667));
#41162=CARTESIAN_POINT('Ctrl Pts',(3.71045854208343,-1.,1.67899249793462));
#41163=CARTESIAN_POINT('Ctrl Pts',(3.71045854208343,1.,1.67899249793462));
#41164=CARTESIAN_POINT('Ctrl Pts',(3.71816812842322,-1.,1.67920328071708));
#41165=CARTESIAN_POINT('Ctrl Pts',(3.71816812842322,1.,1.67920328071708));
#41166=CARTESIAN_POINT('Ctrl Pts',(3.72588753416396,-1.,1.67937685856652));
#41167=CARTESIAN_POINT('Ctrl Pts',(3.72588753416396,1.,1.67937685856652));
#41168=CARTESIAN_POINT('Ctrl Pts',(3.73361623282543,-1.,1.67951336376402));
#41169=CARTESIAN_POINT('Ctrl Pts',(3.73361623282543,1.,1.67951336376402));
#41170=CARTESIAN_POINT('Ctrl Pts',(3.74135385965401,-1.,1.6796129868522));
#41171=CARTESIAN_POINT('Ctrl Pts',(3.74135385965401,1.,1.6796129868522));
#41172=CARTESIAN_POINT('Ctrl Pts',(3.7491002239452,-1.,1.67967598599525));
#41173=CARTESIAN_POINT('Ctrl Pts',(3.7491002239452,1.,1.67967598599525));
#41174=CARTESIAN_POINT('Ctrl Pts',(3.75685523754493,-1.,1.67970265841239));
#41175=CARTESIAN_POINT('Ctrl Pts',(3.75685523754493,1.,1.67970265841239));
#41176=CARTESIAN_POINT('Ctrl Pts',(3.76461886684344,-1.,1.67969332319245));
#41177=CARTESIAN_POINT('Ctrl Pts',(3.76461886684344,1.,1.67969332319245));
#41178=CARTESIAN_POINT('Ctrl Pts',(3.77239107928502,-1.,1.67964830084993));
#41179=CARTESIAN_POINT('Ctrl Pts',(3.77239107928502,1.,1.67964830084993));
#41180=CARTESIAN_POINT('Ctrl Pts',(3.78017178197317,-1.,1.67956789212141));
#41181=CARTESIAN_POINT('Ctrl Pts',(3.78017178197317,1.,1.67956789212141));
#41182=CARTESIAN_POINT('Ctrl Pts',(3.7879608002176,-1.,1.67945236653493));
#41183=CARTESIAN_POINT('Ctrl Pts',(3.7879608002176,1.,1.67945236653493));
#41184=CARTESIAN_POINT('Ctrl Pts',(3.79575791578424,-1.,1.67930196625548));
#41185=CARTESIAN_POINT('Ctrl Pts',(3.79575791578424,1.,1.67930196625548));
#41186=CARTESIAN_POINT('Ctrl Pts',(3.80356289079005,-1.,1.67911690648355));
#41187=CARTESIAN_POINT('Ctrl Pts',(3.80356289079005,1.,1.67911690648355));
#41188=CARTESIAN_POINT('Ctrl Pts',(3.81137549624178,-1.,1.6788973773827));
#41189=CARTESIAN_POINT('Ctrl Pts',(3.81137549624178,1.,1.6788973773827));
#41190=CARTESIAN_POINT('Ctrl Pts',(3.81919554099578,-1.,1.67864354605954));
#41191=CARTESIAN_POINT('Ctrl Pts',(3.81919554099578,1.,1.67864354605954));
#41192=CARTESIAN_POINT('Ctrl Pts',(3.82702289286713,-1.,1.6783555575934));
#41193=CARTESIAN_POINT('Ctrl Pts',(3.82702289286713,1.,1.6783555575934));
#41194=CARTESIAN_POINT('Ctrl Pts',(3.83485746513989,-1.,1.67803353064351));
#41195=CARTESIAN_POINT('Ctrl Pts',(3.83485746513989,1.,1.67803353064351));
#41196=CARTESIAN_POINT('Ctrl Pts',(3.84113085985244,-1.,1.67774874946079));
#41197=CARTESIAN_POINT('Ctrl Pts',(3.84113085985244,1.,1.67774874946079));
#41198=CARTESIAN_POINT('Ctrl Pts',(3.84583912296459,-1.,1.6775199114018));
#41199=CARTESIAN_POINT('Ctrl Pts',(3.84583912296459,1.,1.6775199114018));
#41200=CARTESIAN_POINT('Ctrl Pts',(3.84897939430696,-1.,1.67736057656533));
#41201=CARTESIAN_POINT('Ctrl Pts',(3.84897939430696,1.,1.67736057656533));
#41202=CARTESIAN_POINT('Ctrl Pts',(3.85054988729471,-1.,1.67727921511438));
#41203=CARTESIAN_POINT('Ctrl Pts',(3.85054988729471,1.,1.67727921511438));
#41204=CARTESIAN_POINT('',(3.38171594275765,1.,1.62064718014094));
#41205=CARTESIAN_POINT('Ctrl Pts',(3.38171594275765,-1.,1.62064718014094));
#41206=CARTESIAN_POINT('Ctrl Pts',(3.38171594275765,-0.666666666666667,
1.62064718014094));
#41207=CARTESIAN_POINT('Ctrl Pts',(3.38171594275765,-0.333333333333333,
1.62064718014094));
#41208=CARTESIAN_POINT('Ctrl Pts',(3.38171594275765,0.333333333333333,1.62064718014094));
#41209=CARTESIAN_POINT('Ctrl Pts',(3.38171594275765,0.666666666666667,1.62064718014093));
#41210=CARTESIAN_POINT('Ctrl Pts',(3.38171594275765,1.,1.62064718014093));
#41211=CARTESIAN_POINT('',(3.85054988729471,1.,1.67727921511438));
#41212=CARTESIAN_POINT('',(3.85054988729471,0.,1.67727921511438));
#41213=CARTESIAN_POINT('Ctrl Pts',(3.38171594275765,1.,1.62064718014094));
#41214=CARTESIAN_POINT('Ctrl Pts',(3.38173802621259,1.,1.62069086551492));
#41215=CARTESIAN_POINT('Ctrl Pts',(3.38187506456922,1.,1.62083271135947));
#41216=CARTESIAN_POINT('Ctrl Pts',(3.38243080602408,1.,1.62118047294498));
#41217=CARTESIAN_POINT('Ctrl Pts',(3.38394285763222,1.,1.62192472202769));
#41218=CARTESIAN_POINT('Ctrl Pts',(3.38715832179072,1.,1.6233278855625));
#41219=CARTESIAN_POINT('Ctrl Pts',(3.39206617496906,1.,1.62533996116713));
#41220=CARTESIAN_POINT('Ctrl Pts',(3.39818605297991,1.,1.62774916464408));
#41221=CARTESIAN_POINT('Ctrl Pts',(3.40519422740235,1.,1.63041148964828));
#41222=CARTESIAN_POINT('Ctrl Pts',(3.41272817148478,1.,1.63316667054044));
#41223=CARTESIAN_POINT('Ctrl Pts',(3.42043974590882,1.,1.63586250099773));
#41224=CARTESIAN_POINT('Ctrl Pts',(3.42804772926291,1.,1.63837876246926));
#41225=CARTESIAN_POINT('Ctrl Pts',(3.43540451921548,1.,1.64065778702023));
#41226=CARTESIAN_POINT('Ctrl Pts',(3.44250337701888,1.,1.64270733821113));
#41227=CARTESIAN_POINT('Ctrl Pts',(3.44942242546795,1.,1.64457408708107));
#41228=CARTESIAN_POINT('Ctrl Pts',(3.45628421062422,1.,1.64632429697521));
#41229=CARTESIAN_POINT('Ctrl Pts',(3.46321237515,1.,1.64802323352738));
#41230=CARTESIAN_POINT('Ctrl Pts',(3.47028140995992,1.,1.64971118698256));
#41231=CARTESIAN_POINT('Ctrl Pts',(3.47749926256476,1.,1.65139534930322));
#41232=CARTESIAN_POINT('Ctrl Pts',(3.48483492840894,1.,1.65306335367739));
#41233=CARTESIAN_POINT('Ctrl Pts',(3.49223525300176,1.,1.65469162644468));
#41234=CARTESIAN_POINT('Ctrl Pts',(3.4996447647794,1.,1.65625517961588));
#41235=CARTESIAN_POINT('Ctrl Pts',(3.50702733146542,1.,1.65773832633632));
#41236=CARTESIAN_POINT('Ctrl Pts',(3.5143763218894,1.,1.65913971687342));
#41237=CARTESIAN_POINT('Ctrl Pts',(3.52170261543815,1.,1.66046645222279));
#41238=CARTESIAN_POINT('Ctrl Pts',(3.52902746211093,1.,1.66173058912371));
#41239=CARTESIAN_POINT('Ctrl Pts',(3.5363738506022,1.,1.66294490916111));
#41240=CARTESIAN_POINT('Ctrl Pts',(3.54375747475014,1.,1.66411849222326));
#41241=CARTESIAN_POINT('Ctrl Pts',(3.55118121342861,1.,1.66525401568994));
#41242=CARTESIAN_POINT('Ctrl Pts',(3.55864015233602,1.,1.66635023293114));
#41243=CARTESIAN_POINT('Ctrl Pts',(3.56612465179422,1.,1.66740349220305));
#41244=CARTESIAN_POINT('Ctrl Pts',(3.57362406285887,1.,1.668409574073));
#41245=CARTESIAN_POINT('Ctrl Pts',(3.58113044183829,1.,1.66936552908232));
#41246=CARTESIAN_POINT('Ctrl Pts',(3.58864143097834,1.,1.67027110397604));
#41247=CARTESIAN_POINT('Ctrl Pts',(3.59615824388807,1.,1.67112775290707));
#41248=CARTESIAN_POINT('Ctrl Pts',(3.603684308152,1.,1.67193797318597));
#41249=CARTESIAN_POINT('Ctrl Pts',(3.61122367156181,1.,1.67270452466968));
#41250=CARTESIAN_POINT('Ctrl Pts',(3.61877947398184,1.,1.67342968196224));
#41251=CARTESIAN_POINT('Ctrl Pts',(3.62635249450923,1.,1.67411452372271));
#41252=CARTESIAN_POINT('Ctrl Pts',(3.63394189312924,1.,1.67475929882971));
#41253=CARTESIAN_POINT('Ctrl Pts',(3.6415458297234,1.,1.67536373264848));
#41254=CARTESIAN_POINT('Ctrl Pts',(3.64916213574667,1.,1.67592735946692));
#41255=CARTESIAN_POINT('Ctrl Pts',(3.6567889441642,1.,1.6764498346945));
#41256=CARTESIAN_POINT('Ctrl Pts',(3.66442538670968,1.,1.67693128053132));
#41257=CARTESIAN_POINT('Ctrl Pts',(3.67207136294575,1.,1.67737217414874));
#41258=CARTESIAN_POINT('Ctrl Pts',(3.67972724579124,1.,1.67777320475848));
#41259=CARTESIAN_POINT('Ctrl Pts',(3.68739360236487,1.,1.67813513867965));
#41260=CARTESIAN_POINT('Ctrl Pts',(3.6950709275959,1.,1.67845869064323));
#41261=CARTESIAN_POINT('Ctrl Pts',(3.70275932351108,1.,1.67874436948667));
#41262=CARTESIAN_POINT('Ctrl Pts',(3.71045854208343,1.,1.67899249793462));
#41263=CARTESIAN_POINT('Ctrl Pts',(3.71816812842322,1.,1.67920328071708));
#41264=CARTESIAN_POINT('Ctrl Pts',(3.72588753416396,1.,1.67937685856652));
#41265=CARTESIAN_POINT('Ctrl Pts',(3.73361623282543,1.,1.67951336376402));
#41266=CARTESIAN_POINT('Ctrl Pts',(3.74135385965401,1.,1.6796129868522));
#41267=CARTESIAN_POINT('Ctrl Pts',(3.7491002239452,1.,1.67967598599525));
#41268=CARTESIAN_POINT('Ctrl Pts',(3.75685523754493,1.,1.67970265841239));
#41269=CARTESIAN_POINT('Ctrl Pts',(3.76461886684344,1.,1.67969332319245));
#41270=CARTESIAN_POINT('Ctrl Pts',(3.77239107928502,1.,1.67964830084993));
#41271=CARTESIAN_POINT('Ctrl Pts',(3.78017178197317,1.,1.67956789212141));
#41272=CARTESIAN_POINT('Ctrl Pts',(3.7879608002176,1.,1.67945236653493));
#41273=CARTESIAN_POINT('Ctrl Pts',(3.79575791578424,1.,1.67930196625548));
#41274=CARTESIAN_POINT('Ctrl Pts',(3.80356289079005,1.,1.67911690648355));
#41275=CARTESIAN_POINT('Ctrl Pts',(3.81137549624178,1.,1.6788973773827));
#41276=CARTESIAN_POINT('Ctrl Pts',(3.81919554099578,1.,1.67864354605954));
#41277=CARTESIAN_POINT('Ctrl Pts',(3.82702289286713,1.,1.6783555575934));
#41278=CARTESIAN_POINT('Ctrl Pts',(3.83485746513989,1.,1.67803353064351));
#41279=CARTESIAN_POINT('Ctrl Pts',(3.84113085985244,1.,1.67774874946079));
#41280=CARTESIAN_POINT('Ctrl Pts',(3.84583912296459,1.,1.6775199114018));
#41281=CARTESIAN_POINT('Ctrl Pts',(3.84897939430696,1.,1.67736057656533));
#41282=CARTESIAN_POINT('Ctrl Pts',(3.85054988729471,1.,1.67727921511438));
#41283=CARTESIAN_POINT('Origin',(3.85054988729471,0.,1.67727921511438));
#41284=CARTESIAN_POINT('',(3.90876544355381,1.,1.53673442965256));
#41285=CARTESIAN_POINT('Origin',(0.,0.,0.));
#41286=CARTESIAN_POINT('',(3.29885386921599,1.,1.78327315618183));
#41287=CARTESIAN_POINT('Origin',(0.,1.,0.));
#41288=CARTESIAN_POINT('Ctrl Pts',(3.29885386921599,1.,1.78327315618183));
#41289=CARTESIAN_POINT('Ctrl Pts',(3.29885386921599,0.666666666666667,1.78327315618183));
#41290=CARTESIAN_POINT('Ctrl Pts',(3.29885386921599,0.333333333333333,1.78327315618183));
#41291=CARTESIAN_POINT('Ctrl Pts',(3.29885386921599,-0.333333333333333,
1.78327315618183));
#41292=CARTESIAN_POINT('Ctrl Pts',(3.29885386921599,-0.666666666666667,
1.78327315618183));
#41293=CARTESIAN_POINT('Ctrl Pts',(3.29885386921599,-1.,1.78327315618183));
#41294=CARTESIAN_POINT('Ctrl Pts',(3.62024382630768,-1.,2.12928030988903));
#41295=CARTESIAN_POINT('Ctrl Pts',(3.62024382630768,1.,2.12928030988903));
#41296=CARTESIAN_POINT('Ctrl Pts',(3.61938653649098,-1.,2.12796193131368));
#41297=CARTESIAN_POINT('Ctrl Pts',(3.61938653649098,1.,2.12796193131368));
#41298=CARTESIAN_POINT('Ctrl Pts',(3.61766963590482,-1.,2.12532774376758));
#41299=CARTESIAN_POINT('Ctrl Pts',(3.61766963590482,1.,2.12532774376758));
#41300=CARTESIAN_POINT('Ctrl Pts',(3.61508732216891,-1.,2.12138417126355));
#41301=CARTESIAN_POINT('Ctrl Pts',(3.61508732216891,1.,2.12138417126355));
#41302=CARTESIAN_POINT('Ctrl Pts',(3.61163030609447,-1.,2.11614149815106));
#41303=CARTESIAN_POINT('Ctrl Pts',(3.61163030609447,1.,2.11614149815106));
#41304=CARTESIAN_POINT('Ctrl Pts',(3.60728578532601,-1.,2.10961391334462));
#41305=CARTESIAN_POINT('Ctrl Pts',(3.60728578532601,1.,2.10961391334462));
#41306=CARTESIAN_POINT('Ctrl Pts',(3.60291797088734,-1.,2.1031121772821));
#41307=CARTESIAN_POINT('Ctrl Pts',(3.60291797088734,1.,2.1031121772821));
#41308=CARTESIAN_POINT('Ctrl Pts',(3.59852681775485,-1.,2.09663642986631));
#41309=CARTESIAN_POINT('Ctrl Pts',(3.59852681775485,1.,2.09663642986631));
#41310=CARTESIAN_POINT('Ctrl Pts',(3.59411228625588,-1.,2.09018686331416));
#41311=CARTESIAN_POINT('Ctrl Pts',(3.59411228625588,1.,2.09018686331416));
#41312=CARTESIAN_POINT('Ctrl Pts',(3.58967435355088,-1.,2.08376373048756));
#41313=CARTESIAN_POINT('Ctrl Pts',(3.58967435355088,1.,2.08376373048756));
#41314=CARTESIAN_POINT('Ctrl Pts',(3.58521300039299,-1.,2.07736732842117));
#41315=CARTESIAN_POINT('Ctrl Pts',(3.58521300039299,1.,2.07736732842117));
#41316=CARTESIAN_POINT('Ctrl Pts',(3.58072819250442,-1.,2.07099797605747));
#41317=CARTESIAN_POINT('Ctrl Pts',(3.58072819250442,1.,2.07099797605747));
#41318=CARTESIAN_POINT('Ctrl Pts',(3.576219862243,-1.,2.06465599229174));
#41319=CARTESIAN_POINT('Ctrl Pts',(3.576219862243,1.,2.06465599229174));
#41320=CARTESIAN_POINT('Ctrl Pts',(3.57168789423507,-1.,2.05834167687524));
#41321=CARTESIAN_POINT('Ctrl Pts',(3.57168789423507,1.,2.05834167687524));
#41322=CARTESIAN_POINT('Ctrl Pts',(3.56713209978207,-1.,2.05205528173091));
#41323=CARTESIAN_POINT('Ctrl Pts',(3.56713209978207,1.,2.05205528173091));
#41324=CARTESIAN_POINT('Ctrl Pts',(3.5625522387181,-1.,2.04579702159056));
#41325=CARTESIAN_POINT('Ctrl Pts',(3.5625522387181,1.,2.04579702159056));
#41326=CARTESIAN_POINT('Ctrl Pts',(3.55794807265052,-1.,2.03956711120099));
#41327=CARTESIAN_POINT('Ctrl Pts',(3.55794807265052,1.,2.03956711120099));
#41328=CARTESIAN_POINT('Ctrl Pts',(3.55331941294018,-1.,2.03336579658174));
#41329=CARTESIAN_POINT('Ctrl Pts',(3.55331941294018,1.,2.03336579658174));
#41330=CARTESIAN_POINT('Ctrl Pts',(3.54866616282173,-1.,2.02719338376144));
#41331=CARTESIAN_POINT('Ctrl Pts',(3.54866616282173,1.,2.02719338376144));
#41332=CARTESIAN_POINT('Ctrl Pts',(3.54398838254011,-1.,2.0210502798303));
#41333=CARTESIAN_POINT('Ctrl Pts',(3.54398838254011,1.,2.0210502798303));
#41334=CARTESIAN_POINT('Ctrl Pts',(3.53928627453503,-1.,2.0149369884727));
#41335=CARTESIAN_POINT('Ctrl Pts',(3.53928627453503,1.,2.0149369884727));
#41336=CARTESIAN_POINT('Ctrl Pts',(3.53456004727321,-1.,2.00885403604685));
#41337=CARTESIAN_POINT('Ctrl Pts',(3.53456004727321,1.,2.00885403604685));
#41338=CARTESIAN_POINT('Ctrl Pts',(3.52980980250181,-1.,2.00280191090341));
#41339=CARTESIAN_POINT('Ctrl Pts',(3.52980980250181,1.,2.00280191090341));
#41340=CARTESIAN_POINT('Ctrl Pts',(3.52503542491745,-1.,1.99678100339306));
#41341=CARTESIAN_POINT('Ctrl Pts',(3.52503542491745,1.,1.99678100339306));
#41342=CARTESIAN_POINT('Ctrl Pts',(3.52023644289195,-1.,1.99079153006143));
#41343=CARTESIAN_POINT('Ctrl Pts',(3.52023644289195,1.,1.99079153006143));
#41344=CARTESIAN_POINT('Ctrl Pts',(3.51541198728362,-1.,1.98483351061066));
#41345=CARTESIAN_POINT('Ctrl Pts',(3.51541198728362,1.,1.98483351061066));
#41346=CARTESIAN_POINT('Ctrl Pts',(3.51056110478334,-1.,1.97890693666316));
#41347=CARTESIAN_POINT('Ctrl Pts',(3.51056110478334,1.,1.97890693666316));
#41348=CARTESIAN_POINT('Ctrl Pts',(3.505683018611,-1.,1.9730119116298));
#41349=CARTESIAN_POINT('Ctrl Pts',(3.505683018611,1.,1.9730119116298));
#41350=CARTESIAN_POINT('Ctrl Pts',(3.50077740176262,-1.,1.9671487972405));
#41351=CARTESIAN_POINT('Ctrl Pts',(3.50077740176262,1.,1.9671487972405));
#41352=CARTESIAN_POINT('Ctrl Pts',(3.49584466573045,-1.,1.96131836776489));
#41353=CARTESIAN_POINT('Ctrl Pts',(3.49584466573045,1.,1.96131836776489));
#41354=CARTESIAN_POINT('Ctrl Pts',(3.49088618670967,-1.,1.95552193112071));
#41355=CARTESIAN_POINT('Ctrl Pts',(3.49088618670967,1.,1.95552193112071));
#41356=CARTESIAN_POINT('Ctrl Pts',(3.485903616108,-1.,1.94976096795902));
#41357=CARTESIAN_POINT('Ctrl Pts',(3.485903616108,1.,1.94976096795902));
#41358=CARTESIAN_POINT('Ctrl Pts',(3.48089825770411,-1.,1.94403680554062));
#41359=CARTESIAN_POINT('Ctrl Pts',(3.48089825770411,1.,1.94403680554062));
#41360=CARTESIAN_POINT('Ctrl Pts',(3.47587040389916,-1.,1.93835026973888));
#41361=CARTESIAN_POINT('Ctrl Pts',(3.47587040389916,1.,1.93835026973888));
#41362=CARTESIAN_POINT('Ctrl Pts',(3.47081872409783,-1.,1.93270136427083));
#41363=CARTESIAN_POINT('Ctrl Pts',(3.47081872409783,1.,1.93270136427083));
#41364=CARTESIAN_POINT('Ctrl Pts',(3.46573953254084,-1.,1.92708888591159));
#41365=CARTESIAN_POINT('Ctrl Pts',(3.46573953254084,1.,1.92708888591159));
#41366=CARTESIAN_POINT('Ctrl Pts',(3.4606282172248,-1.,1.9215111821321));
#41367=CARTESIAN_POINT('Ctrl Pts',(3.4606282172248,1.,1.9215111821321));
#41368=CARTESIAN_POINT('Ctrl Pts',(3.45548074309943,-1.,1.9159669478406));
#41369=CARTESIAN_POINT('Ctrl Pts',(3.45548074309943,1.,1.9159669478406));
#41370=CARTESIAN_POINT('Ctrl Pts',(3.45029522038885,-1.,1.91045605593638));
#41371=CARTESIAN_POINT('Ctrl Pts',(3.45029522038885,1.,1.91045605593638));
#41372=CARTESIAN_POINT('Ctrl Pts',(3.44507323983374,-1.,1.90498026502308));
#41373=CARTESIAN_POINT('Ctrl Pts',(3.44507323983374,1.,1.90498026502308));
#41374=CARTESIAN_POINT('Ctrl Pts',(3.43982185678105,-1.,1.89954426803392));
#41375=CARTESIAN_POINT('Ctrl Pts',(3.43982185678105,1.,1.89954426803392));
#41376=CARTESIAN_POINT('Ctrl Pts',(3.43455074411591,-1.,1.89415420002553));
#41377=CARTESIAN_POINT('Ctrl Pts',(3.43455074411591,1.,1.89415420002553));
#41378=CARTESIAN_POINT('Ctrl Pts',(3.42926852222174,-1.,1.88881571322018));
#41379=CARTESIAN_POINT('Ctrl Pts',(3.42926852222174,1.,1.88881571322018));
#41380=CARTESIAN_POINT('Ctrl Pts',(3.42397908819741,-1.,1.88353205062063));
#41381=CARTESIAN_POINT('Ctrl Pts',(3.42397908819741,1.,1.88353205062063));
#41382=CARTESIAN_POINT('Ctrl Pts',(3.4186785838376,-1.,1.87830245689338));
#41383=CARTESIAN_POINT('Ctrl Pts',(3.4186785838376,1.,1.87830245689338));
#41384=CARTESIAN_POINT('Ctrl Pts',(3.41335043875182,-1.,1.87311957248106));
#41385=CARTESIAN_POINT('Ctrl Pts',(3.41335043875182,1.,1.87311957248106));
#41386=CARTESIAN_POINT('Ctrl Pts',(3.40797080000513,-1.,1.86797231196635));
#41387=CARTESIAN_POINT('Ctrl Pts',(3.40797080000513,1.,1.86797231196635));
#41388=CARTESIAN_POINT('Ctrl Pts',(3.40251742305445,-1.,1.86285057051228));
#41389=CARTESIAN_POINT('Ctrl Pts',(3.40251742305445,1.,1.86285057051228));
#41390=CARTESIAN_POINT('Ctrl Pts',(3.39697816833056,-1.,1.85774972037055));
#41391=CARTESIAN_POINT('Ctrl Pts',(3.39697816833056,1.,1.85774972037055));
#41392=CARTESIAN_POINT('Ctrl Pts',(3.39135802549415,-1.,1.85267433291778));
#41393=CARTESIAN_POINT('Ctrl Pts',(3.39135802549415,1.,1.85267433291778));
#41394=CARTESIAN_POINT('Ctrl Pts',(3.38569092349639,-1.,1.84764441927778));
#41395=CARTESIAN_POINT('Ctrl Pts',(3.38569092349639,1.,1.84764441927778));
#41396=CARTESIAN_POINT('Ctrl Pts',(3.38002968341222,-1.,1.84269016931679));
#41397=CARTESIAN_POINT('Ctrl Pts',(3.38002968341222,1.,1.84269016931679));
#41398=CARTESIAN_POINT('Ctrl Pts',(3.37442462015914,-1.,1.83784072967111));
#41399=CARTESIAN_POINT('Ctrl Pts',(3.37442462015914,1.,1.83784072967111));
#41400=CARTESIAN_POINT('Ctrl Pts',(3.36890396271864,-1.,1.83311391452338));
#41401=CARTESIAN_POINT('Ctrl Pts',(3.36890396271864,1.,1.83311391452338));
#41402=CARTESIAN_POINT('Ctrl Pts',(3.36345722124127,-1.,1.82850752153182));
#41403=CARTESIAN_POINT('Ctrl Pts',(3.36345722124127,1.,1.82850752153182));
#41404=CARTESIAN_POINT('Ctrl Pts',(3.35800801557326,-1.,1.82398496829247));
#41405=CARTESIAN_POINT('Ctrl Pts',(3.35800801557326,1.,1.82398496829247));
#41406=CARTESIAN_POINT('Ctrl Pts',(3.35243086937451,-1.,1.81948458796748));
#41407=CARTESIAN_POINT('Ctrl Pts',(3.35243086937451,1.,1.81948458796748));
#41408=CARTESIAN_POINT('Ctrl Pts',(3.34660014370527,-1.,1.81494618732772));
#41409=CARTESIAN_POINT('Ctrl Pts',(3.34660014370527,1.,1.81494618732772));
#41410=CARTESIAN_POINT('Ctrl Pts',(3.34043216147532,-1.,1.81033399625311));
#41411=CARTESIAN_POINT('Ctrl Pts',(3.34043216147532,1.,1.81033399625311));
#41412=CARTESIAN_POINT('Ctrl Pts',(3.33392460276874,-1.,1.80565802981139));
#41413=CARTESIAN_POINT('Ctrl Pts',(3.33392460276874,1.,1.80565802981139));
#41414=CARTESIAN_POINT('Ctrl Pts',(3.3272108803981,-1.,1.80100380443535));
#41415=CARTESIAN_POINT('Ctrl Pts',(3.3272108803981,1.,1.80100380443535));
#41416=CARTESIAN_POINT('Ctrl Pts',(3.32055355101168,-1.,1.79652817033444));
#41417=CARTESIAN_POINT('Ctrl Pts',(3.32055355101168,1.,1.79652817033444));
#41418=CARTESIAN_POINT('Ctrl Pts',(3.31428038326763,-1.,1.79242331350137));
#41419=CARTESIAN_POINT('Ctrl Pts',(3.31428038326763,1.,1.79242331350137));
#41420=CARTESIAN_POINT('Ctrl Pts',(3.30873412266954,-1.,1.78888832245965));
#41421=CARTESIAN_POINT('Ctrl Pts',(3.30873412266954,1.,1.78888832245965));
#41422=CARTESIAN_POINT('Ctrl Pts',(3.30422155558973,-1.,1.78610045419769));
#41423=CARTESIAN_POINT('Ctrl Pts',(3.30422155558973,1.,1.78610045419769));
#41424=CARTESIAN_POINT('Ctrl Pts',(3.30095096463082,-1.,1.78417972819697));
#41425=CARTESIAN_POINT('Ctrl Pts',(3.30095096463082,1.,1.78417972819697));
#41426=CARTESIAN_POINT('Ctrl Pts',(3.29940631673818,-1.,1.78338186555671));
#41427=CARTESIAN_POINT('Ctrl Pts',(3.29940631673818,1.,1.78338186555671));
#41428=CARTESIAN_POINT('Ctrl Pts',(3.29886572077303,-1.,1.78320756177191));
#41429=CARTESIAN_POINT('Ctrl Pts',(3.29886572077303,1.,1.78320756177191));
#41430=CARTESIAN_POINT('Ctrl Pts',(3.29877974053191,-1.,1.78327971836273));
#41431=CARTESIAN_POINT('Ctrl Pts',(3.29877974053191,1.,1.78327971836273));
#41432=CARTESIAN_POINT('Ctrl Pts',(3.2988053601491,-1.,1.7833628895577));
#41433=CARTESIAN_POINT('Ctrl Pts',(3.2988053601491,1.,1.7833628895577));
#41434=CARTESIAN_POINT('',(3.62024382630768,1.,2.12928030988903));
#41435=CARTESIAN_POINT('Ctrl Pts',(3.62024382630768,1.,2.12928030988903));
#41436=CARTESIAN_POINT('Ctrl Pts',(3.61938653649098,1.,2.12796193131368));
#41437=CARTESIAN_POINT('Ctrl Pts',(3.61766963590482,1.,2.12532774376758));
#41438=CARTESIAN_POINT('Ctrl Pts',(3.61508732216891,1.,2.12138417126355));
#41439=CARTESIAN_POINT('Ctrl Pts',(3.61163030609447,1.,2.11614149815106));
#41440=CARTESIAN_POINT('Ctrl Pts',(3.60728578532601,1.,2.10961391334462));
#41441=CARTESIAN_POINT('Ctrl Pts',(3.60291797088734,1.,2.1031121772821));
#41442=CARTESIAN_POINT('Ctrl Pts',(3.59852681775485,1.,2.09663642986631));
#41443=CARTESIAN_POINT('Ctrl Pts',(3.59411228625588,1.,2.09018686331416));
#41444=CARTESIAN_POINT('Ctrl Pts',(3.58967435355088,1.,2.08376373048756));
#41445=CARTESIAN_POINT('Ctrl Pts',(3.58521300039299,1.,2.07736732842117));
#41446=CARTESIAN_POINT('Ctrl Pts',(3.58072819250442,1.,2.07099797605747));
#41447=CARTESIAN_POINT('Ctrl Pts',(3.576219862243,1.,2.06465599229174));
#41448=CARTESIAN_POINT('Ctrl Pts',(3.57168789423507,1.,2.05834167687524));
#41449=CARTESIAN_POINT('Ctrl Pts',(3.56713209978207,1.,2.05205528173091));
#41450=CARTESIAN_POINT('Ctrl Pts',(3.5625522387181,1.,2.04579702159056));
#41451=CARTESIAN_POINT('Ctrl Pts',(3.55794807265052,1.,2.03956711120099));
#41452=CARTESIAN_POINT('Ctrl Pts',(3.55331941294018,1.,2.03336579658174));
#41453=CARTESIAN_POINT('Ctrl Pts',(3.54866616282173,1.,2.02719338376144));
#41454=CARTESIAN_POINT('Ctrl Pts',(3.54398838254011,1.,2.0210502798303));
#41455=CARTESIAN_POINT('Ctrl Pts',(3.53928627453503,1.,2.0149369884727));
#41456=CARTESIAN_POINT('Ctrl Pts',(3.53456004727321,1.,2.00885403604685));
#41457=CARTESIAN_POINT('Ctrl Pts',(3.52980980250181,1.,2.00280191090341));
#41458=CARTESIAN_POINT('Ctrl Pts',(3.52503542491745,1.,1.99678100339306));
#41459=CARTESIAN_POINT('Ctrl Pts',(3.52023644289195,1.,1.99079153006143));
#41460=CARTESIAN_POINT('Ctrl Pts',(3.51541198728362,1.,1.98483351061066));
#41461=CARTESIAN_POINT('Ctrl Pts',(3.51056110478334,1.,1.97890693666316));
#41462=CARTESIAN_POINT('Ctrl Pts',(3.505683018611,1.,1.9730119116298));
#41463=CARTESIAN_POINT('Ctrl Pts',(3.50077740176262,1.,1.9671487972405));
#41464=CARTESIAN_POINT('Ctrl Pts',(3.49584466573045,1.,1.96131836776489));
#41465=CARTESIAN_POINT('Ctrl Pts',(3.49088618670967,1.,1.95552193112071));
#41466=CARTESIAN_POINT('Ctrl Pts',(3.485903616108,1.,1.94976096795902));
#41467=CARTESIAN_POINT('Ctrl Pts',(3.48089825770411,1.,1.94403680554062));
#41468=CARTESIAN_POINT('Ctrl Pts',(3.47587040389916,1.,1.93835026973888));
#41469=CARTESIAN_POINT('Ctrl Pts',(3.47081872409783,1.,1.93270136427083));
#41470=CARTESIAN_POINT('Ctrl Pts',(3.46573953254084,1.,1.92708888591159));
#41471=CARTESIAN_POINT('Ctrl Pts',(3.4606282172248,1.,1.9215111821321));
#41472=CARTESIAN_POINT('Ctrl Pts',(3.45548074309943,1.,1.9159669478406));
#41473=CARTESIAN_POINT('Ctrl Pts',(3.45029522038885,1.,1.91045605593638));
#41474=CARTESIAN_POINT('Ctrl Pts',(3.44507323983374,1.,1.90498026502308));
#41475=CARTESIAN_POINT('Ctrl Pts',(3.43982185678105,1.,1.89954426803392));
#41476=CARTESIAN_POINT('Ctrl Pts',(3.43455074411591,1.,1.89415420002553));
#41477=CARTESIAN_POINT('Ctrl Pts',(3.42926852222174,1.,1.88881571322018));
#41478=CARTESIAN_POINT('Ctrl Pts',(3.42397908819741,1.,1.88353205062063));
#41479=CARTESIAN_POINT('Ctrl Pts',(3.4186785838376,1.,1.87830245689338));
#41480=CARTESIAN_POINT('Ctrl Pts',(3.41335043875182,1.,1.87311957248106));
#41481=CARTESIAN_POINT('Ctrl Pts',(3.40797080000513,1.,1.86797231196635));
#41482=CARTESIAN_POINT('Ctrl Pts',(3.40251742305445,1.,1.86285057051228));
#41483=CARTESIAN_POINT('Ctrl Pts',(3.39697816833056,1.,1.85774972037055));
#41484=CARTESIAN_POINT('Ctrl Pts',(3.39135802549415,1.,1.85267433291778));
#41485=CARTESIAN_POINT('Ctrl Pts',(3.38569092349639,1.,1.84764441927778));
#41486=CARTESIAN_POINT('Ctrl Pts',(3.38002968341222,1.,1.84269016931679));
#41487=CARTESIAN_POINT('Ctrl Pts',(3.37442462015914,1.,1.83784072967111));
#41488=CARTESIAN_POINT('Ctrl Pts',(3.36890396271864,1.,1.83311391452338));
#41489=CARTESIAN_POINT('Ctrl Pts',(3.36345722124127,1.,1.82850752153182));
#41490=CARTESIAN_POINT('Ctrl Pts',(3.35800801557326,1.,1.82398496829247));
#41491=CARTESIAN_POINT('Ctrl Pts',(3.35243086937451,1.,1.81948458796748));
#41492=CARTESIAN_POINT('Ctrl Pts',(3.34660014370527,1.,1.81494618732772));
#41493=CARTESIAN_POINT('Ctrl Pts',(3.34043216147532,1.,1.81033399625311));
#41494=CARTESIAN_POINT('Ctrl Pts',(3.33392460276874,1.,1.80565802981139));
#41495=CARTESIAN_POINT('Ctrl Pts',(3.3272108803981,1.,1.80100380443535));
#41496=CARTESIAN_POINT('Ctrl Pts',(3.32055355101168,1.,1.79652817033444));
#41497=CARTESIAN_POINT('Ctrl Pts',(3.31428038326763,1.,1.79242331350137));
#41498=CARTESIAN_POINT('Ctrl Pts',(3.30873412266954,1.,1.78888832245965));
#41499=CARTESIAN_POINT('Ctrl Pts',(3.30422155558973,1.,1.78610045419769));
#41500=CARTESIAN_POINT('Ctrl Pts',(3.30119637003466,1.,1.78432384788231));
#41501=CARTESIAN_POINT('Ctrl Pts',(3.29970549824337,1.,1.78353803106983));
#41502=CARTESIAN_POINT('Ctrl Pts',(3.29909749657945,1.,1.78329283591903));
#41503=CARTESIAN_POINT('Ctrl Pts',(3.29890219175522,1.,1.78326534445426));
#41504=CARTESIAN_POINT('Ctrl Pts',(3.29885386921599,1.,1.78327315618183));
#41505=CARTESIAN_POINT('',(3.62024382630768,0.,2.12928030988903));
#41506=CARTESIAN_POINT('Ctrl Pts',(3.08661426358891,-1.,2.12962728847315));
#41507=CARTESIAN_POINT('Ctrl Pts',(3.08661426358891,1.,2.12962728847315));
#41508=CARTESIAN_POINT('Ctrl Pts',(3.08652852644995,-1.,2.12964222016025));
#41509=CARTESIAN_POINT('Ctrl Pts',(3.08652852644995,1.,2.12964222016025));
#41510=CARTESIAN_POINT('Ctrl Pts',(3.08650326867133,-1.,2.12975158752407));
#41511=CARTESIAN_POINT('Ctrl Pts',(3.08650326867133,1.,2.12975158752407));
#41512=CARTESIAN_POINT('Ctrl Pts',(3.08690399991463,-1.,2.1301541297946));
#41513=CARTESIAN_POINT('Ctrl Pts',(3.08690399991463,1.,2.1301541297946));
#41514=CARTESIAN_POINT('Ctrl Pts',(3.08831615620074,-1.,2.13116819908542));
#41515=CARTESIAN_POINT('Ctrl Pts',(3.08831615620074,1.,2.13116819908542));
#41516=CARTESIAN_POINT('Ctrl Pts',(3.09151235281963,-1.,2.13321032560894));
#41517=CARTESIAN_POINT('Ctrl Pts',(3.09151235281963,1.,2.13321032560894));
#41518=CARTESIAN_POINT('Ctrl Pts',(3.0960450242104,-1.,2.13596538661048));
#41519=CARTESIAN_POINT('Ctrl Pts',(3.0960450242104,1.,2.13596538661048));
#41520=CARTESIAN_POINT('Ctrl Pts',(3.10171267391049,-1.,2.13930228863751));
#41521=CARTESIAN_POINT('Ctrl Pts',(3.10171267391049,1.,2.13930228863751));
#41522=CARTESIAN_POINT('Ctrl Pts',(3.10821808668859,-1.,2.14302815601973));
#41523=CARTESIAN_POINT('Ctrl Pts',(3.10821808668859,1.,2.14302815601973));
#41524=CARTESIAN_POINT('Ctrl Pts',(3.11522827016855,-1.,2.14692798457532));
#41525=CARTESIAN_POINT('Ctrl Pts',(3.11522827016855,1.,2.14692798457532));
#41526=CARTESIAN_POINT('Ctrl Pts',(3.12242318151938,-1.,2.15079698090585));
#41527=CARTESIAN_POINT('Ctrl Pts',(3.12242318151938,1.,2.15079698090585));
#41528=CARTESIAN_POINT('Ctrl Pts',(3.12954386795646,-1.,2.1544724138292));
#41529=CARTESIAN_POINT('Ctrl Pts',(3.12954386795646,1.,2.1544724138292));
#41530=CARTESIAN_POINT('Ctrl Pts',(3.13645356563038,-1.,2.15787423530676));
#41531=CARTESIAN_POINT('Ctrl Pts',(3.13645356563038,1.,2.15787423530676));
#41532=CARTESIAN_POINT('Ctrl Pts',(3.14314440427022,-1.,2.16100905914435));
#41533=CARTESIAN_POINT('Ctrl Pts',(3.14314440427022,1.,2.16100905914435));
#41534=CARTESIAN_POINT('Ctrl Pts',(3.14968624389054,-1.,2.16393520288072));
#41535=CARTESIAN_POINT('Ctrl Pts',(3.14968624389054,1.,2.16393520288072));
#41536=CARTESIAN_POINT('Ctrl Pts',(3.15618975593656,-1.,2.1667372844769));
#41537=CARTESIAN_POINT('Ctrl Pts',(3.15618975593656,1.,2.1667372844769));
#41538=CARTESIAN_POINT('Ctrl Pts',(3.16276685102972,-1.,2.16949910801219));
#41539=CARTESIAN_POINT('Ctrl Pts',(3.16276685102972,1.,2.16949910801219));
#41540=CARTESIAN_POINT('Ctrl Pts',(3.16948480019497,-1.,2.17227212063817));
#41541=CARTESIAN_POINT('Ctrl Pts',(3.16948480019497,1.,2.17227212063817));
#41542=CARTESIAN_POINT('Ctrl Pts',(3.17635032802523,-1.,2.17506466903694));
#41543=CARTESIAN_POINT('Ctrl Pts',(3.17635032802523,1.,2.17506466903694));
#41544=CARTESIAN_POINT('Ctrl Pts',(3.18333474627807,-1.,2.17785968847142));
#41545=CARTESIAN_POINT('Ctrl Pts',(3.18333474627807,1.,2.17785968847142));
#41546=CARTESIAN_POINT('Ctrl Pts',(3.19038924261573,-1.,2.18062558031778));
#41547=CARTESIAN_POINT('Ctrl Pts',(3.19038924261573,1.,2.18062558031778));
#41548=CARTESIAN_POINT('Ctrl Pts',(3.19746293740411,-1.,2.18332898656602));
#41549=CARTESIAN_POINT('Ctrl Pts',(3.19746293740411,1.,2.18332898656602));
#41550=CARTESIAN_POINT('Ctrl Pts',(3.20452259717976,-1.,2.18594876115934));
#41551=CARTESIAN_POINT('Ctrl Pts',(3.20452259717976,1.,2.18594876115934));
#41552=CARTESIAN_POINT('Ctrl Pts',(3.21156188355769,-1.,2.18848253363901));
#41553=CARTESIAN_POINT('Ctrl Pts',(3.21156188355769,1.,2.18848253363901));
#41554=CARTESIAN_POINT('Ctrl Pts',(3.21859043114095,-1.,2.19093901948667));
#41555=CARTESIAN_POINT('Ctrl Pts',(3.21859043114095,1.,2.19093901948667));
#41556=CARTESIAN_POINT('Ctrl Pts',(3.22562734221646,-1.,2.19333345123538));
#41557=CARTESIAN_POINT('Ctrl Pts',(3.22562734221646,1.,2.19333345123538));
#41558=CARTESIAN_POINT('Ctrl Pts',(3.23269332296933,-1.,2.19568204933168));
#41559=CARTESIAN_POINT('Ctrl Pts',(3.23269332296933,1.,2.19568204933168));
#41560=CARTESIAN_POINT('Ctrl Pts',(3.23980245361308,-1.,2.19799623693253));
#41561=CARTESIAN_POINT('Ctrl Pts',(3.23980245361308,1.,2.19799623693253));
#41562=CARTESIAN_POINT('Ctrl Pts',(3.24695715874338,-1.,2.20027910880981));
#41563=CARTESIAN_POINT('Ctrl Pts',(3.24695715874338,1.,2.20027910880981));
#41564=CARTESIAN_POINT('Ctrl Pts',(3.25415277957775,-1.,2.20252866491545));
#41565=CARTESIAN_POINT('Ctrl Pts',(3.25415277957775,1.,2.20252866491545));
#41566=CARTESIAN_POINT('Ctrl Pts',(3.26138036637705,-1.,2.20473979048678));
#41567=CARTESIAN_POINT('Ctrl Pts',(3.26138036637705,1.,2.20473979048678));
#41568=CARTESIAN_POINT('Ctrl Pts',(3.26863006136782,-1.,2.20690665217743));
#41569=CARTESIAN_POINT('Ctrl Pts',(3.26863006136782,1.,2.20690665217743));
#41570=CARTESIAN_POINT('Ctrl Pts',(3.2758944800554,-1.,2.2090250941743));
#41571=CARTESIAN_POINT('Ctrl Pts',(3.2758944800554,1.,2.2090250941743));
#41572=CARTESIAN_POINT('Ctrl Pts',(3.28317133333131,-1.,2.21109449750641));
#41573=CARTESIAN_POINT('Ctrl Pts',(3.28317133333131,1.,2.21109449750641));
#41574=CARTESIAN_POINT('Ctrl Pts',(3.29046159238343,-1.,2.21311648827391));
#41575=CARTESIAN_POINT('Ctrl Pts',(3.29046159238343,1.,2.21311648827391));
#41576=CARTESIAN_POINT('Ctrl Pts',(3.29776825193159,-1.,2.21509406923369));
#41577=CARTESIAN_POINT('Ctrl Pts',(3.29776825193159,1.,2.21509406923369));
#41578=CARTESIAN_POINT('Ctrl Pts',(3.30509487819569,-1.,2.21703059947836));
#41579=CARTESIAN_POINT('Ctrl Pts',(3.30509487819569,1.,2.21703059947836));
#41580=CARTESIAN_POINT('Ctrl Pts',(3.31244421655666,-1.,2.21892881679086));
#41581=CARTESIAN_POINT('Ctrl Pts',(3.31244421655666,1.,2.21892881679086));
#41582=CARTESIAN_POINT('Ctrl Pts',(3.31981686778022,-1.,2.22078990842776));
#41583=CARTESIAN_POINT('Ctrl Pts',(3.31981686778022,1.,2.22078990842776));
#41584=CARTESIAN_POINT('Ctrl Pts',(3.3272119632604,-1.,2.22261398879635));
#41585=CARTESIAN_POINT('Ctrl Pts',(3.3272119632604,1.,2.22261398879635));
#41586=CARTESIAN_POINT('Ctrl Pts',(3.33462772849598,-1.,2.22440049878511));
#41587=CARTESIAN_POINT('Ctrl Pts',(3.33462772849598,1.,2.22440049878511));
#41588=CARTESIAN_POINT('Ctrl Pts',(3.34206209449375,-1.,2.22614863918047));
#41589=CARTESIAN_POINT('Ctrl Pts',(3.34206209449375,1.,2.22614863918047));
#41590=CARTESIAN_POINT('Ctrl Pts',(3.34951327111096,-1.,2.22785777756576));
#41591=CARTESIAN_POINT('Ctrl Pts',(3.34951327111096,1.,2.22785777756576));
#41592=CARTESIAN_POINT('Ctrl Pts',(3.35698038165483,-1.,2.22952789880983));
#41593=CARTESIAN_POINT('Ctrl Pts',(3.35698038165483,1.,2.22952789880983));
#41594=CARTESIAN_POINT('Ctrl Pts',(3.36446325227848,-1.,2.23115945849739));
#41595=CARTESIAN_POINT('Ctrl Pts',(3.36446325227848,1.,2.23115945849739));
#41596=CARTESIAN_POINT('Ctrl Pts',(3.37196214349304,-1.,2.23275319569221));
#41597=CARTESIAN_POINT('Ctrl Pts',(3.37196214349304,1.,2.23275319569221));
#41598=CARTESIAN_POINT('Ctrl Pts',(3.37947749555632,-1.,2.23430995599561));
#41599=CARTESIAN_POINT('Ctrl Pts',(3.37947749555632,1.,2.23430995599561));
#41600=CARTESIAN_POINT('Ctrl Pts',(3.38700968549563,-1.,2.23583052276308));
#41601=CARTESIAN_POINT('Ctrl Pts',(3.38700968549563,1.,2.23583052276308));
#41602=CARTESIAN_POINT('Ctrl Pts',(3.39455873448189,-1.,2.23731541452791));
#41603=CARTESIAN_POINT('Ctrl Pts',(3.39455873448189,1.,2.23731541452791));
#41604=CARTESIAN_POINT('Ctrl Pts',(3.40212434705647,-1.,2.23876491124151));
#41605=CARTESIAN_POINT('Ctrl Pts',(3.40212434705647,1.,2.23876491124151));
#41606=CARTESIAN_POINT('Ctrl Pts',(3.40970604190328,-1.,2.24017914395289));
#41607=CARTESIAN_POINT('Ctrl Pts',(3.40970604190328,1.,2.24017914395289));
#41608=CARTESIAN_POINT('Ctrl Pts',(3.41730325539172,-1.,2.24155816587844));
#41609=CARTESIAN_POINT('Ctrl Pts',(3.41730325539172,1.,2.24155816587844));
#41610=CARTESIAN_POINT('Ctrl Pts',(3.42491544683008,-1.,2.24290202531101));
#41611=CARTESIAN_POINT('Ctrl Pts',(3.42491544683008,1.,2.24290202531101));
#41612=CARTESIAN_POINT('Ctrl Pts',(3.43254222614803,-1.,2.24421085338727));
#41613=CARTESIAN_POINT('Ctrl Pts',(3.43254222614803,1.,2.24421085338727));
#41614=CARTESIAN_POINT('Ctrl Pts',(3.4401833646032,-1.,2.24548487526022));
#41615=CARTESIAN_POINT('Ctrl Pts',(3.4401833646032,1.,2.24548487526022));
#41616=CARTESIAN_POINT('Ctrl Pts',(3.44783872863151,-1.,2.2467243706995));
#41617=CARTESIAN_POINT('Ctrl Pts',(3.44783872863151,1.,2.2467243706995));
#41618=CARTESIAN_POINT('Ctrl Pts',(3.45550823512049,-1.,2.2479296496077));
#41619=CARTESIAN_POINT('Ctrl Pts',(3.45550823512049,1.,2.2479296496077));
#41620=CARTESIAN_POINT('Ctrl Pts',(3.46319180177573,-1.,2.2491010234604));
#41621=CARTESIAN_POINT('Ctrl Pts',(3.46319180177573,1.,2.2491010234604));
#41622=CARTESIAN_POINT('Ctrl Pts',(3.47088928979888,-1.,2.25023877475942));
#41623=CARTESIAN_POINT('Ctrl Pts',(3.47088928979888,1.,2.25023877475942));
#41624=CARTESIAN_POINT('Ctrl Pts',(3.47860048448691,-1.,2.25134314238687));
#41625=CARTESIAN_POINT('Ctrl Pts',(3.47860048448691,1.,2.25134314238687));
#41626=CARTESIAN_POINT('Ctrl Pts',(3.48632513240961,-1.,2.25241433138695));
#41627=CARTESIAN_POINT('Ctrl Pts',(3.48632513240961,1.,2.25241433138695));
#41628=CARTESIAN_POINT('Ctrl Pts',(3.49406296494791,-1.,2.2534525170976));
#41629=CARTESIAN_POINT('Ctrl Pts',(3.49406296494791,1.,2.2534525170976));
#41630=CARTESIAN_POINT('Ctrl Pts',(3.50181372617971,-1.,2.25445785151868));
#41631=CARTESIAN_POINT('Ctrl Pts',(3.50181372617971,1.,2.25445785151868));
#41632=CARTESIAN_POINT('Ctrl Pts',(3.50957720117341,-1.,2.255430469798));
#41633=CARTESIAN_POINT('Ctrl Pts',(3.50957720117341,1.,2.255430469798));
#41634=CARTESIAN_POINT('Ctrl Pts',(3.51735323667612,-1.,2.25637049455044));
#41635=CARTESIAN_POINT('Ctrl Pts',(3.51735323667612,1.,2.25637049455044));
#41636=CARTESIAN_POINT('Ctrl Pts',(3.52514172847711,-1.,2.25727802940898));
#41637=CARTESIAN_POINT('Ctrl Pts',(3.52514172847711,1.,2.25727802940898));
#41638=CARTESIAN_POINT('Ctrl Pts',(3.53138243688262,-1.,2.25797812950104));
#41639=CARTESIAN_POINT('Ctrl Pts',(3.53138243688262,1.,2.25797812950104));
#41640=CARTESIAN_POINT('Ctrl Pts',(3.53606853162228,-1.,2.25848864343951));
#41641=CARTESIAN_POINT('Ctrl Pts',(3.53606853162228,1.,2.25848864343951));
#41642=CARTESIAN_POINT('Ctrl Pts',(3.53919506647335,-1.,2.2588225169468));
#41643=CARTESIAN_POINT('Ctrl Pts',(3.53919506647335,1.,2.2588225169468));
#41644=CARTESIAN_POINT('Ctrl Pts',(3.54075895182139,-1.,2.25898783642071));
#41645=CARTESIAN_POINT('Ctrl Pts',(3.54075895182139,1.,2.25898783642071));
#41646=CARTESIAN_POINT('',(3.08655633322212,1.,2.1297112484669));
#41647=CARTESIAN_POINT('Ctrl Pts',(3.08655633322211,-1.,2.1297112484669));
#41648=CARTESIAN_POINT('Ctrl Pts',(3.08655633322211,-0.666666666666667,
2.1297112484669));
#41649=CARTESIAN_POINT('Ctrl Pts',(3.08655633322211,-0.333333333333333,
2.1297112484669));
#41650=CARTESIAN_POINT('Ctrl Pts',(3.08655633322211,0.333333333333333,2.1297112484669));
#41651=CARTESIAN_POINT('Ctrl Pts',(3.08655633322212,0.666666666666667,2.1297112484669));
#41652=CARTESIAN_POINT('Ctrl Pts',(3.08655633322212,1.,2.1297112484669));
#41653=CARTESIAN_POINT('',(3.54075895182139,1.,2.25898783642071));
#41654=CARTESIAN_POINT('',(3.54075895182139,0.,2.25898783642071));
#41655=CARTESIAN_POINT('Ctrl Pts',(3.08655633322212,1.,2.1297112484669));
#41656=CARTESIAN_POINT('Ctrl Pts',(3.08657131089497,1.,2.1297578506149));
#41657=CARTESIAN_POINT('Ctrl Pts',(3.08668447250322,1.,2.12991938762374));
#41658=CARTESIAN_POINT('Ctrl Pts',(3.08717896996098,1.,2.13034980480424));
#41659=CARTESIAN_POINT('Ctrl Pts',(3.08855597949761,1.,2.13132142793017));
#41660=CARTESIAN_POINT('Ctrl Pts',(3.09151235281963,1.,2.13321032560894));
#41661=CARTESIAN_POINT('Ctrl Pts',(3.0960450242104,1.,2.13596538661048));
#41662=CARTESIAN_POINT('Ctrl Pts',(3.10171267391049,1.,2.13930228863751));
#41663=CARTESIAN_POINT('Ctrl Pts',(3.10821808668859,1.,2.14302815601973));
#41664=CARTESIAN_POINT('Ctrl Pts',(3.11522827016855,1.,2.14692798457532));
#41665=CARTESIAN_POINT('Ctrl Pts',(3.12242318151938,1.,2.15079698090585));
#41666=CARTESIAN_POINT('Ctrl Pts',(3.12954386795646,1.,2.1544724138292));
#41667=CARTESIAN_POINT('Ctrl Pts',(3.13645356563038,1.,2.15787423530676));
#41668=CARTESIAN_POINT('Ctrl Pts',(3.14314440427022,1.,2.16100905914435));
#41669=CARTESIAN_POINT('Ctrl Pts',(3.14968624389054,1.,2.16393520288072));
#41670=CARTESIAN_POINT('Ctrl Pts',(3.15618975593656,1.,2.1667372844769));
#41671=CARTESIAN_POINT('Ctrl Pts',(3.16276685102972,1.,2.16949910801219));
#41672=CARTESIAN_POINT('Ctrl Pts',(3.16948480019497,1.,2.17227212063817));
#41673=CARTESIAN_POINT('Ctrl Pts',(3.17635032802523,1.,2.17506466903694));
#41674=CARTESIAN_POINT('Ctrl Pts',(3.18333474627807,1.,2.17785968847142));
#41675=CARTESIAN_POINT('Ctrl Pts',(3.19038924261573,1.,2.18062558031778));
#41676=CARTESIAN_POINT('Ctrl Pts',(3.19746293740411,1.,2.18332898656602));
#41677=CARTESIAN_POINT('Ctrl Pts',(3.20452259717976,1.,2.18594876115934));
#41678=CARTESIAN_POINT('Ctrl Pts',(3.21156188355769,1.,2.18848253363901));
#41679=CARTESIAN_POINT('Ctrl Pts',(3.21859043114095,1.,2.19093901948667));
#41680=CARTESIAN_POINT('Ctrl Pts',(3.22562734221646,1.,2.19333345123538));
#41681=CARTESIAN_POINT('Ctrl Pts',(3.23269332296933,1.,2.19568204933168));
#41682=CARTESIAN_POINT('Ctrl Pts',(3.23980245361308,1.,2.19799623693253));
#41683=CARTESIAN_POINT('Ctrl Pts',(3.24695715874338,1.,2.20027910880981));
#41684=CARTESIAN_POINT('Ctrl Pts',(3.25415277957775,1.,2.20252866491545));
#41685=CARTESIAN_POINT('Ctrl Pts',(3.26138036637705,1.,2.20473979048678));
#41686=CARTESIAN_POINT('Ctrl Pts',(3.26863006136782,1.,2.20690665217743));
#41687=CARTESIAN_POINT('Ctrl Pts',(3.2758944800554,1.,2.2090250941743));
#41688=CARTESIAN_POINT('Ctrl Pts',(3.28317133333131,1.,2.21109449750641));
#41689=CARTESIAN_POINT('Ctrl Pts',(3.29046159238343,1.,2.21311648827391));
#41690=CARTESIAN_POINT('Ctrl Pts',(3.29776825193159,1.,2.21509406923369));
#41691=CARTESIAN_POINT('Ctrl Pts',(3.30509487819569,1.,2.21703059947836));
#41692=CARTESIAN_POINT('Ctrl Pts',(3.31244421655666,1.,2.21892881679086));
#41693=CARTESIAN_POINT('Ctrl Pts',(3.31981686778022,1.,2.22078990842776));
#41694=CARTESIAN_POINT('Ctrl Pts',(3.3272119632604,1.,2.22261398879635));
#41695=CARTESIAN_POINT('Ctrl Pts',(3.33462772849598,1.,2.22440049878511));
#41696=CARTESIAN_POINT('Ctrl Pts',(3.34206209449375,1.,2.22614863918047));
#41697=CARTESIAN_POINT('Ctrl Pts',(3.34951327111096,1.,2.22785777756576));
#41698=CARTESIAN_POINT('Ctrl Pts',(3.35698038165483,1.,2.22952789880983));
#41699=CARTESIAN_POINT('Ctrl Pts',(3.36446325227848,1.,2.23115945849739));
#41700=CARTESIAN_POINT('Ctrl Pts',(3.37196214349304,1.,2.23275319569221));
#41701=CARTESIAN_POINT('Ctrl Pts',(3.37947749555632,1.,2.23430995599561));
#41702=CARTESIAN_POINT('Ctrl Pts',(3.38700968549563,1.,2.23583052276308));
#41703=CARTESIAN_POINT('Ctrl Pts',(3.39455873448189,1.,2.23731541452791));
#41704=CARTESIAN_POINT('Ctrl Pts',(3.40212434705647,1.,2.23876491124151));
#41705=CARTESIAN_POINT('Ctrl Pts',(3.40970604190328,1.,2.24017914395289));
#41706=CARTESIAN_POINT('Ctrl Pts',(3.41730325539172,1.,2.24155816587844));
#41707=CARTESIAN_POINT('Ctrl Pts',(3.42491544683008,1.,2.24290202531101));
#41708=CARTESIAN_POINT('Ctrl Pts',(3.43254222614803,1.,2.24421085338727));
#41709=CARTESIAN_POINT('Ctrl Pts',(3.4401833646032,1.,2.24548487526022));
#41710=CARTESIAN_POINT('Ctrl Pts',(3.44783872863151,1.,2.2467243706995));
#41711=CARTESIAN_POINT('Ctrl Pts',(3.45550823512049,1.,2.2479296496077));
#41712=CARTESIAN_POINT('Ctrl Pts',(3.46319180177573,1.,2.2491010234604));
#41713=CARTESIAN_POINT('Ctrl Pts',(3.47088928979888,1.,2.25023877475942));
#41714=CARTESIAN_POINT('Ctrl Pts',(3.47860048448691,1.,2.25134314238687));
#41715=CARTESIAN_POINT('Ctrl Pts',(3.48632513240961,1.,2.25241433138695));
#41716=CARTESIAN_POINT('Ctrl Pts',(3.49406296494791,1.,2.2534525170976));
#41717=CARTESIAN_POINT('Ctrl Pts',(3.50181372617971,1.,2.25445785151868));
#41718=CARTESIAN_POINT('Ctrl Pts',(3.50957720117341,1.,2.255430469798));
#41719=CARTESIAN_POINT('Ctrl Pts',(3.51735323667612,1.,2.25637049455044));
#41720=CARTESIAN_POINT('Ctrl Pts',(3.52514172847711,1.,2.25727802940898));
#41721=CARTESIAN_POINT('Ctrl Pts',(3.53138243688262,1.,2.25797812950104));
#41722=CARTESIAN_POINT('Ctrl Pts',(3.53606853162228,1.,2.25848864343951));
#41723=CARTESIAN_POINT('Ctrl Pts',(3.53919506647335,1.,2.2588225169468));
#41724=CARTESIAN_POINT('Ctrl Pts',(3.54075895182139,1.,2.25898783642071));
#41725=CARTESIAN_POINT('Origin',(3.54075895182139,0.,2.25898783642071));
#41726=CARTESIAN_POINT('',(3.62024382630768,1.,2.12928030988903));
#41727=CARTESIAN_POINT('Origin',(0.,0.,0.));
#41728=CARTESIAN_POINT('',(2.97927412174388,1.,2.27737254473378));
#41729=CARTESIAN_POINT('Origin',(0.,1.,0.));
#41730=CARTESIAN_POINT('Ctrl Pts',(2.97927412174388,1.,2.27737254473378));
#41731=CARTESIAN_POINT('Ctrl Pts',(2.97927412174388,0.666666666666667,2.27737254473378));
#41732=CARTESIAN_POINT('Ctrl Pts',(2.97927412174388,0.333333333333333,2.27737254473378));
#41733=CARTESIAN_POINT('Ctrl Pts',(2.97927412174388,-0.333333333333333,
2.27737254473378));
#41734=CARTESIAN_POINT('Ctrl Pts',(2.97927412174388,-0.666666666666667,
2.27737254473378));
#41735=CARTESIAN_POINT('Ctrl Pts',(2.97927412174388,-1.,2.27737254473378));
#41736=CARTESIAN_POINT('Ctrl Pts',(3.24257979115744,-1.,2.66939624221984));
#41737=CARTESIAN_POINT('Ctrl Pts',(3.24257979115744,1.,2.66939624221984));
#41738=CARTESIAN_POINT('Ctrl Pts',(3.24193929584813,-1.,2.66795998539861));
#41739=CARTESIAN_POINT('Ctrl Pts',(3.24193929584813,1.,2.66795998539861));
#41740=CARTESIAN_POINT('Ctrl Pts',(3.24065561087681,-1.,2.66508964664767));
#41741=CARTESIAN_POINT('Ctrl Pts',(3.24065561087681,1.,2.66508964664767));
#41742=CARTESIAN_POINT('Ctrl Pts',(3.23872200036311,-1.,2.6607906631973));
#41743=CARTESIAN_POINT('Ctrl Pts',(3.23872200036311,1.,2.6607906631973));
#41744=CARTESIAN_POINT('Ctrl Pts',(3.23612768065687,-1.,2.6550717396303));
#41745=CARTESIAN_POINT('Ctrl Pts',(3.23612768065687,1.,2.6550717396303));
#41746=CARTESIAN_POINT('Ctrl Pts',(3.23285778738558,-1.,2.64794488744246));
#41747=CARTESIAN_POINT('Ctrl Pts',(3.23285778738558,1.,2.64794488744246));
#41748=CARTESIAN_POINT('Ctrl Pts',(3.2295608435934,-1.,2.64083992182478));
#41749=CARTESIAN_POINT('Ctrl Pts',(3.2295608435934,1.,2.64083992182478));
#41750=CARTESIAN_POINT('Ctrl Pts',(3.22623678292539,-1.,2.63375697391438));
#41751=CARTESIAN_POINT('Ctrl Pts',(3.22623678292539,1.,2.63375697391438));
#41752=CARTESIAN_POINT('Ctrl Pts',(3.222885536128,-1.,2.62669622735548));
#41753=CARTESIAN_POINT('Ctrl Pts',(3.222885536128,1.,2.62669622735548));
#41754=CARTESIAN_POINT('Ctrl Pts',(3.21950704108654,-1.,2.61965792832396));
#41755=CARTESIAN_POINT('Ctrl Pts',(3.21950704108654,1.,2.61965792832396));
#41756=CARTESIAN_POINT('Ctrl Pts',(3.21610123232465,-1.,2.61264236718662));
#41757=CARTESIAN_POINT('Ctrl Pts',(3.21610123232465,1.,2.61264236718662));
#41758=CARTESIAN_POINT('Ctrl Pts',(3.21266802609297,-1.,2.60564985359699));
#41759=CARTESIAN_POINT('Ctrl Pts',(3.21266802609297,1.,2.60564985359699));
#41760=CARTESIAN_POINT('Ctrl Pts',(3.2092073056959,-1.,2.59868069194267));
#41761=CARTESIAN_POINT('Ctrl Pts',(3.2092073056959,1.,2.59868069194267));
#41762=CARTESIAN_POINT('Ctrl Pts',(3.20571891028879,-1.,2.59173516023605));
#41763=CARTESIAN_POINT('Ctrl Pts',(3.20571891028879,1.,2.59173516023605));
#41764=CARTESIAN_POINT('Ctrl Pts',(3.20220261408685,-1.,2.58481347777953));
#41765=CARTESIAN_POINT('Ctrl Pts',(3.20220261408685,1.,2.58481347777953));
#41766=CARTESIAN_POINT('Ctrl Pts',(3.19865814628955,-1.,2.577915819091));
#41767=CARTESIAN_POINT('Ctrl Pts',(3.19865814628955,1.,2.577915819091));
#41768=CARTESIAN_POINT('Ctrl Pts',(3.19508523784548,-1.,2.57104235898053));
#41769=CARTESIAN_POINT('Ctrl Pts',(3.19508523784548,1.,2.57104235898053));
#41770=CARTESIAN_POINT('Ctrl Pts',(3.19148366395201,-1.,2.56419331092909));
#41771=CARTESIAN_POINT('Ctrl Pts',(3.19148366395201,1.,2.56419331092909));
#41772=CARTESIAN_POINT('Ctrl Pts',(3.1878532811617,-1.,2.55736896206016));
#41773=CARTESIAN_POINT('Ctrl Pts',(3.1878532811617,1.,2.55736896206016));
#41774=CARTESIAN_POINT('Ctrl Pts',(3.18419408529482,-1.,2.55056972387638));
#41775=CARTESIAN_POINT('Ctrl Pts',(3.18419408529482,1.,2.55056972387638));
#41776=CARTESIAN_POINT('Ctrl Pts',(3.18050619750515,-1.,2.54379612552948));
#41777=CARTESIAN_POINT('Ctrl Pts',(3.18050619750515,1.,2.54379612552948));
#41778=CARTESIAN_POINT('Ctrl Pts',(3.17678974135225,-1.,2.53704871950871));
#41779=CARTESIAN_POINT('Ctrl Pts',(3.17678974135225,1.,2.53704871950871));
#41780=CARTESIAN_POINT('Ctrl Pts',(3.17304474093574,-1.,2.5303280040691));
#41781=CARTESIAN_POINT('Ctrl Pts',(3.17304474093574,1.,2.5303280040691));
#41782=CARTESIAN_POINT('Ctrl Pts',(3.1692710213075,-1.,2.523634346718));
#41783=CARTESIAN_POINT('Ctrl Pts',(3.1692710213075,1.,2.523634346718));
#41784=CARTESIAN_POINT('Ctrl Pts',(3.16546808277069,-1.,2.51696788755616));
#41785=CARTESIAN_POINT('Ctrl Pts',(3.16546808277069,1.,2.51696788755616));
#41786=CARTESIAN_POINT('Ctrl Pts',(3.16163506380211,-1.,2.51032851007939));
#41787=CARTESIAN_POINT('Ctrl Pts',(3.16163506380211,1.,2.51032851007939));
#41788=CARTESIAN_POINT('Ctrl Pts',(3.15777102413998,-1.,2.50371605688287));
#41789=CARTESIAN_POINT('Ctrl Pts',(3.15777102413998,1.,2.50371605688287));
#41790=CARTESIAN_POINT('Ctrl Pts',(3.15387518039064,-1.,2.49713050858911));
#41791=CARTESIAN_POINT('Ctrl Pts',(3.15387518039064,1.,2.49713050858911));
#41792=CARTESIAN_POINT('Ctrl Pts',(3.14994715298903,-1.,2.49057217131985));
#41793=CARTESIAN_POINT('Ctrl Pts',(3.14994715298903,1.,2.49057217131985));
#41794=CARTESIAN_POINT('Ctrl Pts',(3.14598722723879,-1.,2.48404187418376));
#41795=CARTESIAN_POINT('Ctrl Pts',(3.14598722723879,1.,2.48404187418376));
#41796=CARTESIAN_POINT('Ctrl Pts',(3.14199655778845,-1.,2.47754112428028));
#41797=CARTESIAN_POINT('Ctrl Pts',(3.14199655778845,1.,2.47754112428028));
#41798=CARTESIAN_POINT('Ctrl Pts',(3.13797654408931,-1.,2.47107164236827));
#41799=CARTESIAN_POINT('Ctrl Pts',(3.13797654408931,1.,2.47107164236827));
#41800=CARTESIAN_POINT('Ctrl Pts',(3.13392826623902,-1.,2.4646349433237));
#41801=CARTESIAN_POINT('Ctrl Pts',(3.13392826623902,1.,2.4646349433237));
#41802=CARTESIAN_POINT('Ctrl Pts',(3.12985188384372,-1.,2.45823188859367));
#41803=CARTESIAN_POINT('Ctrl Pts',(3.12985188384372,1.,2.45823188859367));
#41804=CARTESIAN_POINT('Ctrl Pts',(3.12574608210849,-1.,2.45186227369848));
#41805=CARTESIAN_POINT('Ctrl Pts',(3.12574608210849,1.,2.45186227369848));
#41806=CARTESIAN_POINT('Ctrl Pts',(3.12160740887768,-1.,2.44552433364716));
#41807=CARTESIAN_POINT('Ctrl Pts',(3.12160740887768,1.,2.44552433364716));
#41808=CARTESIAN_POINT('Ctrl Pts',(3.11743156744182,-1.,2.43921571477975));
#41809=CARTESIAN_POINT('Ctrl Pts',(3.11743156744182,1.,2.43921571477975));
#41810=CARTESIAN_POINT('Ctrl Pts',(3.11321477659012,-1.,2.4329344968514));
#41811=CARTESIAN_POINT('Ctrl Pts',(3.11321477659012,1.,2.4329344968514));
#41812=CARTESIAN_POINT('Ctrl Pts',(3.10895518969592,-1.,2.42668025870013));
#41813=CARTESIAN_POINT('Ctrl Pts',(3.10895518969592,1.,2.42668025870013));
#41814=CARTESIAN_POINT('Ctrl Pts',(3.10465410280902,-1.,2.42045498612494));
#41815=CARTESIAN_POINT('Ctrl Pts',(3.10465410280902,1.,2.42045498612494));
#41816=CARTESIAN_POINT('Ctrl Pts',(3.10031775027683,-1.,2.41426441798067));
#41817=CARTESIAN_POINT('Ctrl Pts',(3.10031775027683,1.,2.41426441798067));
#41818=CARTESIAN_POINT('Ctrl Pts',(3.09595472616093,-1.,2.40811612696382));
#41819=CARTESIAN_POINT('Ctrl Pts',(3.09595472616093,1.,2.40811612696382));
#41820=CARTESIAN_POINT('Ctrl Pts',(3.09157266051115,-1.,2.40201704423352));
#41821=CARTESIAN_POINT('Ctrl Pts',(3.09157266051115,1.,2.40201704423352));
#41822=CARTESIAN_POINT('Ctrl Pts',(3.08717489512919,-1.,2.39597098250635));
#41823=CARTESIAN_POINT('Ctrl Pts',(3.08717489512919,1.,2.39597098250635));
#41824=CARTESIAN_POINT('Ctrl Pts',(3.08275773747083,-1.,2.38997659219192));
#41825=CARTESIAN_POINT('Ctrl Pts',(3.08275773747083,1.,2.38997659219192));
#41826=CARTESIAN_POINT('Ctrl Pts',(3.07830597244301,-1.,2.38402401216107));
#41827=CARTESIAN_POINT('Ctrl Pts',(3.07830597244301,1.,2.38402401216107));
#41828=CARTESIAN_POINT('Ctrl Pts',(3.07379777492133,-1.,2.37809856205524));
#41829=CARTESIAN_POINT('Ctrl Pts',(3.07379777492133,1.,2.37809856205524));
#41830=CARTESIAN_POINT('Ctrl Pts',(3.06921275497472,-1.,2.37218678163157));
#41831=CARTESIAN_POINT('Ctrl Pts',(3.06921275497472,1.,2.37218678163157));
#41832=CARTESIAN_POINT('Ctrl Pts',(3.06453964643152,-1.,2.36628220107001));
#41833=CARTESIAN_POINT('Ctrl Pts',(3.06453964643152,1.,2.36628220107001));
#41834=CARTESIAN_POINT('Ctrl Pts',(3.05978266240056,-1.,2.36039011602084));
#41835=CARTESIAN_POINT('Ctrl Pts',(3.05978266240056,1.,2.36039011602084));
#41836=CARTESIAN_POINT('Ctrl Pts',(3.05497218368188,-1.,2.35453559889506));
#41837=CARTESIAN_POINT('Ctrl Pts',(3.05497218368188,1.,2.35453559889506));
#41838=CARTESIAN_POINT('Ctrl Pts',(3.05015565829976,-1.,2.34875673090816));
#41839=CARTESIAN_POINT('Ctrl Pts',(3.05015565829976,1.,2.34875673090816));
#41840=CARTESIAN_POINT('Ctrl Pts',(3.04537822217311,-1.,2.3430901708402));
#41841=CARTESIAN_POINT('Ctrl Pts',(3.04537822217311,1.,2.3430901708402));
#41842=CARTESIAN_POINT('Ctrl Pts',(3.04066496998569,-1.,2.33755792953726));
#41843=CARTESIAN_POINT('Ctrl Pts',(3.04066496998569,1.,2.33755792953726));
#41844=CARTESIAN_POINT('Ctrl Pts',(3.03600588555765,-1.,2.33215619079807));
#41845=CARTESIAN_POINT('Ctrl Pts',(3.03600588555765,1.,2.33215619079807));
#41846=CARTESIAN_POINT('Ctrl Pts',(3.03133125185047,-1.,2.32683687412027));
#41847=CARTESIAN_POINT('Ctrl Pts',(3.03133125185047,1.,2.32683687412027));
#41848=CARTESIAN_POINT('Ctrl Pts',(3.02652678416478,-1.,2.32151944306299));
#41849=CARTESIAN_POINT('Ctrl Pts',(3.02652678416478,1.,2.32151944306299));
#41850=CARTESIAN_POINT('Ctrl Pts',(3.02147780668029,-1.,2.31612479121528));
#41851=CARTESIAN_POINT('Ctrl Pts',(3.02147780668029,1.,2.31612479121528));
#41852=CARTESIAN_POINT('Ctrl Pts',(3.01610726819019,-1.,2.31060449886577));
#41853=CARTESIAN_POINT('Ctrl Pts',(3.01610726819019,1.,2.31060449886577));
#41854=CARTESIAN_POINT('Ctrl Pts',(3.01041131063882,-1.,2.30496809486529));
#41855=CARTESIAN_POINT('Ctrl Pts',(3.01041131063882,1.,2.30496809486529));
#41856=CARTESIAN_POINT('Ctrl Pts',(3.00450832658822,-1.,2.29932091315939));
#41857=CARTESIAN_POINT('Ctrl Pts',(3.00450832658822,1.,2.29932091315939));
#41858=CARTESIAN_POINT('Ctrl Pts',(2.99863310340004,-1.,2.29385894577999));
#41859=CARTESIAN_POINT('Ctrl Pts',(2.99863310340004,1.,2.29385894577999));
#41860=CARTESIAN_POINT('Ctrl Pts',(2.9930793098434,-1.,2.28882328690601));
#41861=CARTESIAN_POINT('Ctrl Pts',(2.9930793098434,1.,2.28882328690601));
#41862=CARTESIAN_POINT('Ctrl Pts',(2.98815432734929,-1.,2.28446419116036));
#41863=CARTESIAN_POINT('Ctrl Pts',(2.98815432734929,1.,2.28446419116036));
#41864=CARTESIAN_POINT('Ctrl Pts',(2.98413343613858,-1.,2.28100472516582));
#41865=CARTESIAN_POINT('Ctrl Pts',(2.98413343613858,1.,2.28100472516582));
#41866=CARTESIAN_POINT('Ctrl Pts',(2.98120357932601,-1.,2.2785960133424));
#41867=CARTESIAN_POINT('Ctrl Pts',(2.98120357932601,1.,2.2785960133424));
#41868=CARTESIAN_POINT('Ctrl Pts',(2.97980276182744,-1.,2.27756633754846));
#41869=CARTESIAN_POINT('Ctrl Pts',(2.97980276182744,1.,2.27756633754846));
#41870=CARTESIAN_POINT('Ctrl Pts',(2.97929608861502,-1.,2.27730961189188));
#41871=CARTESIAN_POINT('Ctrl Pts',(2.97929608861502,1.,2.27730961189188));
#41872=CARTESIAN_POINT('Ctrl Pts',(2.97919987915565,-1.,2.2773674298423));
#41873=CARTESIAN_POINT('Ctrl Pts',(2.97919987915565,1.,2.2773674298423));
#41874=CARTESIAN_POINT('Ctrl Pts',(2.97921217251145,-1.,2.27745358485296));
#41875=CARTESIAN_POINT('Ctrl Pts',(2.97921217251145,1.,2.27745358485296));
#41876=CARTESIAN_POINT('',(3.24257979115744,1.,2.66939624221984));
#41877=CARTESIAN_POINT('Ctrl Pts',(3.24257979115744,1.,2.66939624221984));
#41878=CARTESIAN_POINT('Ctrl Pts',(3.24193929584813,1.,2.66795998539861));
#41879=CARTESIAN_POINT('Ctrl Pts',(3.24065561087681,1.,2.66508964664767));
#41880=CARTESIAN_POINT('Ctrl Pts',(3.23872200036311,1.,2.6607906631973));
#41881=CARTESIAN_POINT('Ctrl Pts',(3.23612768065687,1.,2.6550717396303));
#41882=CARTESIAN_POINT('Ctrl Pts',(3.23285778738558,1.,2.64794488744246));
#41883=CARTESIAN_POINT('Ctrl Pts',(3.2295608435934,1.,2.64083992182478));
#41884=CARTESIAN_POINT('Ctrl Pts',(3.22623678292539,1.,2.63375697391438));
#41885=CARTESIAN_POINT('Ctrl Pts',(3.222885536128,1.,2.62669622735548));
#41886=CARTESIAN_POINT('Ctrl Pts',(3.21950704108654,1.,2.61965792832396));
#41887=CARTESIAN_POINT('Ctrl Pts',(3.21610123232465,1.,2.61264236718662));
#41888=CARTESIAN_POINT('Ctrl Pts',(3.21266802609297,1.,2.60564985359699));
#41889=CARTESIAN_POINT('Ctrl Pts',(3.2092073056959,1.,2.59868069194267));
#41890=CARTESIAN_POINT('Ctrl Pts',(3.20571891028879,1.,2.59173516023605));
#41891=CARTESIAN_POINT('Ctrl Pts',(3.20220261408685,1.,2.58481347777953));
#41892=CARTESIAN_POINT('Ctrl Pts',(3.19865814628955,1.,2.577915819091));
#41893=CARTESIAN_POINT('Ctrl Pts',(3.19508523784548,1.,2.57104235898053));
#41894=CARTESIAN_POINT('Ctrl Pts',(3.19148366395201,1.,2.56419331092909));
#41895=CARTESIAN_POINT('Ctrl Pts',(3.1878532811617,1.,2.55736896206016));
#41896=CARTESIAN_POINT('Ctrl Pts',(3.18419408529482,1.,2.55056972387638));
#41897=CARTESIAN_POINT('Ctrl Pts',(3.18050619750515,1.,2.54379612552948));
#41898=CARTESIAN_POINT('Ctrl Pts',(3.17678974135225,1.,2.53704871950871));
#41899=CARTESIAN_POINT('Ctrl Pts',(3.17304474093574,1.,2.5303280040691));
#41900=CARTESIAN_POINT('Ctrl Pts',(3.1692710213075,1.,2.523634346718));
#41901=CARTESIAN_POINT('Ctrl Pts',(3.16546808277069,1.,2.51696788755616));
#41902=CARTESIAN_POINT('Ctrl Pts',(3.16163506380211,1.,2.51032851007939));
#41903=CARTESIAN_POINT('Ctrl Pts',(3.15777102413998,1.,2.50371605688287));
#41904=CARTESIAN_POINT('Ctrl Pts',(3.15387518039064,1.,2.49713050858911));
#41905=CARTESIAN_POINT('Ctrl Pts',(3.14994715298903,1.,2.49057217131985));
#41906=CARTESIAN_POINT('Ctrl Pts',(3.14598722723879,1.,2.48404187418376));
#41907=CARTESIAN_POINT('Ctrl Pts',(3.14199655778845,1.,2.47754112428028));
#41908=CARTESIAN_POINT('Ctrl Pts',(3.13797654408931,1.,2.47107164236827));
#41909=CARTESIAN_POINT('Ctrl Pts',(3.13392826623902,1.,2.4646349433237));
#41910=CARTESIAN_POINT('Ctrl Pts',(3.12985188384372,1.,2.45823188859367));
#41911=CARTESIAN_POINT('Ctrl Pts',(3.12574608210849,1.,2.45186227369848));
#41912=CARTESIAN_POINT('Ctrl Pts',(3.12160740887768,1.,2.44552433364716));
#41913=CARTESIAN_POINT('Ctrl Pts',(3.11743156744182,1.,2.43921571477975));
#41914=CARTESIAN_POINT('Ctrl Pts',(3.11321477659012,1.,2.4329344968514));
#41915=CARTESIAN_POINT('Ctrl Pts',(3.10895518969592,1.,2.42668025870013));
#41916=CARTESIAN_POINT('Ctrl Pts',(3.10465410280902,1.,2.42045498612494));
#41917=CARTESIAN_POINT('Ctrl Pts',(3.10031775027683,1.,2.41426441798067));
#41918=CARTESIAN_POINT('Ctrl Pts',(3.09595472616093,1.,2.40811612696382));
#41919=CARTESIAN_POINT('Ctrl Pts',(3.09157266051115,1.,2.40201704423352));
#41920=CARTESIAN_POINT('Ctrl Pts',(3.08717489512919,1.,2.39597098250635));
#41921=CARTESIAN_POINT('Ctrl Pts',(3.08275773747083,1.,2.38997659219192));
#41922=CARTESIAN_POINT('Ctrl Pts',(3.07830597244301,1.,2.38402401216107));
#41923=CARTESIAN_POINT('Ctrl Pts',(3.07379777492133,1.,2.37809856205524));
#41924=CARTESIAN_POINT('Ctrl Pts',(3.06921275497472,1.,2.37218678163157));
#41925=CARTESIAN_POINT('Ctrl Pts',(3.06453964643152,1.,2.36628220107001));
#41926=CARTESIAN_POINT('Ctrl Pts',(3.05978266240056,1.,2.36039011602084));
#41927=CARTESIAN_POINT('Ctrl Pts',(3.05497218368188,1.,2.35453559889506));
#41928=CARTESIAN_POINT('Ctrl Pts',(3.05015565829976,1.,2.34875673090816));
#41929=CARTESIAN_POINT('Ctrl Pts',(3.04537822217311,1.,2.3430901708402));
#41930=CARTESIAN_POINT('Ctrl Pts',(3.04066496998569,1.,2.33755792953726));
#41931=CARTESIAN_POINT('Ctrl Pts',(3.03600588555765,1.,2.33215619079807));
#41932=CARTESIAN_POINT('Ctrl Pts',(3.03133125185047,1.,2.32683687412027));
#41933=CARTESIAN_POINT('Ctrl Pts',(3.02652678416478,1.,2.32151944306299));
#41934=CARTESIAN_POINT('Ctrl Pts',(3.02147780668029,1.,2.31612479121528));
#41935=CARTESIAN_POINT('Ctrl Pts',(3.01610726819019,1.,2.31060449886577));
#41936=CARTESIAN_POINT('Ctrl Pts',(3.01041131063882,1.,2.30496809486529));
#41937=CARTESIAN_POINT('Ctrl Pts',(3.00450832658822,1.,2.29932091315939));
#41938=CARTESIAN_POINT('Ctrl Pts',(2.99863310340004,1.,2.29385894577999));
#41939=CARTESIAN_POINT('Ctrl Pts',(2.9930793098434,1.,2.28882328690601));
#41940=CARTESIAN_POINT('Ctrl Pts',(2.98815432734929,1.,2.28446419116036));
#41941=CARTESIAN_POINT('Ctrl Pts',(2.98413343613858,1.,2.28100472516582));
#41942=CARTESIAN_POINT('Ctrl Pts',(2.98142341809623,1.,2.27877674853833));
#41943=CARTESIAN_POINT('Ctrl Pts',(2.98007383024333,1.,2.27776738270369));
#41944=CARTESIAN_POINT('Ctrl Pts',(2.97951167106106,1.,2.27743009389704));
#41945=CARTESIAN_POINT('Ctrl Pts',(2.97932307137589,1.,2.27737238849212));
#41946=CARTESIAN_POINT('Ctrl Pts',(2.97927412174388,1.,2.27737254473378));
#41947=CARTESIAN_POINT('',(3.24257979115744,0.,2.66939624221984));
#41948=CARTESIAN_POINT('Ctrl Pts',(2.71546581445404,-1.,2.58626089374824));
#41949=CARTESIAN_POINT('Ctrl Pts',(2.71546581445404,1.,2.58626089374824));
#41950=CARTESIAN_POINT('Ctrl Pts',(2.71537879705104,-1.,2.58626222935804));
#41951=CARTESIAN_POINT('Ctrl Pts',(2.71537879705104,1.,2.58626222935804));
#41952=CARTESIAN_POINT('Ctrl Pts',(2.71533674141254,-1.,2.58636629904103));
#41953=CARTESIAN_POINT('Ctrl Pts',(2.71533674141254,1.,2.58636629904103));
#41954=CARTESIAN_POINT('Ctrl Pts',(2.71566956750452,-1.,2.5868265735259));
#41955=CARTESIAN_POINT('Ctrl Pts',(2.71566956750452,1.,2.5868265735259));
#41956=CARTESIAN_POINT('Ctrl Pts',(2.71690570241638,-1.,2.58804906785417));
#41957=CARTESIAN_POINT('Ctrl Pts',(2.71690570241638,1.,2.58804906785417));
#41958=CARTESIAN_POINT('Ctrl Pts',(2.71974308958086,-1.,2.59056604771971));
#41959=CARTESIAN_POINT('Ctrl Pts',(2.71974308958086,1.,2.59056604771971));
#41960=CARTESIAN_POINT('Ctrl Pts',(2.72378896977134,-1.,2.59399625537278));
#41961=CARTESIAN_POINT('Ctrl Pts',(2.72378896977134,1.,2.59399625537278));
#41962=CARTESIAN_POINT('Ctrl Pts',(2.7288648348152,-1.,2.59817869034746));
#41963=CARTESIAN_POINT('Ctrl Pts',(2.7288648348152,1.,2.59817869034746));
#41964=CARTESIAN_POINT('Ctrl Pts',(2.73470730109615,-1.,2.60287635688728));
#41965=CARTESIAN_POINT('Ctrl Pts',(2.73470730109615,1.,2.60287635688728));
#41966=CARTESIAN_POINT('Ctrl Pts',(2.7410211099909,-1.,2.60782480638448));
#41967=CARTESIAN_POINT('Ctrl Pts',(2.7410211099909,1.,2.60782480638448));
#41968=CARTESIAN_POINT('Ctrl Pts',(2.74752219567252,-1.,2.61277170105813));
#41969=CARTESIAN_POINT('Ctrl Pts',(2.74752219567252,1.,2.61277170105813));
#41970=CARTESIAN_POINT('Ctrl Pts',(2.7539802502603,-1.,2.61751580407667));
#41971=CARTESIAN_POINT('Ctrl Pts',(2.7539802502603,1.,2.61751580407667));
#41972=CARTESIAN_POINT('Ctrl Pts',(2.76027271596686,-1.,2.62195665834605));
#41973=CARTESIAN_POINT('Ctrl Pts',(2.76027271596686,1.,2.62195665834605));
#41974=CARTESIAN_POINT('Ctrl Pts',(2.7663907847902,-1.,2.62609956506355));
#41975=CARTESIAN_POINT('Ctrl Pts',(2.7663907847902,1.,2.62609956506355));
#41976=CARTESIAN_POINT('Ctrl Pts',(2.77239433377921,-1.,2.63001305229625));
#41977=CARTESIAN_POINT('Ctrl Pts',(2.77239433377921,1.,2.63001305229625));
#41978=CARTESIAN_POINT('Ctrl Pts',(2.77837943466449,-1.,2.63379800904599));
#41979=CARTESIAN_POINT('Ctrl Pts',(2.77837943466449,1.,2.63379800904599));
#41980=CARTESIAN_POINT('Ctrl Pts',(2.78444351041571,-1.,2.637554714303));
#41981=CARTESIAN_POINT('Ctrl Pts',(2.78444351041571,1.,2.637554714303));
#41982=CARTESIAN_POINT('Ctrl Pts',(2.79064495573224,-1.,2.64134450532584));
#41983=CARTESIAN_POINT('Ctrl Pts',(2.79064495573224,1.,2.64134450532584));
#41984=CARTESIAN_POINT('Ctrl Pts',(2.79698910670736,-1.,2.6451766779932));
#41985=CARTESIAN_POINT('Ctrl Pts',(2.79698910670736,1.,2.6451766779932));
#41986=CARTESIAN_POINT('Ctrl Pts',(2.80345029781152,-1.,2.64902988983337));
#41987=CARTESIAN_POINT('Ctrl Pts',(2.80345029781152,1.,2.64902988983337));
#41988=CARTESIAN_POINT('Ctrl Pts',(2.80998526078165,-1.,2.65286529532208));
#41989=CARTESIAN_POINT('Ctrl Pts',(2.80998526078165,1.,2.65286529532208));
#41990=CARTESIAN_POINT('Ctrl Pts',(2.81654896073883,-1.,2.65664198781344));
#41991=CARTESIAN_POINT('Ctrl Pts',(2.81654896073883,1.,2.65664198781344));
#41992=CARTESIAN_POINT('Ctrl Pts',(2.82311188135078,-1.,2.66033388273461));
#41993=CARTESIAN_POINT('Ctrl Pts',(2.82311188135078,1.,2.66033388273461));
#41994=CARTESIAN_POINT('Ctrl Pts',(2.82966813308998,-1.,2.6639376472693));
#41995=CARTESIAN_POINT('Ctrl Pts',(2.82966813308998,1.,2.6639376472693));
#41996=CARTESIAN_POINT('Ctrl Pts',(2.83622586853982,-1.,2.66746339678107));
#41997=CARTESIAN_POINT('Ctrl Pts',(2.83622586853982,1.,2.66746339678107));
#41998=CARTESIAN_POINT('Ctrl Pts',(2.84280157191323,-1.,2.67092916452125));
#41999=CARTESIAN_POINT('Ctrl Pts',(2.84280157191323,1.,2.67092916452125));
#42000=CARTESIAN_POINT('Ctrl Pts',(2.84941315703092,-1.,2.67435421039677));
#42001=CARTESIAN_POINT('Ctrl Pts',(2.84941315703092,1.,2.67435421039677));
#42002=CARTESIAN_POINT('Ctrl Pts',(2.85607274378017,-1.,2.67775201955724));
#42003=CARTESIAN_POINT('Ctrl Pts',(2.85607274378017,1.,2.67775201955724));
#42004=CARTESIAN_POINT('Ctrl Pts',(2.86278224277689,-1.,2.68112602796308));
#42005=CARTESIAN_POINT('Ctrl Pts',(2.86278224277689,1.,2.68112602796308));
#42006=CARTESIAN_POINT('Ctrl Pts',(2.86953736547238,-1.,2.68447353139599));
#42007=CARTESIAN_POINT('Ctrl Pts',(2.86953736547238,1.,2.68447353139599));
#42008=CARTESIAN_POINT('Ctrl Pts',(2.8763300724388,-1.,2.68778807801686));
#42009=CARTESIAN_POINT('Ctrl Pts',(2.8763300724388,1.,2.68778807801686));
#42010=CARTESIAN_POINT('Ctrl Pts',(2.88315153980466,-1.,2.69106236420198));
#42011=CARTESIAN_POINT('Ctrl Pts',(2.88315153980466,1.,2.69106236420198));
#42012=CARTESIAN_POINT('Ctrl Pts',(2.88999512410309,-1.,2.69429113011374));
#42013=CARTESIAN_POINT('Ctrl Pts',(2.88999512410309,1.,2.69429113011374));
#42014=CARTESIAN_POINT('Ctrl Pts',(2.89685866123671,-1.,2.69747340630625));
#42015=CARTESIAN_POINT('Ctrl Pts',(2.89685866123671,1.,2.69747340630625));
#42016=CARTESIAN_POINT('Ctrl Pts',(2.90374285605838,-1.,2.70061095078692));
#42017=CARTESIAN_POINT('Ctrl Pts',(2.90374285605838,1.,2.70061095078692));
#42018=CARTESIAN_POINT('Ctrl Pts',(2.91065019668329,-1.,2.70370719782113));
#42019=CARTESIAN_POINT('Ctrl Pts',(2.91065019668329,1.,2.70370719782113));
#42020=CARTESIAN_POINT('Ctrl Pts',(2.91758367994737,-1.,2.70676602302518));
#42021=CARTESIAN_POINT('Ctrl Pts',(2.91758367994737,1.,2.70676602302518));
#42022=CARTESIAN_POINT('Ctrl Pts',(2.92454558914778,-1.,2.70979055994754));
#42023=CARTESIAN_POINT('Ctrl Pts',(2.92454558914778,1.,2.70979055994754));
#42024=CARTESIAN_POINT('Ctrl Pts',(2.93153633192595,-1.,2.71278207520817));
#42025=CARTESIAN_POINT('Ctrl Pts',(2.93153633192595,1.,2.71278207520817));
#42026=CARTESIAN_POINT('Ctrl Pts',(2.93855503247266,-1.,2.71574054592591));
#42027=CARTESIAN_POINT('Ctrl Pts',(2.93855503247266,1.,2.71574054592591));
#42028=CARTESIAN_POINT('Ctrl Pts',(2.94560002559805,-1.,2.71866514227965));
#42029=CARTESIAN_POINT('Ctrl Pts',(2.94560002559805,1.,2.71866514227965));
#42030=CARTESIAN_POINT('Ctrl Pts',(2.95266939280621,-1.,2.72155475123364));
#42031=CARTESIAN_POINT('Ctrl Pts',(2.95266939280621,1.,2.72155475123364));
#42032=CARTESIAN_POINT('Ctrl Pts',(2.95976146492576,-1.,2.72440846811729));
#42033=CARTESIAN_POINT('Ctrl Pts',(2.95976146492576,1.,2.72440846811729));
#42034=CARTESIAN_POINT('Ctrl Pts',(2.96687537842451,-1.,2.72722614084076));
#42035=CARTESIAN_POINT('Ctrl Pts',(2.96687537842451,1.,2.72722614084076));
#42036=CARTESIAN_POINT('Ctrl Pts',(2.97401089032676,-1.,2.73000819218414));
#42037=CARTESIAN_POINT('Ctrl Pts',(2.97401089032676,1.,2.73000819218414));
#42038=CARTESIAN_POINT('Ctrl Pts',(2.98116814232129,-1.,2.73275539286497));
#42039=CARTESIAN_POINT('Ctrl Pts',(2.98116814232129,1.,2.73275539286497));
#42040=CARTESIAN_POINT('Ctrl Pts',(2.9883474369644,-1.,2.73546864694536));
#42041=CARTESIAN_POINT('Ctrl Pts',(2.9883474369644,1.,2.73546864694536));
#42042=CARTESIAN_POINT('Ctrl Pts',(2.99554902409778,-1.,2.73814878711641));
#42043=CARTESIAN_POINT('Ctrl Pts',(2.99554902409778,1.,2.73814878711641));
#42044=CARTESIAN_POINT('Ctrl Pts',(3.00277284351521,-1.,2.74079632883931));
#42045=CARTESIAN_POINT('Ctrl Pts',(3.00277284351521,1.,2.74079632883931));
#42046=CARTESIAN_POINT('Ctrl Pts',(3.01001855960162,-1.,2.74341150239887));
#42047=CARTESIAN_POINT('Ctrl Pts',(3.01001855960162,1.,2.74341150239887));
#42048=CARTESIAN_POINT('Ctrl Pts',(3.01728567646611,-1.,2.74599436193625));
#42049=CARTESIAN_POINT('Ctrl Pts',(3.01728567646611,1.,2.74599436193625));
#42050=CARTESIAN_POINT('Ctrl Pts',(3.02457362909245,-1.,2.7485448718414));
#42051=CARTESIAN_POINT('Ctrl Pts',(3.02457362909245,1.,2.7485448718414));
#42052=CARTESIAN_POINT('Ctrl Pts',(3.03188187589107,-1.,2.75106299522979));
#42053=CARTESIAN_POINT('Ctrl Pts',(3.03188187589107,1.,2.75106299522979));
#42054=CARTESIAN_POINT('Ctrl Pts',(3.03921001107977,-1.,2.75354880060314));
#42055=CARTESIAN_POINT('Ctrl Pts',(3.03921001107977,1.,2.75354880060314));
#42056=CARTESIAN_POINT('Ctrl Pts',(3.04655777351067,-1.,2.75600247455925));
#42057=CARTESIAN_POINT('Ctrl Pts',(3.04655777351067,1.,2.75600247455925));
#42058=CARTESIAN_POINT('Ctrl Pts',(3.05392498749847,-1.,2.75842427252931));
#42059=CARTESIAN_POINT('Ctrl Pts',(3.05392498749847,1.,2.75842427252931));
#42060=CARTESIAN_POINT('Ctrl Pts',(3.06131152247454,-1.,2.76081448759882));
#42061=CARTESIAN_POINT('Ctrl Pts',(3.06131152247454,1.,2.76081448759882));
#42062=CARTESIAN_POINT('Ctrl Pts',(3.0687172484321,-1.,2.76317341453493));
#42063=CARTESIAN_POINT('Ctrl Pts',(3.0687172484321,1.,2.76317341453493));
#42064=CARTESIAN_POINT('Ctrl Pts',(3.07614198408862,-1.,2.76550131064852));
#42065=CARTESIAN_POINT('Ctrl Pts',(3.07614198408862,1.,2.76550131064852));
#42066=CARTESIAN_POINT('Ctrl Pts',(3.08358548001503,-1.,2.76779837829373));
#42067=CARTESIAN_POINT('Ctrl Pts',(3.08358548001503,1.,2.76779837829373));
#42068=CARTESIAN_POINT('Ctrl Pts',(3.0910474538253,-1.,2.7700647803451));
#42069=CARTESIAN_POINT('Ctrl Pts',(3.0910474538253,1.,2.7700647803451));
#42070=CARTESIAN_POINT('Ctrl Pts',(3.0985276127786,-1.,2.77230064796057));
#42071=CARTESIAN_POINT('Ctrl Pts',(3.0985276127786,1.,2.77230064796057));
#42072=CARTESIAN_POINT('Ctrl Pts',(3.10602568032564,-1.,2.77450609123362));
#42073=CARTESIAN_POINT('Ctrl Pts',(3.10602568032564,1.,2.77450609123362));
#42074=CARTESIAN_POINT('Ctrl Pts',(3.11354142303921,-1.,2.77668121002545));
#42075=CARTESIAN_POINT('Ctrl Pts',(3.11354142303921,1.,2.77668121002545));
#42076=CARTESIAN_POINT('Ctrl Pts',(3.12107467037201,-1.,2.77882610146731));
#42077=CARTESIAN_POINT('Ctrl Pts',(3.12107467037201,1.,2.77882610146731));
#42078=CARTESIAN_POINT('Ctrl Pts',(3.12862530318457,-1.,2.78094085161413));
#42079=CARTESIAN_POINT('Ctrl Pts',(3.12862530318457,1.,2.78094085161413));
#42080=CARTESIAN_POINT('Ctrl Pts',(3.13467965833037,-1.,2.78260859419319));
#42081=CARTESIAN_POINT('Ctrl Pts',(3.13467965833037,1.,2.78260859419319));
#42082=CARTESIAN_POINT('Ctrl Pts',(3.13922819749279,-1.,2.78384588958166));
#42083=CARTESIAN_POINT('Ctrl Pts',(3.13922819749279,1.,2.78384588958166));
#42084=CARTESIAN_POINT('Ctrl Pts',(3.14226401018816,-1.,2.7846647503589));
#42085=CARTESIAN_POINT('Ctrl Pts',(3.14226401018816,1.,2.7846647503589));
#42086=CARTESIAN_POINT('Ctrl Pts',(3.14378277984898,-1.,2.78507268004356));
#42087=CARTESIAN_POINT('Ctrl Pts',(3.14378277984898,1.,2.78507268004356));
#42088=CARTESIAN_POINT('',(2.71539546306948,1.,2.58633475774921));
#42089=CARTESIAN_POINT('Ctrl Pts',(2.71539546306948,-1.,2.58633475774921));
#42090=CARTESIAN_POINT('Ctrl Pts',(2.71539546306948,-0.666666666666667,
2.58633475774921));
#42091=CARTESIAN_POINT('Ctrl Pts',(2.71539546306948,-0.333333333333333,
2.58633475774921));
#42092=CARTESIAN_POINT('Ctrl Pts',(2.71539546306948,0.333333333333333,2.58633475774921));
#42093=CARTESIAN_POINT('Ctrl Pts',(2.71539546306948,0.666666666666667,2.58633475774921));
#42094=CARTESIAN_POINT('Ctrl Pts',(2.71539546306948,1.,2.58633475774921));
#42095=CARTESIAN_POINT('',(3.14378277984898,1.,2.78507268004356));
#42096=CARTESIAN_POINT('',(3.14378277984898,0.,2.78507268004356));
#42097=CARTESIAN_POINT('Ctrl Pts',(2.71539546306948,1.,2.58633475774921));
#42098=CARTESIAN_POINT('Ctrl Pts',(2.71540296616024,1.,2.58638312917167));
#42099=CARTESIAN_POINT('Ctrl Pts',(2.71548946460575,1.,2.58656037976753));
#42100=CARTESIAN_POINT('Ctrl Pts',(2.71591054189786,1.,2.58706285424358));
#42101=CARTESIAN_POINT('Ctrl Pts',(2.71711860281815,1.,2.58823792682672));
#42102=CARTESIAN_POINT('Ctrl Pts',(2.71974308958086,1.,2.59056604771971));
#42103=CARTESIAN_POINT('Ctrl Pts',(2.72378896977134,1.,2.59399625537278));
#42104=CARTESIAN_POINT('Ctrl Pts',(2.7288648348152,1.,2.59817869034746));
#42105=CARTESIAN_POINT('Ctrl Pts',(2.73470730109615,1.,2.60287635688728));
#42106=CARTESIAN_POINT('Ctrl Pts',(2.7410211099909,1.,2.60782480638448));
#42107=CARTESIAN_POINT('Ctrl Pts',(2.74752219567252,1.,2.61277170105813));
#42108=CARTESIAN_POINT('Ctrl Pts',(2.7539802502603,1.,2.61751580407667));
#42109=CARTESIAN_POINT('Ctrl Pts',(2.76027271596686,1.,2.62195665834605));
#42110=CARTESIAN_POINT('Ctrl Pts',(2.7663907847902,1.,2.62609956506355));
#42111=CARTESIAN_POINT('Ctrl Pts',(2.77239433377921,1.,2.63001305229625));
#42112=CARTESIAN_POINT('Ctrl Pts',(2.77837943466449,1.,2.63379800904599));
#42113=CARTESIAN_POINT('Ctrl Pts',(2.78444351041571,1.,2.637554714303));
#42114=CARTESIAN_POINT('Ctrl Pts',(2.79064495573224,1.,2.64134450532584));
#42115=CARTESIAN_POINT('Ctrl Pts',(2.79698910670736,1.,2.6451766779932));
#42116=CARTESIAN_POINT('Ctrl Pts',(2.80345029781152,1.,2.64902988983337));
#42117=CARTESIAN_POINT('Ctrl Pts',(2.80998526078165,1.,2.65286529532208));
#42118=CARTESIAN_POINT('Ctrl Pts',(2.81654896073883,1.,2.65664198781344));
#42119=CARTESIAN_POINT('Ctrl Pts',(2.82311188135078,1.,2.66033388273461));
#42120=CARTESIAN_POINT('Ctrl Pts',(2.82966813308998,1.,2.6639376472693));
#42121=CARTESIAN_POINT('Ctrl Pts',(2.83622586853982,1.,2.66746339678107));
#42122=CARTESIAN_POINT('Ctrl Pts',(2.84280157191323,1.,2.67092916452125));
#42123=CARTESIAN_POINT('Ctrl Pts',(2.84941315703092,1.,2.67435421039677));
#42124=CARTESIAN_POINT('Ctrl Pts',(2.85607274378017,1.,2.67775201955724));
#42125=CARTESIAN_POINT('Ctrl Pts',(2.86278224277689,1.,2.68112602796308));
#42126=CARTESIAN_POINT('Ctrl Pts',(2.86953736547238,1.,2.68447353139599));
#42127=CARTESIAN_POINT('Ctrl Pts',(2.8763300724388,1.,2.68778807801686));
#42128=CARTESIAN_POINT('Ctrl Pts',(2.88315153980466,1.,2.69106236420198));
#42129=CARTESIAN_POINT('Ctrl Pts',(2.88999512410309,1.,2.69429113011374));
#42130=CARTESIAN_POINT('Ctrl Pts',(2.89685866123671,1.,2.69747340630625));
#42131=CARTESIAN_POINT('Ctrl Pts',(2.90374285605838,1.,2.70061095078692));
#42132=CARTESIAN_POINT('Ctrl Pts',(2.91065019668329,1.,2.70370719782113));
#42133=CARTESIAN_POINT('Ctrl Pts',(2.91758367994737,1.,2.70676602302518));
#42134=CARTESIAN_POINT('Ctrl Pts',(2.92454558914778,1.,2.70979055994754));
#42135=CARTESIAN_POINT('Ctrl Pts',(2.93153633192595,1.,2.71278207520817));
#42136=CARTESIAN_POINT('Ctrl Pts',(2.93855503247266,1.,2.71574054592591));
#42137=CARTESIAN_POINT('Ctrl Pts',(2.94560002559805,1.,2.71866514227965));
#42138=CARTESIAN_POINT('Ctrl Pts',(2.95266939280621,1.,2.72155475123364));
#42139=CARTESIAN_POINT('Ctrl Pts',(2.95976146492576,1.,2.72440846811729));
#42140=CARTESIAN_POINT('Ctrl Pts',(2.96687537842451,1.,2.72722614084076));
#42141=CARTESIAN_POINT('Ctrl Pts',(2.97401089032676,1.,2.73000819218414));
#42142=CARTESIAN_POINT('Ctrl Pts',(2.98116814232129,1.,2.73275539286497));
#42143=CARTESIAN_POINT('Ctrl Pts',(2.9883474369644,1.,2.73546864694536));
#42144=CARTESIAN_POINT('Ctrl Pts',(2.99554902409778,1.,2.73814878711641));
#42145=CARTESIAN_POINT('Ctrl Pts',(3.00277284351521,1.,2.74079632883931));
#42146=CARTESIAN_POINT('Ctrl Pts',(3.01001855960162,1.,2.74341150239887));
#42147=CARTESIAN_POINT('Ctrl Pts',(3.01728567646611,1.,2.74599436193625));
#42148=CARTESIAN_POINT('Ctrl Pts',(3.02457362909245,1.,2.7485448718414));
#42149=CARTESIAN_POINT('Ctrl Pts',(3.03188187589107,1.,2.75106299522979));
#42150=CARTESIAN_POINT('Ctrl Pts',(3.03921001107977,1.,2.75354880060314));
#42151=CARTESIAN_POINT('Ctrl Pts',(3.04655777351067,1.,2.75600247455925));
#42152=CARTESIAN_POINT('Ctrl Pts',(3.05392498749847,1.,2.75842427252931));
#42153=CARTESIAN_POINT('Ctrl Pts',(3.06131152247454,1.,2.76081448759882));
#42154=CARTESIAN_POINT('Ctrl Pts',(3.0687172484321,1.,2.76317341453493));
#42155=CARTESIAN_POINT('Ctrl Pts',(3.07614198408862,1.,2.76550131064852));
#42156=CARTESIAN_POINT('Ctrl Pts',(3.08358548001503,1.,2.76779837829373));
#42157=CARTESIAN_POINT('Ctrl Pts',(3.0910474538253,1.,2.7700647803451));
#42158=CARTESIAN_POINT('Ctrl Pts',(3.0985276127786,1.,2.77230064796057));
#42159=CARTESIAN_POINT('Ctrl Pts',(3.10602568032564,1.,2.77450609123362));
#42160=CARTESIAN_POINT('Ctrl Pts',(3.11354142303921,1.,2.77668121002545));
#42161=CARTESIAN_POINT('Ctrl Pts',(3.12107467037201,1.,2.77882610146731));
#42162=CARTESIAN_POINT('Ctrl Pts',(3.12862530318457,1.,2.78094085161413));
#42163=CARTESIAN_POINT('Ctrl Pts',(3.13467965833037,1.,2.78260859419319));
#42164=CARTESIAN_POINT('Ctrl Pts',(3.13922819749279,1.,2.78384588958166));
#42165=CARTESIAN_POINT('Ctrl Pts',(3.14226401018816,1.,2.7846647503589));
#42166=CARTESIAN_POINT('Ctrl Pts',(3.14378277984898,1.,2.78507268004356));
#42167=CARTESIAN_POINT('Origin',(3.14378277984898,0.,2.78507268004356));
#42168=CARTESIAN_POINT('',(3.24257979115744,1.,2.66939624221984));
#42169=CARTESIAN_POINT('Origin',(0.,0.,0.));
#42170=CARTESIAN_POINT('',(2.58633475775051,1.,2.71539546306824));
#42171=CARTESIAN_POINT('Origin',(0.,1.,0.));
#42172=CARTESIAN_POINT('Ctrl Pts',(2.58633475775051,1.,2.71539546306824));
#42173=CARTESIAN_POINT('Ctrl Pts',(2.58633475775051,0.666666666666667,2.71539546306824));
#42174=CARTESIAN_POINT('Ctrl Pts',(2.58633475775051,0.333333333333333,2.71539546306824));
#42175=CARTESIAN_POINT('Ctrl Pts',(2.58633475775051,-0.333333333333333,
2.71539546306824));
#42176=CARTESIAN_POINT('Ctrl Pts',(2.58633475775051,-0.666666666666667,
2.71539546306824));
#42177=CARTESIAN_POINT('Ctrl Pts',(2.58633475775051,-1.,2.71539546306824));
#42178=CARTESIAN_POINT('Ctrl Pts',(2.78507268004355,-1.,3.14378277984898));
#42179=CARTESIAN_POINT('Ctrl Pts',(2.78507268004355,1.,3.14378277984898));
#42180=CARTESIAN_POINT('Ctrl Pts',(2.78466475036183,-1.,3.14226401019149));
#42181=CARTESIAN_POINT('Ctrl Pts',(2.78466475036183,1.,3.14226401019149));
#42182=CARTESIAN_POINT('Ctrl Pts',(2.78384588958965,-1.,3.13922819750185));
#42183=CARTESIAN_POINT('Ctrl Pts',(2.78384588958965,1.,3.13922819750185));
#42184=CARTESIAN_POINT('Ctrl Pts',(2.78260859420629,-1.,3.1346796583452));
#42185=CARTESIAN_POINT('Ctrl Pts',(2.78260859420629,1.,3.1346796583452));
#42186=CARTESIAN_POINT('Ctrl Pts',(2.78094085162947,-1.,3.12862530320194));
#42187=CARTESIAN_POINT('Ctrl Pts',(2.78094085162947,1.,3.12862530320194));
#42188=CARTESIAN_POINT('Ctrl Pts',(2.77882610147986,-1.,3.12107467038623));
#42189=CARTESIAN_POINT('Ctrl Pts',(2.77882610147986,1.,3.12107467038623));
#42190=CARTESIAN_POINT('Ctrl Pts',(2.77668121003225,-1.,3.11354142304692));
#42191=CARTESIAN_POINT('Ctrl Pts',(2.77668121003225,1.,3.11354142304692));
#42192=CARTESIAN_POINT('Ctrl Pts',(2.7745060912343,-1.,3.10602568032641));
#42193=CARTESIAN_POINT('Ctrl Pts',(2.7745060912343,1.,3.10602568032641));
#42194=CARTESIAN_POINT('Ctrl Pts',(2.77230064795679,-1.,3.09852761277432));
#42195=CARTESIAN_POINT('Ctrl Pts',(2.77230064795679,1.,3.09852761277432));
#42196=CARTESIAN_POINT('Ctrl Pts',(2.77006478033937,-1.,3.09104745381882));
#42197=CARTESIAN_POINT('Ctrl Pts',(2.77006478033937,1.,3.09104745381882));
#42198=CARTESIAN_POINT('Ctrl Pts',(2.76779837828843,-1.,3.08358548000904));
#42199=CARTESIAN_POINT('Ctrl Pts',(2.76779837828843,1.,3.08358548000904));
#42200=CARTESIAN_POINT('Ctrl Pts',(2.76550131064522,-1.,3.07614198408488));
#42201=CARTESIAN_POINT('Ctrl Pts',(2.76550131064522,1.,3.07614198408488));
#42202=CARTESIAN_POINT('Ctrl Pts',(2.76317341453415,-1.,3.06871724843121));
#42203=CARTESIAN_POINT('Ctrl Pts',(2.76317341453415,1.,3.06871724843121));
#42204=CARTESIAN_POINT('Ctrl Pts',(2.76081448760011,-1.,3.06131152247599));
#42205=CARTESIAN_POINT('Ctrl Pts',(2.76081448760011,1.,3.06131152247599));
#42206=CARTESIAN_POINT('Ctrl Pts',(2.75842427253164,-1.,3.05392498750112));
#42207=CARTESIAN_POINT('Ctrl Pts',(2.75842427253164,1.,3.05392498750112));
#42208=CARTESIAN_POINT('Ctrl Pts',(2.7560024745616,-1.,3.04655777351333));
#42209=CARTESIAN_POINT('Ctrl Pts',(2.7560024745616,1.,3.04655777351333));
#42210=CARTESIAN_POINT('Ctrl Pts',(2.75354880060473,-1.,3.03921001108158));
#42211=CARTESIAN_POINT('Ctrl Pts',(2.75354880060473,1.,3.03921001108158));
#42212=CARTESIAN_POINT('Ctrl Pts',(2.75106299523032,-1.,3.03188187589168));
#42213=CARTESIAN_POINT('Ctrl Pts',(2.75106299523032,1.,3.03188187589168));
#42214=CARTESIAN_POINT('Ctrl Pts',(2.74854487184099,-1.,3.02457362909199));
#42215=CARTESIAN_POINT('Ctrl Pts',(2.74854487184099,1.,3.02457362909199));
#42216=CARTESIAN_POINT('Ctrl Pts',(2.74599436193528,-1.,3.01728567646502));
#42217=CARTESIAN_POINT('Ctrl Pts',(2.74599436193528,1.,3.01728567646502));
#42218=CARTESIAN_POINT('Ctrl Pts',(2.7434115023978,-1.,3.01001855960041));
#42219=CARTESIAN_POINT('Ctrl Pts',(2.7434115023978,1.,3.01001855960041));
#42220=CARTESIAN_POINT('Ctrl Pts',(2.74079632883852,-1.,3.00277284351431));
#42221=CARTESIAN_POINT('Ctrl Pts',(2.74079632883852,1.,3.00277284351431));
#42222=CARTESIAN_POINT('Ctrl Pts',(2.73814878711609,-1.,2.99554902409741));
#42223=CARTESIAN_POINT('Ctrl Pts',(2.73814878711609,1.,2.99554902409741));
#42224=CARTESIAN_POINT('Ctrl Pts',(2.73546864694548,-1.,2.98834743696455));
#42225=CARTESIAN_POINT('Ctrl Pts',(2.73546864694548,1.,2.98834743696455));
#42226=CARTESIAN_POINT('Ctrl Pts',(2.73275539286537,-1.,2.98116814232175));
#42227=CARTESIAN_POINT('Ctrl Pts',(2.73275539286537,1.,2.98116814232175));
#42228=CARTESIAN_POINT('Ctrl Pts',(2.7300081921846,-1.,2.97401089032729));
#42229=CARTESIAN_POINT('Ctrl Pts',(2.7300081921846,1.,2.97401089032729));
#42230=CARTESIAN_POINT('Ctrl Pts',(2.72722614084112,-1.,2.96687537842492));
#42231=CARTESIAN_POINT('Ctrl Pts',(2.72722614084112,1.,2.96687537842492));
#42232=CARTESIAN_POINT('Ctrl Pts',(2.72440846811745,-1.,2.95976146492595));
#42233=CARTESIAN_POINT('Ctrl Pts',(2.72440846811745,1.,2.95976146492595));
#42234=CARTESIAN_POINT('Ctrl Pts',(2.72155475123361,-1.,2.95266939280617));
#42235=CARTESIAN_POINT('Ctrl Pts',(2.72155475123361,1.,2.95266939280617));
#42236=CARTESIAN_POINT('Ctrl Pts',(2.71866514227951,-1.,2.94560002559789));
#42237=CARTESIAN_POINT('Ctrl Pts',(2.71866514227951,1.,2.94560002559789));
#42238=CARTESIAN_POINT('Ctrl Pts',(2.71574054592575,-1.,2.93855503247248));
#42239=CARTESIAN_POINT('Ctrl Pts',(2.71574054592575,1.,2.93855503247248));
#42240=CARTESIAN_POINT('Ctrl Pts',(2.71278207520807,-1.,2.93153633192583));
#42241=CARTESIAN_POINT('Ctrl Pts',(2.71278207520807,1.,2.93153633192583));
#42242=CARTESIAN_POINT('Ctrl Pts',(2.70979055994751,-1.,2.92454558914774));
#42243=CARTESIAN_POINT('Ctrl Pts',(2.70979055994751,1.,2.92454558914774));
#42244=CARTESIAN_POINT('Ctrl Pts',(2.70676602302518,-1.,2.91758367994738));
#42245=CARTESIAN_POINT('Ctrl Pts',(2.70676602302518,1.,2.91758367994738));
#42246=CARTESIAN_POINT('Ctrl Pts',(2.70370719782114,-1.,2.91065019668331));
#42247=CARTESIAN_POINT('Ctrl Pts',(2.70370719782114,1.,2.91065019668331));
#42248=CARTESIAN_POINT('Ctrl Pts',(2.70061095078692,-1.,2.90374285605839));
#42249=CARTESIAN_POINT('Ctrl Pts',(2.70061095078692,1.,2.90374285605839));
#42250=CARTESIAN_POINT('Ctrl Pts',(2.69747340630621,-1.,2.89685866123668));
#42251=CARTESIAN_POINT('Ctrl Pts',(2.69747340630621,1.,2.89685866123668));
#42252=CARTESIAN_POINT('Ctrl Pts',(2.69429113011369,-1.,2.88999512410304));
#42253=CARTESIAN_POINT('Ctrl Pts',(2.69429113011369,1.,2.88999512410304));
#42254=CARTESIAN_POINT('Ctrl Pts',(2.69106236420196,-1.,2.88315153980464));
#42255=CARTESIAN_POINT('Ctrl Pts',(2.69106236420196,1.,2.88315153980464));
#42256=CARTESIAN_POINT('Ctrl Pts',(2.68778807801691,-1.,2.87633007243885));
#42257=CARTESIAN_POINT('Ctrl Pts',(2.68778807801691,1.,2.87633007243885));
#42258=CARTESIAN_POINT('Ctrl Pts',(2.6844735313961,-1.,2.8695373654725));
#42259=CARTESIAN_POINT('Ctrl Pts',(2.6844735313961,1.,2.8695373654725));
#42260=CARTESIAN_POINT('Ctrl Pts',(2.68112602796323,-1.,2.86278224277705));
#42261=CARTESIAN_POINT('Ctrl Pts',(2.68112602796323,1.,2.86278224277705));
#42262=CARTESIAN_POINT('Ctrl Pts',(2.67775201955736,-1.,2.85607274378031));
#42263=CARTESIAN_POINT('Ctrl Pts',(2.67775201955736,1.,2.85607274378031));
#42264=CARTESIAN_POINT('Ctrl Pts',(2.67435421039682,-1.,2.84941315703096));
#42265=CARTESIAN_POINT('Ctrl Pts',(2.67435421039682,1.,2.84941315703096));
#42266=CARTESIAN_POINT('Ctrl Pts',(2.67092916452116,-1.,2.84280157191314));
#42267=CARTESIAN_POINT('Ctrl Pts',(2.67092916452116,1.,2.84280157191314));
#42268=CARTESIAN_POINT('Ctrl Pts',(2.66746339678085,-1.,2.8362258685396));
#42269=CARTESIAN_POINT('Ctrl Pts',(2.66746339678085,1.,2.8362258685396));
#42270=CARTESIAN_POINT('Ctrl Pts',(2.66393764726902,-1.,2.82966813308969));
#42271=CARTESIAN_POINT('Ctrl Pts',(2.66393764726902,1.,2.82966813308969));
#42272=CARTESIAN_POINT('Ctrl Pts',(2.66033388273437,-1.,2.82311188135053));
#42273=CARTESIAN_POINT('Ctrl Pts',(2.66033388273437,1.,2.82311188135053));
#42274=CARTESIAN_POINT('Ctrl Pts',(2.65664198781335,-1.,2.81654896073874));
#42275=CARTESIAN_POINT('Ctrl Pts',(2.65664198781335,1.,2.81654896073874));
#42276=CARTESIAN_POINT('Ctrl Pts',(2.65286529532221,-1.,2.80998526078179));
#42277=CARTESIAN_POINT('Ctrl Pts',(2.65286529532221,1.,2.80998526078179));
#42278=CARTESIAN_POINT('Ctrl Pts',(2.64902988983373,-1.,2.80345029781191));
#42279=CARTESIAN_POINT('Ctrl Pts',(2.64902988983373,1.,2.80345029781191));
#42280=CARTESIAN_POINT('Ctrl Pts',(2.6451766779937,-1.,2.7969891067079));
#42281=CARTESIAN_POINT('Ctrl Pts',(2.6451766779937,1.,2.7969891067079));
#42282=CARTESIAN_POINT('Ctrl Pts',(2.64134450532632,-1.,2.79064495573275));
#42283=CARTESIAN_POINT('Ctrl Pts',(2.64134450532632,1.,2.79064495573275));
#42284=CARTESIAN_POINT('Ctrl Pts',(2.63755471430322,-1.,2.78444351041594));
#42285=CARTESIAN_POINT('Ctrl Pts',(2.63755471430322,1.,2.78444351041594));
#42286=CARTESIAN_POINT('Ctrl Pts',(2.63379800904575,-1.,2.77837943466423));
#42287=CARTESIAN_POINT('Ctrl Pts',(2.63379800904575,1.,2.77837943466423));
#42288=CARTESIAN_POINT('Ctrl Pts',(2.63001305229548,-1.,2.77239433377839));
#42289=CARTESIAN_POINT('Ctrl Pts',(2.63001305229548,1.,2.77239433377839));
#42290=CARTESIAN_POINT('Ctrl Pts',(2.6260995650624,-1.,2.76639078478898));
#42291=CARTESIAN_POINT('Ctrl Pts',(2.6260995650624,1.,2.76639078478898));
#42292=CARTESIAN_POINT('Ctrl Pts',(2.62195665834491,-1.,2.76027271596564));
#42293=CARTESIAN_POINT('Ctrl Pts',(2.62195665834491,1.,2.76027271596564));
#42294=CARTESIAN_POINT('Ctrl Pts',(2.61751580407608,-1.,2.75398025025967));
#42295=CARTESIAN_POINT('Ctrl Pts',(2.61751580407608,1.,2.75398025025967));
#42296=CARTESIAN_POINT('Ctrl Pts',(2.61277170105864,-1.,2.74752219567307));
#42297=CARTESIAN_POINT('Ctrl Pts',(2.61277170105864,1.,2.74752219567307));
#42298=CARTESIAN_POINT('Ctrl Pts',(2.60782480638629,-1.,2.74102110999284));
#42299=CARTESIAN_POINT('Ctrl Pts',(2.60782480638629,1.,2.74102110999284));
#42300=CARTESIAN_POINT('Ctrl Pts',(2.60287635689,-1.,2.73470730109906));
#42301=CARTESIAN_POINT('Ctrl Pts',(2.60287635689,1.,2.73470730109906));
#42302=CARTESIAN_POINT('Ctrl Pts',(2.5981786903501,-1.,2.72886483481804));
#42303=CARTESIAN_POINT('Ctrl Pts',(2.5981786903501,1.,2.72886483481804));
#42304=CARTESIAN_POINT('Ctrl Pts',(2.59399625537407,-1.,2.72378896977273));
#42305=CARTESIAN_POINT('Ctrl Pts',(2.59399625537407,1.,2.72378896977273));
#42306=CARTESIAN_POINT('Ctrl Pts',(2.59056604771863,-1.,2.7197430895797));
#42307=CARTESIAN_POINT('Ctrl Pts',(2.59056604771863,1.,2.7197430895797));
#42308=CARTESIAN_POINT('Ctrl Pts',(2.58804906785077,-1.,2.71690570241274));
#42309=CARTESIAN_POINT('Ctrl Pts',(2.58804906785077,1.,2.71690570241274));
#42310=CARTESIAN_POINT('Ctrl Pts',(2.58682657352212,-1.,2.71566956750046));
#42311=CARTESIAN_POINT('Ctrl Pts',(2.58682657352212,1.,2.71566956750046));
#42312=CARTESIAN_POINT('Ctrl Pts',(2.58636629903847,-1.,2.71533674140979));
#42313=CARTESIAN_POINT('Ctrl Pts',(2.58636629903847,1.,2.71533674140979));
#42314=CARTESIAN_POINT('Ctrl Pts',(2.58626222935706,-1.,2.71537879705));
#42315=CARTESIAN_POINT('Ctrl Pts',(2.58626222935706,1.,2.71537879705));
#42316=CARTESIAN_POINT('Ctrl Pts',(2.58626089374824,-1.,2.71546581445404));
#42317=CARTESIAN_POINT('Ctrl Pts',(2.58626089374824,1.,2.71546581445404));
#42318=CARTESIAN_POINT('',(2.78507268004355,1.,3.14378277984898));
#42319=CARTESIAN_POINT('Ctrl Pts',(2.78507268004355,1.,3.14378277984898));
#42320=CARTESIAN_POINT('Ctrl Pts',(2.78466475036183,1.,3.14226401019149));
#42321=CARTESIAN_POINT('Ctrl Pts',(2.78384588958965,1.,3.13922819750185));
#42322=CARTESIAN_POINT('Ctrl Pts',(2.78260859420629,1.,3.1346796583452));
#42323=CARTESIAN_POINT('Ctrl Pts',(2.78094085162947,1.,3.12862530320194));
#42324=CARTESIAN_POINT('Ctrl Pts',(2.77882610147986,1.,3.12107467038623));
#42325=CARTESIAN_POINT('Ctrl Pts',(2.77668121003225,1.,3.11354142304692));
#42326=CARTESIAN_POINT('Ctrl Pts',(2.7745060912343,1.,3.10602568032641));
#42327=CARTESIAN_POINT('Ctrl Pts',(2.77230064795679,1.,3.09852761277432));
#42328=CARTESIAN_POINT('Ctrl Pts',(2.77006478033937,1.,3.09104745381882));
#42329=CARTESIAN_POINT('Ctrl Pts',(2.76779837828843,1.,3.08358548000904));
#42330=CARTESIAN_POINT('Ctrl Pts',(2.76550131064522,1.,3.07614198408488));
#42331=CARTESIAN_POINT('Ctrl Pts',(2.76317341453415,1.,3.06871724843121));
#42332=CARTESIAN_POINT('Ctrl Pts',(2.76081448760011,1.,3.06131152247599));
#42333=CARTESIAN_POINT('Ctrl Pts',(2.75842427253164,1.,3.05392498750112));
#42334=CARTESIAN_POINT('Ctrl Pts',(2.7560024745616,1.,3.04655777351333));
#42335=CARTESIAN_POINT('Ctrl Pts',(2.75354880060473,1.,3.03921001108158));
#42336=CARTESIAN_POINT('Ctrl Pts',(2.75106299523032,1.,3.03188187589168));
#42337=CARTESIAN_POINT('Ctrl Pts',(2.74854487184099,1.,3.02457362909199));
#42338=CARTESIAN_POINT('Ctrl Pts',(2.74599436193528,1.,3.01728567646502));
#42339=CARTESIAN_POINT('Ctrl Pts',(2.7434115023978,1.,3.01001855960041));
#42340=CARTESIAN_POINT('Ctrl Pts',(2.74079632883852,1.,3.00277284351431));
#42341=CARTESIAN_POINT('Ctrl Pts',(2.73814878711609,1.,2.99554902409741));
#42342=CARTESIAN_POINT('Ctrl Pts',(2.73546864694548,1.,2.98834743696455));
#42343=CARTESIAN_POINT('Ctrl Pts',(2.73275539286537,1.,2.98116814232175));
#42344=CARTESIAN_POINT('Ctrl Pts',(2.7300081921846,1.,2.97401089032729));
#42345=CARTESIAN_POINT('Ctrl Pts',(2.72722614084112,1.,2.96687537842492));
#42346=CARTESIAN_POINT('Ctrl Pts',(2.72440846811745,1.,2.95976146492595));
#42347=CARTESIAN_POINT('Ctrl Pts',(2.72155475123361,1.,2.95266939280617));
#42348=CARTESIAN_POINT('Ctrl Pts',(2.71866514227951,1.,2.94560002559789));
#42349=CARTESIAN_POINT('Ctrl Pts',(2.71574054592575,1.,2.93855503247248));
#42350=CARTESIAN_POINT('Ctrl Pts',(2.71278207520807,1.,2.93153633192583));
#42351=CARTESIAN_POINT('Ctrl Pts',(2.70979055994751,1.,2.92454558914774));
#42352=CARTESIAN_POINT('Ctrl Pts',(2.70676602302518,1.,2.91758367994738));
#42353=CARTESIAN_POINT('Ctrl Pts',(2.70370719782114,1.,2.91065019668331));
#42354=CARTESIAN_POINT('Ctrl Pts',(2.70061095078692,1.,2.90374285605839));
#42355=CARTESIAN_POINT('Ctrl Pts',(2.69747340630621,1.,2.89685866123668));
#42356=CARTESIAN_POINT('Ctrl Pts',(2.69429113011369,1.,2.88999512410304));
#42357=CARTESIAN_POINT('Ctrl Pts',(2.69106236420196,1.,2.88315153980464));
#42358=CARTESIAN_POINT('Ctrl Pts',(2.68778807801691,1.,2.87633007243885));
#42359=CARTESIAN_POINT('Ctrl Pts',(2.6844735313961,1.,2.8695373654725));
#42360=CARTESIAN_POINT('Ctrl Pts',(2.68112602796323,1.,2.86278224277705));
#42361=CARTESIAN_POINT('Ctrl Pts',(2.67775201955736,1.,2.85607274378031));
#42362=CARTESIAN_POINT('Ctrl Pts',(2.67435421039682,1.,2.84941315703096));
#42363=CARTESIAN_POINT('Ctrl Pts',(2.67092916452116,1.,2.84280157191314));
#42364=CARTESIAN_POINT('Ctrl Pts',(2.66746339678085,1.,2.8362258685396));
#42365=CARTESIAN_POINT('Ctrl Pts',(2.66393764726902,1.,2.82966813308969));
#42366=CARTESIAN_POINT('Ctrl Pts',(2.66033388273437,1.,2.82311188135053));
#42367=CARTESIAN_POINT('Ctrl Pts',(2.65664198781335,1.,2.81654896073874));
#42368=CARTESIAN_POINT('Ctrl Pts',(2.65286529532221,1.,2.80998526078179));
#42369=CARTESIAN_POINT('Ctrl Pts',(2.64902988983373,1.,2.80345029781191));
#42370=CARTESIAN_POINT('Ctrl Pts',(2.6451766779937,1.,2.7969891067079));
#42371=CARTESIAN_POINT('Ctrl Pts',(2.64134450532632,1.,2.79064495573275));
#42372=CARTESIAN_POINT('Ctrl Pts',(2.63755471430322,1.,2.78444351041594));
#42373=CARTESIAN_POINT('Ctrl Pts',(2.63379800904575,1.,2.77837943466423));
#42374=CARTESIAN_POINT('Ctrl Pts',(2.63001305229548,1.,2.77239433377839));
#42375=CARTESIAN_POINT('Ctrl Pts',(2.6260995650624,1.,2.76639078478898));
#42376=CARTESIAN_POINT('Ctrl Pts',(2.62195665834491,1.,2.76027271596564));
#42377=CARTESIAN_POINT('Ctrl Pts',(2.61751580407608,1.,2.75398025025967));
#42378=CARTESIAN_POINT('Ctrl Pts',(2.61277170105864,1.,2.74752219567307));
#42379=CARTESIAN_POINT('Ctrl Pts',(2.60782480638629,1.,2.74102110999284));
#42380=CARTESIAN_POINT('Ctrl Pts',(2.60287635689,1.,2.73470730109906));
#42381=CARTESIAN_POINT('Ctrl Pts',(2.5981786903501,1.,2.72886483481804));
#42382=CARTESIAN_POINT('Ctrl Pts',(2.59399625537407,1.,2.72378896977273));
#42383=CARTESIAN_POINT('Ctrl Pts',(2.59056604771863,1.,2.7197430895797));
#42384=CARTESIAN_POINT('Ctrl Pts',(2.58823792682724,1.,2.71711860281891));
#42385=CARTESIAN_POINT('Ctrl Pts',(2.58706285424469,1.,2.71591054189884));
#42386=CARTESIAN_POINT('Ctrl Pts',(2.58656037976884,1.,2.71548946460616));
#42387=CARTESIAN_POINT('Ctrl Pts',(2.58638312917291,1.,2.71540296615967));
#42388=CARTESIAN_POINT('Ctrl Pts',(2.58633475775051,1.,2.71539546306824));
#42389=CARTESIAN_POINT('',(2.78507268004355,0.,3.14378277984898));
#42390=CARTESIAN_POINT('Ctrl Pts',(2.27745358485296,-1.,2.97921217251145));
#42391=CARTESIAN_POINT('Ctrl Pts',(2.27745358485296,1.,2.97921217251145));
#42392=CARTESIAN_POINT('Ctrl Pts',(2.27736742984319,-1.,2.97919987915679));
#42393=CARTESIAN_POINT('Ctrl Pts',(2.27736742984319,1.,2.97919987915679));
#42394=CARTESIAN_POINT('Ctrl Pts',(2.2773096118942,-1.,2.97929608861798));
#42395=CARTESIAN_POINT('Ctrl Pts',(2.2773096118942,1.,2.97929608861798));
#42396=CARTESIAN_POINT('Ctrl Pts',(2.27756633755188,-1.,2.97980276183181));
#42397=CARTESIAN_POINT('Ctrl Pts',(2.27756633755188,1.,2.97980276183181));
#42398=CARTESIAN_POINT('Ctrl Pts',(2.27859601334547,-1.,2.98120357932994));
#42399=CARTESIAN_POINT('Ctrl Pts',(2.27859601334547,1.,2.98120357932994));
#42400=CARTESIAN_POINT('Ctrl Pts',(2.28100472516679,-1.,2.98413343613983));
#42401=CARTESIAN_POINT('Ctrl Pts',(2.28100472516679,1.,2.98413343613983));
#42402=CARTESIAN_POINT('Ctrl Pts',(2.28446419115919,-1.,2.9881543273478));
#42403=CARTESIAN_POINT('Ctrl Pts',(2.28446419115919,1.,2.9881543273478));
#42404=CARTESIAN_POINT('Ctrl Pts',(2.28882328690362,-1.,2.99307930984034));
#42405=CARTESIAN_POINT('Ctrl Pts',(2.28882328690362,1.,2.99307930984034));
#42406=CARTESIAN_POINT('Ctrl Pts',(2.29385894577754,-1.,2.99863310339691));
#42407=CARTESIAN_POINT('Ctrl Pts',(2.29385894577754,1.,2.99863310339691));
#42408=CARTESIAN_POINT('Ctrl Pts',(2.29932091315775,-1.,3.00450832658613));
#42409=CARTESIAN_POINT('Ctrl Pts',(2.29932091315775,1.,3.00450832658613));
#42410=CARTESIAN_POINT('Ctrl Pts',(2.30496809486482,-1.,3.01041131063823));
#42411=CARTESIAN_POINT('Ctrl Pts',(2.30496809486482,1.,3.01041131063823));
#42412=CARTESIAN_POINT('Ctrl Pts',(2.31060449886629,-1.,3.01610726819086));
#42413=CARTESIAN_POINT('Ctrl Pts',(2.31060449886629,1.,3.01610726819086));
#42414=CARTESIAN_POINT('Ctrl Pts',(2.31612479121631,-1.,3.02147780668161));
#42415=CARTESIAN_POINT('Ctrl Pts',(2.31612479121631,1.,3.02147780668161));
#42416=CARTESIAN_POINT('Ctrl Pts',(2.32151944306402,-1.,3.02652678416611));
#42417=CARTESIAN_POINT('Ctrl Pts',(2.32151944306402,1.,3.02652678416611));
#42418=CARTESIAN_POINT('Ctrl Pts',(2.32683687412096,-1.,3.03133125185136));
#42419=CARTESIAN_POINT('Ctrl Pts',(2.32683687412096,1.,3.03133125185136));
#42420=CARTESIAN_POINT('Ctrl Pts',(2.33215619079829,-1.,3.03600588555793));
#42421=CARTESIAN_POINT('Ctrl Pts',(2.33215619079829,1.,3.03600588555793));
#42422=CARTESIAN_POINT('Ctrl Pts',(2.33755792953706,-1.,3.04066496998544));
#42423=CARTESIAN_POINT('Ctrl Pts',(2.33755792953706,1.,3.04066496998544));
#42424=CARTESIAN_POINT('Ctrl Pts',(2.34309017083976,-1.,3.04537822217256));
#42425=CARTESIAN_POINT('Ctrl Pts',(2.34309017083976,1.,3.04537822217256));
#42426=CARTESIAN_POINT('Ctrl Pts',(2.3487567309077,-1.,3.05015565829918));
#42427=CARTESIAN_POINT('Ctrl Pts',(2.3487567309077,1.,3.05015565829918));
#42428=CARTESIAN_POINT('Ctrl Pts',(2.35453559889474,-1.,3.05497218368146));
#42429=CARTESIAN_POINT('Ctrl Pts',(2.35453559889474,1.,3.05497218368146));
#42430=CARTESIAN_POINT('Ctrl Pts',(2.36039011602072,-1.,3.0597826624004));
#42431=CARTESIAN_POINT('Ctrl Pts',(2.36039011602072,1.,3.0597826624004));
#42432=CARTESIAN_POINT('Ctrl Pts',(2.36628220107009,-1.,3.06453964643162));
#42433=CARTESIAN_POINT('Ctrl Pts',(2.36628220107009,1.,3.06453964643162));
#42434=CARTESIAN_POINT('Ctrl Pts',(2.37218678163178,-1.,3.069212754975));
#42435=CARTESIAN_POINT('Ctrl Pts',(2.37218678163178,1.,3.069212754975));
#42436=CARTESIAN_POINT('Ctrl Pts',(2.37809856205548,-1.,3.07379777492165));
#42437=CARTESIAN_POINT('Ctrl Pts',(2.37809856205548,1.,3.07379777492165));
#42438=CARTESIAN_POINT('Ctrl Pts',(2.38402401216126,-1.,3.07830597244326));
#42439=CARTESIAN_POINT('Ctrl Pts',(2.38402401216126,1.,3.07830597244326));
#42440=CARTESIAN_POINT('Ctrl Pts',(2.38997659219199,-1.,3.08275773747093));
#42441=CARTESIAN_POINT('Ctrl Pts',(2.38997659219199,1.,3.08275773747093));
#42442=CARTESIAN_POINT('Ctrl Pts',(2.39597098250631,-1.,3.08717489512914));
#42443=CARTESIAN_POINT('Ctrl Pts',(2.39597098250631,1.,3.08717489512914));
#42444=CARTESIAN_POINT('Ctrl Pts',(2.40201704423341,-1.,3.091572660511));
#42445=CARTESIAN_POINT('Ctrl Pts',(2.40201704423341,1.,3.091572660511));
#42446=CARTESIAN_POINT('Ctrl Pts',(2.40811612696369,-1.,3.09595472616076));
#42447=CARTESIAN_POINT('Ctrl Pts',(2.40811612696369,1.,3.09595472616076));
#42448=CARTESIAN_POINT('Ctrl Pts',(2.41426441798057,-1.,3.1003177502767));
#42449=CARTESIAN_POINT('Ctrl Pts',(2.41426441798057,1.,3.1003177502767));
#42450=CARTESIAN_POINT('Ctrl Pts',(2.42045498612489,-1.,3.10465410280896));
#42451=CARTESIAN_POINT('Ctrl Pts',(2.42045498612489,1.,3.10465410280896));
#42452=CARTESIAN_POINT('Ctrl Pts',(2.42668025870015,-1.,3.10895518969595));
#42453=CARTESIAN_POINT('Ctrl Pts',(2.42668025870015,1.,3.10895518969595));
#42454=CARTESIAN_POINT('Ctrl Pts',(2.43293449685144,-1.,3.11321477659018));
#42455=CARTESIAN_POINT('Ctrl Pts',(2.43293449685144,1.,3.11321477659018));
#42456=CARTESIAN_POINT('Ctrl Pts',(2.43921571477977,-1.,3.11743156744186));
#42457=CARTESIAN_POINT('Ctrl Pts',(2.43921571477977,1.,3.11743156744186));
#42458=CARTESIAN_POINT('Ctrl Pts',(2.44552433364715,-1.,3.12160740887768));
#42459=CARTESIAN_POINT('Ctrl Pts',(2.44552433364715,1.,3.12160740887768));
#42460=CARTESIAN_POINT('Ctrl Pts',(2.45186227369846,-1.,3.12574608210847));
#42461=CARTESIAN_POINT('Ctrl Pts',(2.45186227369846,1.,3.12574608210847));
#42462=CARTESIAN_POINT('Ctrl Pts',(2.45823188859366,-1.,3.12985188384371));
#42463=CARTESIAN_POINT('Ctrl Pts',(2.45823188859366,1.,3.12985188384371));
#42464=CARTESIAN_POINT('Ctrl Pts',(2.46463494332374,-1.,3.13392826623906));
#42465=CARTESIAN_POINT('Ctrl Pts',(2.46463494332374,1.,3.13392826623906));
#42466=CARTESIAN_POINT('Ctrl Pts',(2.47107164236838,-1.,3.13797654408943));
#42467=CARTESIAN_POINT('Ctrl Pts',(2.47107164236838,1.,3.13797654408943));
#42468=CARTESIAN_POINT('Ctrl Pts',(2.47754112428043,-1.,3.14199655778863));
#42469=CARTESIAN_POINT('Ctrl Pts',(2.47754112428043,1.,3.14199655778863));
#42470=CARTESIAN_POINT('Ctrl Pts',(2.4840418741839,-1.,3.14598722723896));
#42471=CARTESIAN_POINT('Ctrl Pts',(2.4840418741839,1.,3.14598722723896));
#42472=CARTESIAN_POINT('Ctrl Pts',(2.49057217131988,-1.,3.14994715298907));
#42473=CARTESIAN_POINT('Ctrl Pts',(2.49057217131988,1.,3.14994715298907));
#42474=CARTESIAN_POINT('Ctrl Pts',(2.49713050858896,-1.,3.15387518039046));
#42475=CARTESIAN_POINT('Ctrl Pts',(2.49713050858896,1.,3.15387518039046));
#42476=CARTESIAN_POINT('Ctrl Pts',(2.50371605688252,-1.,3.15777102413957));
#42477=CARTESIAN_POINT('Ctrl Pts',(2.50371605688252,1.,3.15777102413957));
#42478=CARTESIAN_POINT('Ctrl Pts',(2.51032851007894,-1.,3.16163506380157));
#42479=CARTESIAN_POINT('Ctrl Pts',(2.51032851007894,1.,3.16163506380157));
#42480=CARTESIAN_POINT('Ctrl Pts',(2.51696788755577,-1.,3.16546808277023));
#42481=CARTESIAN_POINT('Ctrl Pts',(2.51696788755577,1.,3.16546808277023));
#42482=CARTESIAN_POINT('Ctrl Pts',(2.52363434671788,-1.,3.16927102130736));
#42483=CARTESIAN_POINT('Ctrl Pts',(2.52363434671788,1.,3.16927102130736));
#42484=CARTESIAN_POINT('Ctrl Pts',(2.53032800406941,-1.,3.17304474093612));
#42485=CARTESIAN_POINT('Ctrl Pts',(2.53032800406941,1.,3.17304474093612));
#42486=CARTESIAN_POINT('Ctrl Pts',(2.53704871950948,-1.,3.17678974135318));
#42487=CARTESIAN_POINT('Ctrl Pts',(2.53704871950948,1.,3.17678974135318));
#42488=CARTESIAN_POINT('Ctrl Pts',(2.5437961255305,-1.,3.1805061975064));
#42489=CARTESIAN_POINT('Ctrl Pts',(2.5437961255305,1.,3.1805061975064));
#42490=CARTESIAN_POINT('Ctrl Pts',(2.5505697238773,-1.,3.18419408529594));
#42491=CARTESIAN_POINT('Ctrl Pts',(2.5505697238773,1.,3.18419408529594));
#42492=CARTESIAN_POINT('Ctrl Pts',(2.55736896206056,-1.,3.18785328116218));
#42493=CARTESIAN_POINT('Ctrl Pts',(2.55736896206056,1.,3.18785328116218));
#42494=CARTESIAN_POINT('Ctrl Pts',(2.56419331092858,-1.,3.19148366395139));
#42495=CARTESIAN_POINT('Ctrl Pts',(2.56419331092858,1.,3.19148366395139));
#42496=CARTESIAN_POINT('Ctrl Pts',(2.57104235897899,-1.,3.19508523784363));
#42497=CARTESIAN_POINT('Ctrl Pts',(2.57104235897899,1.,3.19508523784363));
#42498=CARTESIAN_POINT('Ctrl Pts',(2.57791581908874,-1.,3.19865814628682));
#42499=CARTESIAN_POINT('Ctrl Pts',(2.57791581908874,1.,3.19865814628682));
#42500=CARTESIAN_POINT('Ctrl Pts',(2.58481347777728,-1.,3.20220261408414));
#42501=CARTESIAN_POINT('Ctrl Pts',(2.58481347777728,1.,3.20220261408414));
#42502=CARTESIAN_POINT('Ctrl Pts',(2.59173516023481,-1.,3.2057189102873));
#42503=CARTESIAN_POINT('Ctrl Pts',(2.59173516023481,1.,3.2057189102873));
#42504=CARTESIAN_POINT('Ctrl Pts',(2.59868069194341,-1.,3.20920730569681));
#42505=CARTESIAN_POINT('Ctrl Pts',(2.59868069194341,1.,3.20920730569681));
#42506=CARTESIAN_POINT('Ctrl Pts',(2.60564985360017,-1.,3.21266802609682));
#42507=CARTESIAN_POINT('Ctrl Pts',(2.60564985360017,1.,3.21266802609682));
#42508=CARTESIAN_POINT('Ctrl Pts',(2.61264236719171,-1.,3.21610123233082));
#42509=CARTESIAN_POINT('Ctrl Pts',(2.61264236719171,1.,3.21610123233082));
#42510=CARTESIAN_POINT('Ctrl Pts',(2.61965792832947,-1.,3.21950704109321));
#42511=CARTESIAN_POINT('Ctrl Pts',(2.61965792832947,1.,3.21950704109321));
#42512=CARTESIAN_POINT('Ctrl Pts',(2.62669622735912,-1.,3.2228855361324));
#42513=CARTESIAN_POINT('Ctrl Pts',(2.62669622735912,1.,3.2228855361324));
#42514=CARTESIAN_POINT('Ctrl Pts',(2.63375697391372,-1.,3.2262367829246));
#42515=CARTESIAN_POINT('Ctrl Pts',(2.63375697391372,1.,3.2262367829246));
#42516=CARTESIAN_POINT('Ctrl Pts',(2.64083992181823,-1.,3.22956084358547));
#42517=CARTESIAN_POINT('Ctrl Pts',(2.64083992181823,1.,3.22956084358547));
#42518=CARTESIAN_POINT('Ctrl Pts',(2.64794488743038,-1.,3.23285778737096));
#42519=CARTESIAN_POINT('Ctrl Pts',(2.64794488743038,1.,3.23285778737096));
#42520=CARTESIAN_POINT('Ctrl Pts',(2.65507173961555,-1.,3.236127680639));
#42521=CARTESIAN_POINT('Ctrl Pts',(2.65507173961555,1.,3.236127680639));
#42522=CARTESIAN_POINT('Ctrl Pts',(2.6607906631847,-1.,3.23872200034785));
#42523=CARTESIAN_POINT('Ctrl Pts',(2.6607906631847,1.,3.23872200034785));
#42524=CARTESIAN_POINT('Ctrl Pts',(2.66508964663997,-1.,3.24065561086749));
#42525=CARTESIAN_POINT('Ctrl Pts',(2.66508964663997,1.,3.24065561086749));
#42526=CARTESIAN_POINT('Ctrl Pts',(2.66795998539579,-1.,3.24193929584471));
#42527=CARTESIAN_POINT('Ctrl Pts',(2.66795998539579,1.,3.24193929584471));
#42528=CARTESIAN_POINT('Ctrl Pts',(2.66939624221984,-1.,3.24257979115744));
#42529=CARTESIAN_POINT('Ctrl Pts',(2.66939624221984,1.,3.24257979115744));
#42530=CARTESIAN_POINT('',(2.27737254473521,1.,2.97927412174279));
#42531=CARTESIAN_POINT('Ctrl Pts',(2.27737254473521,-1.,2.97927412174279));
#42532=CARTESIAN_POINT('Ctrl Pts',(2.27737254473521,-0.666666666666667,
2.97927412174279));
#42533=CARTESIAN_POINT('Ctrl Pts',(2.27737254473521,-0.333333333333333,
2.97927412174279));
#42534=CARTESIAN_POINT('Ctrl Pts',(2.27737254473521,0.333333333333333,2.97927412174279));
#42535=CARTESIAN_POINT('Ctrl Pts',(2.27737254473521,0.666666666666667,2.97927412174279));
#42536=CARTESIAN_POINT('Ctrl Pts',(2.27737254473521,1.,2.97927412174279));
#42537=CARTESIAN_POINT('',(2.66939624221984,1.,3.24257979115744));
#42538=CARTESIAN_POINT('',(2.66939624221984,0.,3.24257979115744));
#42539=CARTESIAN_POINT('Ctrl Pts',(2.27737254473521,1.,2.97927412174279));
#42540=CARTESIAN_POINT('Ctrl Pts',(2.27737238849287,1.,2.97932307137477));
#42541=CARTESIAN_POINT('Ctrl Pts',(2.27743009389684,1.,2.9795116710597));
#42542=CARTESIAN_POINT('Ctrl Pts',(2.27776738270289,1.,2.98007383024208));
#42543=CARTESIAN_POINT('Ctrl Pts',(2.27877674853766,1.,2.9814234180956));
#42544=CARTESIAN_POINT('Ctrl Pts',(2.28100472516679,1.,2.98413343613983));
#42545=CARTESIAN_POINT('Ctrl Pts',(2.28446419115919,1.,2.9881543273478));
#42546=CARTESIAN_POINT('Ctrl Pts',(2.28882328690362,1.,2.99307930984034));
#42547=CARTESIAN_POINT('Ctrl Pts',(2.29385894577754,1.,2.99863310339691));
#42548=CARTESIAN_POINT('Ctrl Pts',(2.29932091315775,1.,3.00450832658613));
#42549=CARTESIAN_POINT('Ctrl Pts',(2.30496809486482,1.,3.01041131063823));
#42550=CARTESIAN_POINT('Ctrl Pts',(2.31060449886629,1.,3.01610726819086));
#42551=CARTESIAN_POINT('Ctrl Pts',(2.31612479121631,1.,3.02147780668161));
#42552=CARTESIAN_POINT('Ctrl Pts',(2.32151944306402,1.,3.02652678416611));
#42553=CARTESIAN_POINT('Ctrl Pts',(2.32683687412096,1.,3.03133125185136));
#42554=CARTESIAN_POINT('Ctrl Pts',(2.33215619079829,1.,3.03600588555793));
#42555=CARTESIAN_POINT('Ctrl Pts',(2.33755792953706,1.,3.04066496998544));
#42556=CARTESIAN_POINT('Ctrl Pts',(2.34309017083976,1.,3.04537822217256));
#42557=CARTESIAN_POINT('Ctrl Pts',(2.3487567309077,1.,3.05015565829918));
#42558=CARTESIAN_POINT('Ctrl Pts',(2.35453559889474,1.,3.05497218368146));
#42559=CARTESIAN_POINT('Ctrl Pts',(2.36039011602072,1.,3.0597826624004));
#42560=CARTESIAN_POINT('Ctrl Pts',(2.36628220107009,1.,3.06453964643162));
#42561=CARTESIAN_POINT('Ctrl Pts',(2.37218678163178,1.,3.069212754975));
#42562=CARTESIAN_POINT('Ctrl Pts',(2.37809856205548,1.,3.07379777492165));
#42563=CARTESIAN_POINT('Ctrl Pts',(2.38402401216126,1.,3.07830597244326));
#42564=CARTESIAN_POINT('Ctrl Pts',(2.38997659219199,1.,3.08275773747093));
#42565=CARTESIAN_POINT('Ctrl Pts',(2.39597098250631,1.,3.08717489512914));
#42566=CARTESIAN_POINT('Ctrl Pts',(2.40201704423341,1.,3.091572660511));
#42567=CARTESIAN_POINT('Ctrl Pts',(2.40811612696369,1.,3.09595472616076));
#42568=CARTESIAN_POINT('Ctrl Pts',(2.41426441798057,1.,3.1003177502767));
#42569=CARTESIAN_POINT('Ctrl Pts',(2.42045498612489,1.,3.10465410280896));
#42570=CARTESIAN_POINT('Ctrl Pts',(2.42668025870015,1.,3.10895518969595));
#42571=CARTESIAN_POINT('Ctrl Pts',(2.43293449685144,1.,3.11321477659018));
#42572=CARTESIAN_POINT('Ctrl Pts',(2.43921571477977,1.,3.11743156744186));
#42573=CARTESIAN_POINT('Ctrl Pts',(2.44552433364715,1.,3.12160740887768));
#42574=CARTESIAN_POINT('Ctrl Pts',(2.45186227369846,1.,3.12574608210847));
#42575=CARTESIAN_POINT('Ctrl Pts',(2.45823188859366,1.,3.12985188384371));
#42576=CARTESIAN_POINT('Ctrl Pts',(2.46463494332374,1.,3.13392826623906));
#42577=CARTESIAN_POINT('Ctrl Pts',(2.47107164236838,1.,3.13797654408943));
#42578=CARTESIAN_POINT('Ctrl Pts',(2.47754112428043,1.,3.14199655778863));
#42579=CARTESIAN_POINT('Ctrl Pts',(2.4840418741839,1.,3.14598722723896));
#42580=CARTESIAN_POINT('Ctrl Pts',(2.49057217131988,1.,3.14994715298907));
#42581=CARTESIAN_POINT('Ctrl Pts',(2.49713050858896,1.,3.15387518039046));
#42582=CARTESIAN_POINT('Ctrl Pts',(2.50371605688252,1.,3.15777102413957));
#42583=CARTESIAN_POINT('Ctrl Pts',(2.51032851007894,1.,3.16163506380157));
#42584=CARTESIAN_POINT('Ctrl Pts',(2.51696788755577,1.,3.16546808277023));
#42585=CARTESIAN_POINT('Ctrl Pts',(2.52363434671788,1.,3.16927102130736));
#42586=CARTESIAN_POINT('Ctrl Pts',(2.53032800406941,1.,3.17304474093612));
#42587=CARTESIAN_POINT('Ctrl Pts',(2.53704871950948,1.,3.17678974135318));
#42588=CARTESIAN_POINT('Ctrl Pts',(2.5437961255305,1.,3.1805061975064));
#42589=CARTESIAN_POINT('Ctrl Pts',(2.5505697238773,1.,3.18419408529594));
#42590=CARTESIAN_POINT('Ctrl Pts',(2.55736896206056,1.,3.18785328116218));
#42591=CARTESIAN_POINT('Ctrl Pts',(2.56419331092858,1.,3.19148366395139));
#42592=CARTESIAN_POINT('Ctrl Pts',(2.57104235897899,1.,3.19508523784363));
#42593=CARTESIAN_POINT('Ctrl Pts',(2.57791581908874,1.,3.19865814628682));
#42594=CARTESIAN_POINT('Ctrl Pts',(2.58481347777728,1.,3.20220261408414));
#42595=CARTESIAN_POINT('Ctrl Pts',(2.59173516023481,1.,3.2057189102873));
#42596=CARTESIAN_POINT('Ctrl Pts',(2.59868069194341,1.,3.20920730569681));
#42597=CARTESIAN_POINT('Ctrl Pts',(2.60564985360017,1.,3.21266802609682));
#42598=CARTESIAN_POINT('Ctrl Pts',(2.61264236719171,1.,3.21610123233082));
#42599=CARTESIAN_POINT('Ctrl Pts',(2.61965792832947,1.,3.21950704109321));
#42600=CARTESIAN_POINT('Ctrl Pts',(2.62669622735912,1.,3.2228855361324));
#42601=CARTESIAN_POINT('Ctrl Pts',(2.63375697391372,1.,3.2262367829246));
#42602=CARTESIAN_POINT('Ctrl Pts',(2.64083992181823,1.,3.22956084358547));
#42603=CARTESIAN_POINT('Ctrl Pts',(2.64794488743038,1.,3.23285778737096));
#42604=CARTESIAN_POINT('Ctrl Pts',(2.65507173961555,1.,3.236127680639));
#42605=CARTESIAN_POINT('Ctrl Pts',(2.6607906631847,1.,3.23872200034785));
#42606=CARTESIAN_POINT('Ctrl Pts',(2.66508964663997,1.,3.24065561086749));
#42607=CARTESIAN_POINT('Ctrl Pts',(2.66795998539579,1.,3.24193929584471));
#42608=CARTESIAN_POINT('Ctrl Pts',(2.66939624221984,1.,3.24257979115744));
#42609=CARTESIAN_POINT('Origin',(2.66939624221984,0.,3.24257979115744));
#42610=CARTESIAN_POINT('',(2.78507268004355,1.,3.14378277984898));
#42611=CARTESIAN_POINT('Origin',(0.,0.,0.));
#42612=CARTESIAN_POINT('',(2.12971124846838,1.,3.08655633322109));
#42613=CARTESIAN_POINT('Origin',(0.,1.,0.));
#42614=CARTESIAN_POINT('Ctrl Pts',(2.12971124846838,1.,3.08655633322109));
#42615=CARTESIAN_POINT('Ctrl Pts',(2.12971124846838,0.666666666666667,3.08655633322109));
#42616=CARTESIAN_POINT('Ctrl Pts',(2.12971124846838,0.333333333333333,3.08655633322109));
#42617=CARTESIAN_POINT('Ctrl Pts',(2.12971124846838,-0.333333333333333,
3.08655633322109));
#42618=CARTESIAN_POINT('Ctrl Pts',(2.12971124846838,-0.666666666666667,
3.08655633322109));
#42619=CARTESIAN_POINT('Ctrl Pts',(2.12971124846838,-1.,3.08655633322109));
#42620=CARTESIAN_POINT('Ctrl Pts',(2.25898783642071,-1.,3.54075895182139));
#42621=CARTESIAN_POINT('Ctrl Pts',(2.25898783642071,1.,3.54075895182139));
#42622=CARTESIAN_POINT('Ctrl Pts',(2.25882251694918,-1.,3.5391950664771));
#42623=CARTESIAN_POINT('Ctrl Pts',(2.25882251694918,1.,3.5391950664771));
#42624=CARTESIAN_POINT('Ctrl Pts',(2.25848864344599,-1.,3.53606853163247));
#42625=CARTESIAN_POINT('Ctrl Pts',(2.25848864344599,1.,3.53606853163247));
#42626=CARTESIAN_POINT('Ctrl Pts',(2.25797812951166,-1.,3.53138243689932));
#42627=CARTESIAN_POINT('Ctrl Pts',(2.25797812951166,1.,3.53138243689932));
#42628=CARTESIAN_POINT('Ctrl Pts',(2.25727802942141,-1.,3.52514172849666));
#42629=CARTESIAN_POINT('Ctrl Pts',(2.25727802942141,1.,3.52514172849666));
#42630=CARTESIAN_POINT('Ctrl Pts',(2.25637049456061,-1.,3.51735323669213));
#42631=CARTESIAN_POINT('Ctrl Pts',(2.25637049456061,1.,3.51735323669213));
#42632=CARTESIAN_POINT('Ctrl Pts',(2.25543046980351,-1.,3.50957720118209));
#42633=CARTESIAN_POINT('Ctrl Pts',(2.25543046980351,1.,3.50957720118209));
#42634=CARTESIAN_POINT('Ctrl Pts',(2.25445785151923,-1.,3.50181372618058));
#42635=CARTESIAN_POINT('Ctrl Pts',(2.25445785151923,1.,3.50181372618058));
#42636=CARTESIAN_POINT('Ctrl Pts',(2.25345251709453,-1.,3.49406296494309));
#42637=CARTESIAN_POINT('Ctrl Pts',(2.25345251709453,1.,3.49406296494309));
#42638=CARTESIAN_POINT('Ctrl Pts',(2.25241433138231,-1.,3.48632513240231));
#42639=CARTESIAN_POINT('Ctrl Pts',(2.25241433138231,1.,3.48632513240231));
#42640=CARTESIAN_POINT('Ctrl Pts',(2.25134314238258,-1.,3.47860048448015));
#42641=CARTESIAN_POINT('Ctrl Pts',(2.25134314238258,1.,3.47860048448015));
#42642=CARTESIAN_POINT('Ctrl Pts',(2.25023877475674,-1.,3.47088928979467));
#42643=CARTESIAN_POINT('Ctrl Pts',(2.25023877475674,1.,3.47088928979467));
#42644=CARTESIAN_POINT('Ctrl Pts',(2.24910102345977,-1.,3.46319180177474));
#42645=CARTESIAN_POINT('Ctrl Pts',(2.24910102345977,1.,3.46319180177474));
#42646=CARTESIAN_POINT('Ctrl Pts',(2.24792964960874,-1.,3.45550823512213));
#42647=CARTESIAN_POINT('Ctrl Pts',(2.24792964960874,1.,3.45550823512213));
#42648=CARTESIAN_POINT('Ctrl Pts',(2.24672437070139,-1.,3.44783872863448));
#42649=CARTESIAN_POINT('Ctrl Pts',(2.24672437070139,1.,3.44783872863448));
#42650=CARTESIAN_POINT('Ctrl Pts',(2.24548487526212,-1.,3.44018336460619));
#42651=CARTESIAN_POINT('Ctrl Pts',(2.24548487526212,1.,3.44018336460619));
#42652=CARTESIAN_POINT('Ctrl Pts',(2.24421085338856,-1.,3.43254222615007));
#42653=CARTESIAN_POINT('Ctrl Pts',(2.24421085338856,1.,3.43254222615007));
#42654=CARTESIAN_POINT('Ctrl Pts',(2.24290202531144,-1.,3.42491544683075));
#42655=CARTESIAN_POINT('Ctrl Pts',(2.24290202531144,1.,3.42491544683075));
#42656=CARTESIAN_POINT('Ctrl Pts',(2.24155816587811,-1.,3.41730325539119));
#42657=CARTESIAN_POINT('Ctrl Pts',(2.24155816587811,1.,3.41730325539119));
#42658=CARTESIAN_POINT('Ctrl Pts',(2.24017914395211,-1.,3.40970604190205));
#42659=CARTESIAN_POINT('Ctrl Pts',(2.24017914395211,1.,3.40970604190205));
#42660=CARTESIAN_POINT('Ctrl Pts',(2.23876491124064,-1.,3.40212434705511));
#42661=CARTESIAN_POINT('Ctrl Pts',(2.23876491124064,1.,3.40212434705511));
#42662=CARTESIAN_POINT('Ctrl Pts',(2.23731541452726,-1.,3.39455873448088));
#42663=CARTESIAN_POINT('Ctrl Pts',(2.23731541452726,1.,3.39455873448088));
#42664=CARTESIAN_POINT('Ctrl Pts',(2.23583052276281,-1.,3.38700968549522));
#42665=CARTESIAN_POINT('Ctrl Pts',(2.23583052276281,1.,3.38700968549522));
#42666=CARTESIAN_POINT('Ctrl Pts',(2.23430995599572,-1.,3.37947749555649));
#42667=CARTESIAN_POINT('Ctrl Pts',(2.23430995599572,1.,3.37947749555649));
#42668=CARTESIAN_POINT('Ctrl Pts',(2.23275319569253,-1.,3.37196214349356));
#42669=CARTESIAN_POINT('Ctrl Pts',(2.23275319569253,1.,3.37196214349356));
#42670=CARTESIAN_POINT('Ctrl Pts',(2.23115945849777,-1.,3.36446325227908));
#42671=CARTESIAN_POINT('Ctrl Pts',(2.23115945849777,1.,3.36446325227908));
#42672=CARTESIAN_POINT('Ctrl Pts',(2.22952789881011,-1.,3.35698038165529));
#42673=CARTESIAN_POINT('Ctrl Pts',(2.22952789881011,1.,3.35698038165529));
#42674=CARTESIAN_POINT('Ctrl Pts',(2.22785777756588,-1.,3.34951327111117));
#42675=CARTESIAN_POINT('Ctrl Pts',(2.22785777756588,1.,3.34951327111117));
#42676=CARTESIAN_POINT('Ctrl Pts',(2.22614863918044,-1.,3.34206209449371));
#42677=CARTESIAN_POINT('Ctrl Pts',(2.22614863918044,1.,3.34206209449371));
#42678=CARTESIAN_POINT('Ctrl Pts',(2.224400498785,-1.,3.3346277284958));
#42679=CARTESIAN_POINT('Ctrl Pts',(2.224400498785,1.,3.3346277284958));
#42680=CARTESIAN_POINT('Ctrl Pts',(2.22261398879623,-1.,3.32721196326019));
#42681=CARTESIAN_POINT('Ctrl Pts',(2.22261398879623,1.,3.32721196326019));
#42682=CARTESIAN_POINT('Ctrl Pts',(2.22078990842768,-1.,3.31981686778008));
#42683=CARTESIAN_POINT('Ctrl Pts',(2.22078990842768,1.,3.31981686778008));
#42684=CARTESIAN_POINT('Ctrl Pts',(2.21892881679083,-1.,3.31244421655662));
#42685=CARTESIAN_POINT('Ctrl Pts',(2.21892881679083,1.,3.31244421655662));
#42686=CARTESIAN_POINT('Ctrl Pts',(2.21703059947837,-1.,3.3050948781957));
#42687=CARTESIAN_POINT('Ctrl Pts',(2.21703059947837,1.,3.3050948781957));
#42688=CARTESIAN_POINT('Ctrl Pts',(2.21509406923369,-1.,3.29776825193162));
#42689=CARTESIAN_POINT('Ctrl Pts',(2.21509406923369,1.,3.29776825193162));
#42690=CARTESIAN_POINT('Ctrl Pts',(2.2131164882739,-1.,3.29046159238344));
#42691=CARTESIAN_POINT('Ctrl Pts',(2.2131164882739,1.,3.29046159238344));
#42692=CARTESIAN_POINT('Ctrl Pts',(2.21109449750638,-1.,3.28317133333127));
#42693=CARTESIAN_POINT('Ctrl Pts',(2.21109449750638,1.,3.28317133333127));
#42694=CARTESIAN_POINT('Ctrl Pts',(2.20902509417425,-1.,3.27589448005534));
#42695=CARTESIAN_POINT('Ctrl Pts',(2.20902509417425,1.,3.27589448005534));
#42696=CARTESIAN_POINT('Ctrl Pts',(2.20690665217741,-1.,3.2686300613678));
#42697=CARTESIAN_POINT('Ctrl Pts',(2.20690665217741,1.,3.2686300613678));
#42698=CARTESIAN_POINT('Ctrl Pts',(2.20473979048682,-1.,3.26138036637711));
#42699=CARTESIAN_POINT('Ctrl Pts',(2.20473979048682,1.,3.26138036637711));
#42700=CARTESIAN_POINT('Ctrl Pts',(2.20252866491554,-1.,3.25415277957789));
#42701=CARTESIAN_POINT('Ctrl Pts',(2.20252866491554,1.,3.25415277957789));
#42702=CARTESIAN_POINT('Ctrl Pts',(2.20027910880993,-1.,3.24695715874356));
#42703=CARTESIAN_POINT('Ctrl Pts',(2.20027910880993,1.,3.24695715874356));
#42704=CARTESIAN_POINT('Ctrl Pts',(2.19799623693263,-1.,3.23980245361323));
#42705=CARTESIAN_POINT('Ctrl Pts',(2.19799623693263,1.,3.23980245361323));
#42706=CARTESIAN_POINT('Ctrl Pts',(2.19568204933172,-1.,3.23269332296938));
#42707=CARTESIAN_POINT('Ctrl Pts',(2.19568204933172,1.,3.23269332296938));
#42708=CARTESIAN_POINT('Ctrl Pts',(2.19333345123531,-1.,3.22562734221636));
#42709=CARTESIAN_POINT('Ctrl Pts',(2.19333345123531,1.,3.22562734221636));
#42710=CARTESIAN_POINT('Ctrl Pts',(2.1909390194865,-1.,3.21859043114069));
#42711=CARTESIAN_POINT('Ctrl Pts',(2.1909390194865,1.,3.21859043114069));
#42712=CARTESIAN_POINT('Ctrl Pts',(2.18848253363878,-1.,3.21156188355736));
#42713=CARTESIAN_POINT('Ctrl Pts',(2.18848253363878,1.,3.21156188355736));
#42714=CARTESIAN_POINT('Ctrl Pts',(2.18594876115914,-1.,3.20452259717947));
#42715=CARTESIAN_POINT('Ctrl Pts',(2.18594876115914,1.,3.20452259717947));
#42716=CARTESIAN_POINT('Ctrl Pts',(2.18332898656595,-1.,3.197462937404));
#42717=CARTESIAN_POINT('Ctrl Pts',(2.18332898656595,1.,3.197462937404));
#42718=CARTESIAN_POINT('Ctrl Pts',(2.18062558031789,-1.,3.19038924261589));
#42719=CARTESIAN_POINT('Ctrl Pts',(2.18062558031789,1.,3.19038924261589));
#42720=CARTESIAN_POINT('Ctrl Pts',(2.17785968847172,-1.,3.18333474627851));
#42721=CARTESIAN_POINT('Ctrl Pts',(2.17785968847172,1.,3.18333474627851));
#42722=CARTESIAN_POINT('Ctrl Pts',(2.17506466903736,-1.,3.17635032802584));
#42723=CARTESIAN_POINT('Ctrl Pts',(2.17506466903736,1.,3.17635032802584));
#42724=CARTESIAN_POINT('Ctrl Pts',(2.17227212063857,-1.,3.16948480019555));
#42725=CARTESIAN_POINT('Ctrl Pts',(2.17227212063857,1.,3.16948480019555));
#42726=CARTESIAN_POINT('Ctrl Pts',(2.16949910801237,-1.,3.16276685102999));
#42727=CARTESIAN_POINT('Ctrl Pts',(2.16949910801237,1.,3.16276685102999));
#42728=CARTESIAN_POINT('Ctrl Pts',(2.1667372844767,-1.,3.15618975593627));
#42729=CARTESIAN_POINT('Ctrl Pts',(2.1667372844767,1.,3.15618975593627));
#42730=CARTESIAN_POINT('Ctrl Pts',(2.16393520288009,-1.,3.14968624388961));
#42731=CARTESIAN_POINT('Ctrl Pts',(2.16393520288009,1.,3.14968624388961));
#42732=CARTESIAN_POINT('Ctrl Pts',(2.16100905914341,-1.,3.14314440426882));
#42733=CARTESIAN_POINT('Ctrl Pts',(2.16100905914341,1.,3.14314440426882));
#42734=CARTESIAN_POINT('Ctrl Pts',(2.15787423530583,-1.,3.136453565629));
#42735=CARTESIAN_POINT('Ctrl Pts',(2.15787423530583,1.,3.136453565629));
#42736=CARTESIAN_POINT('Ctrl Pts',(2.15447241382872,-1.,3.12954386795575));
#42737=CARTESIAN_POINT('Ctrl Pts',(2.15447241382872,1.,3.12954386795575));
#42738=CARTESIAN_POINT('Ctrl Pts',(2.15079698090627,-1.,3.12242318152001));
#42739=CARTESIAN_POINT('Ctrl Pts',(2.15079698090627,1.,3.12242318152001));
#42740=CARTESIAN_POINT('Ctrl Pts',(2.1469279845768,-1.,3.11522827017075));
#42741=CARTESIAN_POINT('Ctrl Pts',(2.1469279845768,1.,3.11522827017075));
#42742=CARTESIAN_POINT('Ctrl Pts',(2.14302815602195,-1.,3.10821808669189));
#42743=CARTESIAN_POINT('Ctrl Pts',(2.14302815602195,1.,3.10821808669189));
#42744=CARTESIAN_POINT('Ctrl Pts',(2.13930228863968,-1.,3.1017126739137));
#42745=CARTESIAN_POINT('Ctrl Pts',(2.13930228863968,1.,3.1017126739137));
#42746=CARTESIAN_POINT('Ctrl Pts',(2.13596538661154,-1.,3.09604502421197));
#42747=CARTESIAN_POINT('Ctrl Pts',(2.13596538661154,1.,3.09604502421197));
#42748=CARTESIAN_POINT('Ctrl Pts',(2.13321032560805,-1.,3.09151235281832));
#42749=CARTESIAN_POINT('Ctrl Pts',(2.13321032560805,1.,3.09151235281832));
#42750=CARTESIAN_POINT('Ctrl Pts',(2.13116819908263,-1.,3.08831615619661));
#42751=CARTESIAN_POINT('Ctrl Pts',(2.13116819908263,1.,3.08831615619661));
#42752=CARTESIAN_POINT('Ctrl Pts',(2.1301541297915,-1.,3.08690399991003));
#42753=CARTESIAN_POINT('Ctrl Pts',(2.1301541297915,1.,3.08690399991003));
#42754=CARTESIAN_POINT('Ctrl Pts',(2.12975158752197,-1.,3.08650326866821));
#42755=CARTESIAN_POINT('Ctrl Pts',(2.12975158752197,1.,3.08650326866821));
#42756=CARTESIAN_POINT('Ctrl Pts',(2.12964222015945,-1.,3.08652852644876));
#42757=CARTESIAN_POINT('Ctrl Pts',(2.12964222015945,1.,3.08652852644876));
#42758=CARTESIAN_POINT('Ctrl Pts',(2.12962728847314,-1.,3.08661426358891));
#42759=CARTESIAN_POINT('Ctrl Pts',(2.12962728847314,1.,3.08661426358891));
#42760=CARTESIAN_POINT('',(2.25898783642071,1.,3.54075895182139));
#42761=CARTESIAN_POINT('Ctrl Pts',(2.25898783642071,1.,3.54075895182139));
#42762=CARTESIAN_POINT('Ctrl Pts',(2.25882251694918,1.,3.5391950664771));
#42763=CARTESIAN_POINT('Ctrl Pts',(2.25848864344599,1.,3.53606853163247));
#42764=CARTESIAN_POINT('Ctrl Pts',(2.25797812951166,1.,3.53138243689932));
#42765=CARTESIAN_POINT('Ctrl Pts',(2.25727802942141,1.,3.52514172849666));
#42766=CARTESIAN_POINT('Ctrl Pts',(2.25637049456061,1.,3.51735323669213));
#42767=CARTESIAN_POINT('Ctrl Pts',(2.25543046980351,1.,3.50957720118209));
#42768=CARTESIAN_POINT('Ctrl Pts',(2.25445785151923,1.,3.50181372618058));
#42769=CARTESIAN_POINT('Ctrl Pts',(2.25345251709453,1.,3.49406296494309));
#42770=CARTESIAN_POINT('Ctrl Pts',(2.25241433138231,1.,3.48632513240231));
#42771=CARTESIAN_POINT('Ctrl Pts',(2.25134314238258,1.,3.47860048448015));
#42772=CARTESIAN_POINT('Ctrl Pts',(2.25023877475674,1.,3.47088928979467));
#42773=CARTESIAN_POINT('Ctrl Pts',(2.24910102345977,1.,3.46319180177474));
#42774=CARTESIAN_POINT('Ctrl Pts',(2.24792964960874,1.,3.45550823512213));
#42775=CARTESIAN_POINT('Ctrl Pts',(2.24672437070139,1.,3.44783872863448));
#42776=CARTESIAN_POINT('Ctrl Pts',(2.24548487526212,1.,3.44018336460619));
#42777=CARTESIAN_POINT('Ctrl Pts',(2.24421085338856,1.,3.43254222615007));
#42778=CARTESIAN_POINT('Ctrl Pts',(2.24290202531144,1.,3.42491544683075));
#42779=CARTESIAN_POINT('Ctrl Pts',(2.24155816587811,1.,3.41730325539119));
#42780=CARTESIAN_POINT('Ctrl Pts',(2.24017914395211,1.,3.40970604190205));
#42781=CARTESIAN_POINT('Ctrl Pts',(2.23876491124064,1.,3.40212434705511));
#42782=CARTESIAN_POINT('Ctrl Pts',(2.23731541452726,1.,3.39455873448088));
#42783=CARTESIAN_POINT('Ctrl Pts',(2.23583052276281,1.,3.38700968549522));
#42784=CARTESIAN_POINT('Ctrl Pts',(2.23430995599572,1.,3.37947749555649));
#42785=CARTESIAN_POINT('Ctrl Pts',(2.23275319569253,1.,3.37196214349356));
#42786=CARTESIAN_POINT('Ctrl Pts',(2.23115945849777,1.,3.36446325227908));
#42787=CARTESIAN_POINT('Ctrl Pts',(2.22952789881011,1.,3.35698038165529));
#42788=CARTESIAN_POINT('Ctrl Pts',(2.22785777756588,1.,3.34951327111117));
#42789=CARTESIAN_POINT('Ctrl Pts',(2.22614863918044,1.,3.34206209449371));
#42790=CARTESIAN_POINT('Ctrl Pts',(2.224400498785,1.,3.3346277284958));
#42791=CARTESIAN_POINT('Ctrl Pts',(2.22261398879623,1.,3.32721196326019));
#42792=CARTESIAN_POINT('Ctrl Pts',(2.22078990842768,1.,3.31981686778008));
#42793=CARTESIAN_POINT('Ctrl Pts',(2.21892881679083,1.,3.31244421655662));
#42794=CARTESIAN_POINT('Ctrl Pts',(2.21703059947837,1.,3.3050948781957));
#42795=CARTESIAN_POINT('Ctrl Pts',(2.21509406923369,1.,3.29776825193162));
#42796=CARTESIAN_POINT('Ctrl Pts',(2.2131164882739,1.,3.29046159238344));
#42797=CARTESIAN_POINT('Ctrl Pts',(2.21109449750638,1.,3.28317133333127));
#42798=CARTESIAN_POINT('Ctrl Pts',(2.20902509417425,1.,3.27589448005534));
#42799=CARTESIAN_POINT('Ctrl Pts',(2.20690665217741,1.,3.2686300613678));
#42800=CARTESIAN_POINT('Ctrl Pts',(2.20473979048682,1.,3.26138036637711));
#42801=CARTESIAN_POINT('Ctrl Pts',(2.20252866491554,1.,3.25415277957789));
#42802=CARTESIAN_POINT('Ctrl Pts',(2.20027910880993,1.,3.24695715874356));
#42803=CARTESIAN_POINT('Ctrl Pts',(2.19799623693263,1.,3.23980245361323));
#42804=CARTESIAN_POINT('Ctrl Pts',(2.19568204933172,1.,3.23269332296938));
#42805=CARTESIAN_POINT('Ctrl Pts',(2.19333345123531,1.,3.22562734221636));
#42806=CARTESIAN_POINT('Ctrl Pts',(2.1909390194865,1.,3.21859043114069));
#42807=CARTESIAN_POINT('Ctrl Pts',(2.18848253363878,1.,3.21156188355736));
#42808=CARTESIAN_POINT('Ctrl Pts',(2.18594876115914,1.,3.20452259717947));
#42809=CARTESIAN_POINT('Ctrl Pts',(2.18332898656595,1.,3.197462937404));
#42810=CARTESIAN_POINT('Ctrl Pts',(2.18062558031789,1.,3.19038924261589));
#42811=CARTESIAN_POINT('Ctrl Pts',(2.17785968847172,1.,3.18333474627851));
#42812=CARTESIAN_POINT('Ctrl Pts',(2.17506466903736,1.,3.17635032802584));
#42813=CARTESIAN_POINT('Ctrl Pts',(2.17227212063857,1.,3.16948480019555));
#42814=CARTESIAN_POINT('Ctrl Pts',(2.16949910801237,1.,3.16276685102999));
#42815=CARTESIAN_POINT('Ctrl Pts',(2.1667372844767,1.,3.15618975593627));
#42816=CARTESIAN_POINT('Ctrl Pts',(2.16393520288009,1.,3.14968624388961));
#42817=CARTESIAN_POINT('Ctrl Pts',(2.16100905914341,1.,3.14314440426882));
#42818=CARTESIAN_POINT('Ctrl Pts',(2.15787423530583,1.,3.136453565629));
#42819=CARTESIAN_POINT('Ctrl Pts',(2.15447241382872,1.,3.12954386795575));
#42820=CARTESIAN_POINT('Ctrl Pts',(2.15079698090627,1.,3.12242318152001));
#42821=CARTESIAN_POINT('Ctrl Pts',(2.1469279845768,1.,3.11522827017075));
#42822=CARTESIAN_POINT('Ctrl Pts',(2.14302815602195,1.,3.10821808669189));
#42823=CARTESIAN_POINT('Ctrl Pts',(2.13930228863968,1.,3.1017126739137));
#42824=CARTESIAN_POINT('Ctrl Pts',(2.13596538661154,1.,3.09604502421197));
#42825=CARTESIAN_POINT('Ctrl Pts',(2.13321032560805,1.,3.09151235281832));
#42826=CARTESIAN_POINT('Ctrl Pts',(2.13132142793056,1.,3.08855597949844));
#42827=CARTESIAN_POINT('Ctrl Pts',(2.13034980480519,1.,3.08717896996213));
#42828=CARTESIAN_POINT('Ctrl Pts',(2.12991938762497,1.,3.08668447250383));
#42829=CARTESIAN_POINT('Ctrl Pts',(2.1297578506162,1.,3.0865713108946));
#42830=CARTESIAN_POINT('Ctrl Pts',(2.12971124846838,1.,3.0865563332211));
#42831=CARTESIAN_POINT('',(2.25898783642071,0.,3.54075895182139));
#42832=CARTESIAN_POINT('Ctrl Pts',(1.7833628895577,-1.,3.2988053601491));
#42833=CARTESIAN_POINT('Ctrl Pts',(1.7833628895577,1.,3.2988053601491));
#42834=CARTESIAN_POINT('Ctrl Pts',(1.78327971836342,-1.,3.29877974053316));
#42835=CARTESIAN_POINT('Ctrl Pts',(1.78327971836342,1.,3.29877974053316));
#42836=CARTESIAN_POINT('Ctrl Pts',(1.78320756177373,-1.,3.29886572077632));
#42837=CARTESIAN_POINT('Ctrl Pts',(1.78320756177373,1.,3.29886572077632));
#42838=CARTESIAN_POINT('Ctrl Pts',(1.7833818655594,-1.,3.29940631674303));
#42839=CARTESIAN_POINT('Ctrl Pts',(1.7833818655594,1.,3.29940631674303));
#42840=CARTESIAN_POINT('Ctrl Pts',(1.78417972819938,-1.,3.30095096463517));
#42841=CARTESIAN_POINT('Ctrl Pts',(1.78417972819938,1.,3.30095096463517));
#42842=CARTESIAN_POINT('Ctrl Pts',(1.78610045419846,-1.,3.30422155559112));
#42843=CARTESIAN_POINT('Ctrl Pts',(1.78610045419846,1.,3.30422155559112));
#42844=CARTESIAN_POINT('Ctrl Pts',(1.78888832245873,-1.,3.30873412266788));
#42845=CARTESIAN_POINT('Ctrl Pts',(1.78888832245873,1.,3.30873412266788));
#42846=CARTESIAN_POINT('Ctrl Pts',(1.79242331349949,-1.,3.31428038326424));
#42847=CARTESIAN_POINT('Ctrl Pts',(1.79242331349949,1.,3.31428038326424));
#42848=CARTESIAN_POINT('Ctrl Pts',(1.79652817033251,-1.,3.3205535510082));
#42849=CARTESIAN_POINT('Ctrl Pts',(1.79652817033251,1.,3.3205535510082));
#42850=CARTESIAN_POINT('Ctrl Pts',(1.80100380443406,-1.,3.32721088039578));
#42851=CARTESIAN_POINT('Ctrl Pts',(1.80100380443406,1.,3.32721088039578));
#42852=CARTESIAN_POINT('Ctrl Pts',(1.80565802981102,-1.,3.33392460276808));
#42853=CARTESIAN_POINT('Ctrl Pts',(1.80565802981102,1.,3.33392460276808));
#42854=CARTESIAN_POINT('Ctrl Pts',(1.81033399625352,-1.,3.34043216147606));
#42855=CARTESIAN_POINT('Ctrl Pts',(1.81033399625352,1.,3.34043216147606));
#42856=CARTESIAN_POINT('Ctrl Pts',(1.81494618732853,-1.,3.34660014370673));
#42857=CARTESIAN_POINT('Ctrl Pts',(1.81494618732853,1.,3.34660014370673));
#42858=CARTESIAN_POINT('Ctrl Pts',(1.81948458796829,-1.,3.35243086937598));
#42859=CARTESIAN_POINT('Ctrl Pts',(1.81948458796829,1.,3.35243086937598));
#42860=CARTESIAN_POINT('Ctrl Pts',(1.82398496829301,-1.,3.35800801557424));
#42861=CARTESIAN_POINT('Ctrl Pts',(1.82398496829301,1.,3.35800801557424));
#42862=CARTESIAN_POINT('Ctrl Pts',(1.82850752153199,-1.,3.36345722124158));
#42863=CARTESIAN_POINT('Ctrl Pts',(1.82850752153199,1.,3.36345722124158));
#42864=CARTESIAN_POINT('Ctrl Pts',(1.83311391452322,-1.,3.36890396271836));
#42865=CARTESIAN_POINT('Ctrl Pts',(1.83311391452322,1.,3.36890396271836));
#42866=CARTESIAN_POINT('Ctrl Pts',(1.83784072967077,-1.,3.37442462015853));
#42867=CARTESIAN_POINT('Ctrl Pts',(1.83784072967077,1.,3.37442462015853));
#42868=CARTESIAN_POINT('Ctrl Pts',(1.84269016931643,-1.,3.38002968341157));
#42869=CARTESIAN_POINT('Ctrl Pts',(1.84269016931643,1.,3.38002968341157));
#42870=CARTESIAN_POINT('Ctrl Pts',(1.84764441927753,-1.,3.38569092349592));
#42871=CARTESIAN_POINT('Ctrl Pts',(1.84764441927753,1.,3.38569092349592));
#42872=CARTESIAN_POINT('Ctrl Pts',(1.85267433291769,-1.,3.39135802549398));
#42873=CARTESIAN_POINT('Ctrl Pts',(1.85267433291769,1.,3.39135802549398));
#42874=CARTESIAN_POINT('Ctrl Pts',(1.85774972037062,-1.,3.39697816833067));
#42875=CARTESIAN_POINT('Ctrl Pts',(1.85774972037062,1.,3.39697816833067));
#42876=CARTESIAN_POINT('Ctrl Pts',(1.86285057051245,-1.,3.40251742305476));
#42877=CARTESIAN_POINT('Ctrl Pts',(1.86285057051245,1.,3.40251742305476));
#42878=CARTESIAN_POINT('Ctrl Pts',(1.86797231196654,-1.,3.40797080000549));
#42879=CARTESIAN_POINT('Ctrl Pts',(1.86797231196654,1.,3.40797080000549));
#42880=CARTESIAN_POINT('Ctrl Pts',(1.87311957248121,-1.,3.41335043875209));
#42881=CARTESIAN_POINT('Ctrl Pts',(1.87311957248121,1.,3.41335043875209));
#42882=CARTESIAN_POINT('Ctrl Pts',(1.87830245689344,-1.,3.41867858383771));
#42883=CARTESIAN_POINT('Ctrl Pts',(1.87830245689344,1.,3.41867858383771));
#42884=CARTESIAN_POINT('Ctrl Pts',(1.8835320506206,-1.,3.42397908819736));
#42885=CARTESIAN_POINT('Ctrl Pts',(1.8835320506206,1.,3.42397908819736));
#42886=CARTESIAN_POINT('Ctrl Pts',(1.88881571322009,-1.,3.42926852222158));
#42887=CARTESIAN_POINT('Ctrl Pts',(1.88881571322009,1.,3.42926852222158));
#42888=CARTESIAN_POINT('Ctrl Pts',(1.89415420002542,-1.,3.43455074411571));
#42889=CARTESIAN_POINT('Ctrl Pts',(1.89415420002542,1.,3.43455074411571));
#42890=CARTESIAN_POINT('Ctrl Pts',(1.89954426803384,-1.,3.4398218567809));
#42891=CARTESIAN_POINT('Ctrl Pts',(1.89954426803384,1.,3.4398218567809));
#42892=CARTESIAN_POINT('Ctrl Pts',(1.90498026502304,-1.,3.44507323983368));
#42893=CARTESIAN_POINT('Ctrl Pts',(1.90498026502304,1.,3.44507323983368));
#42894=CARTESIAN_POINT('Ctrl Pts',(1.91045605593639,-1.,3.45029522038888));
#42895=CARTESIAN_POINT('Ctrl Pts',(1.91045605593639,1.,3.45029522038888));
#42896=CARTESIAN_POINT('Ctrl Pts',(1.91596694784063,-1.,3.4554807430995));
#42897=CARTESIAN_POINT('Ctrl Pts',(1.91596694784063,1.,3.4554807430995));
#42898=CARTESIAN_POINT('Ctrl Pts',(1.92151118213212,-1.,3.46062821722485));
#42899=CARTESIAN_POINT('Ctrl Pts',(1.92151118213212,1.,3.46062821722485));
#42900=CARTESIAN_POINT('Ctrl Pts',(1.92708888591158,-1.,3.46573953254084));
#42901=CARTESIAN_POINT('Ctrl Pts',(1.92708888591158,1.,3.46573953254084));
#42902=CARTESIAN_POINT('Ctrl Pts',(1.93270136427081,-1.,3.47081872409781));
#42903=CARTESIAN_POINT('Ctrl Pts',(1.93270136427081,1.,3.47081872409781));
#42904=CARTESIAN_POINT('Ctrl Pts',(1.93835026973887,-1.,3.47587040389915));
#42905=CARTESIAN_POINT('Ctrl Pts',(1.93835026973887,1.,3.47587040389915));
#42906=CARTESIAN_POINT('Ctrl Pts',(1.94403680554065,-1.,3.48089825770416));
#42907=CARTESIAN_POINT('Ctrl Pts',(1.94403680554065,1.,3.48089825770416));
#42908=CARTESIAN_POINT('Ctrl Pts',(1.94976096795911,-1.,3.48590361610814));
#42909=CARTESIAN_POINT('Ctrl Pts',(1.94976096795911,1.,3.48590361610814));
#42910=CARTESIAN_POINT('Ctrl Pts',(1.95552193112084,-1.,3.49088618670987));
#42911=CARTESIAN_POINT('Ctrl Pts',(1.95552193112084,1.,3.49088618670987));
#42912=CARTESIAN_POINT('Ctrl Pts',(1.961318367765,-1.,3.49584466573064));
#42913=CARTESIAN_POINT('Ctrl Pts',(1.961318367765,1.,3.49584466573064));
#42914=CARTESIAN_POINT('Ctrl Pts',(1.96714879724052,-1.,3.50077740176267));
#42915=CARTESIAN_POINT('Ctrl Pts',(1.96714879724052,1.,3.50077740176267));
#42916=CARTESIAN_POINT('Ctrl Pts',(1.97301191162968,-1.,3.5056830186108));
#42917=CARTESIAN_POINT('Ctrl Pts',(1.97301191162968,1.,3.5056830186108));
#42918=CARTESIAN_POINT('Ctrl Pts',(1.97890693666288,-1.,3.51056110478287));
#42919=CARTESIAN_POINT('Ctrl Pts',(1.97890693666288,1.,3.51056110478287));
#42920=CARTESIAN_POINT('Ctrl Pts',(1.9848335106103,-1.,3.51541198728301));
#42921=CARTESIAN_POINT('Ctrl Pts',(1.9848335106103,1.,3.51541198728301));
#42922=CARTESIAN_POINT('Ctrl Pts',(1.99079153006112,-1.,3.52023644289142));
#42923=CARTESIAN_POINT('Ctrl Pts',(1.99079153006112,1.,3.52023644289142));
#42924=CARTESIAN_POINT('Ctrl Pts',(1.99678100339295,-1.,3.52503542491728));
#42925=CARTESIAN_POINT('Ctrl Pts',(1.99678100339295,1.,3.52503542491728));
#42926=CARTESIAN_POINT('Ctrl Pts',(2.00280191090366,-1.,3.52980980250224));
#42927=CARTESIAN_POINT('Ctrl Pts',(2.00280191090366,1.,3.52980980250224));
#42928=CARTESIAN_POINT('Ctrl Pts',(2.00885403604746,-1.,3.53456004727424));
#42929=CARTESIAN_POINT('Ctrl Pts',(2.00885403604746,1.,3.53456004727424));
#42930=CARTESIAN_POINT('Ctrl Pts',(2.01493698847351,-1.,3.53928627453642));
#42931=CARTESIAN_POINT('Ctrl Pts',(2.01493698847351,1.,3.53928627453642));
#42932=CARTESIAN_POINT('Ctrl Pts',(2.02105027983104,-1.,3.54398838254136));
#42933=CARTESIAN_POINT('Ctrl Pts',(2.02105027983104,1.,3.54398838254136));
#42934=CARTESIAN_POINT('Ctrl Pts',(2.02719338376175,-1.,3.54866616282227));
#42935=CARTESIAN_POINT('Ctrl Pts',(2.02719338376175,1.,3.54866616282227));
#42936=CARTESIAN_POINT('Ctrl Pts',(2.03336579658133,-1.,3.55331941293949));
#42937=CARTESIAN_POINT('Ctrl Pts',(2.03336579658133,1.,3.55331941293949));
#42938=CARTESIAN_POINT('Ctrl Pts',(2.03956711119976,-1.,3.55794807264844));
#42939=CARTESIAN_POINT('Ctrl Pts',(2.03956711119976,1.,3.55794807264844));
#42940=CARTESIAN_POINT('Ctrl Pts',(2.04579702158876,-1.,3.56255223871505));
#42941=CARTESIAN_POINT('Ctrl Pts',(2.04579702158876,1.,3.56255223871505));
#42942=CARTESIAN_POINT('Ctrl Pts',(2.05205528172911,-1.,3.56713209977904));
#42943=CARTESIAN_POINT('Ctrl Pts',(2.05205528172911,1.,3.56713209977904));
#42944=CARTESIAN_POINT('Ctrl Pts',(2.05834167687425,-1.,3.5716878942334));
#42945=CARTESIAN_POINT('Ctrl Pts',(2.05834167687425,1.,3.5716878942334));
#42946=CARTESIAN_POINT('Ctrl Pts',(2.06465599229234,-1.,3.57621986224402));
#42947=CARTESIAN_POINT('Ctrl Pts',(2.06465599229234,1.,3.57621986224402));
#42948=CARTESIAN_POINT('Ctrl Pts',(2.07099797606,-1.,3.58072819250872));
#42949=CARTESIAN_POINT('Ctrl Pts',(2.07099797606,1.,3.58072819250872));
#42950=CARTESIAN_POINT('Ctrl Pts',(2.07736732842524,-1.,3.58521300039988));
#42951=CARTESIAN_POINT('Ctrl Pts',(2.07736732842524,1.,3.58521300039988));
#42952=CARTESIAN_POINT('Ctrl Pts',(2.08376373049196,-1.,3.58967435355834));
#42953=CARTESIAN_POINT('Ctrl Pts',(2.08376373049196,1.,3.58967435355834));
#42954=CARTESIAN_POINT('Ctrl Pts',(2.09018686331706,-1.,3.5941122862608));
#42955=CARTESIAN_POINT('Ctrl Pts',(2.09018686331706,1.,3.5941122862608));
#42956=CARTESIAN_POINT('Ctrl Pts',(2.09663642986579,-1.,3.59852681775396));
#42957=CARTESIAN_POINT('Ctrl Pts',(2.09663642986579,1.,3.59852681775396));
#42958=CARTESIAN_POINT('Ctrl Pts',(2.10311217727687,-1.,3.60291797087849));
#42959=CARTESIAN_POINT('Ctrl Pts',(2.10311217727687,1.,3.60291797087849));
#42960=CARTESIAN_POINT('Ctrl Pts',(2.10961391333497,-1.,3.60728578530968));
#42961=CARTESIAN_POINT('Ctrl Pts',(2.10961391333497,1.,3.60728578530968));
#42962=CARTESIAN_POINT('Ctrl Pts',(2.11614149813928,-1.,3.61163030607452));
#42963=CARTESIAN_POINT('Ctrl Pts',(2.11614149813928,1.,3.61163030607452));
#42964=CARTESIAN_POINT('Ctrl Pts',(2.12138417125349,-1.,3.61508732215187));
#42965=CARTESIAN_POINT('Ctrl Pts',(2.12138417125349,1.,3.61508732215187));
#42966=CARTESIAN_POINT('Ctrl Pts',(2.12532774376144,-1.,3.61766963589442));
#42967=CARTESIAN_POINT('Ctrl Pts',(2.12532774376144,1.,3.61766963589442));
#42968=CARTESIAN_POINT('Ctrl Pts',(2.12796193131142,-1.,3.61938653648716));
#42969=CARTESIAN_POINT('Ctrl Pts',(2.12796193131142,1.,3.61938653648716));
#42970=CARTESIAN_POINT('Ctrl Pts',(2.12928030988903,-1.,3.62024382630768));
#42971=CARTESIAN_POINT('Ctrl Pts',(2.12928030988903,1.,3.62024382630768));
#42972=CARTESIAN_POINT('',(1.78327315618341,1.,3.29885386921513));
#42973=CARTESIAN_POINT('Ctrl Pts',(1.78327315618341,-1.,3.29885386921514));
#42974=CARTESIAN_POINT('Ctrl Pts',(1.78327315618341,-0.666666666666667,
3.29885386921514));
#42975=CARTESIAN_POINT('Ctrl Pts',(1.78327315618341,-0.333333333333333,
3.29885386921514));
#42976=CARTESIAN_POINT('Ctrl Pts',(1.78327315618341,0.333333333333333,3.29885386921514));
#42977=CARTESIAN_POINT('Ctrl Pts',(1.78327315618341,0.666666666666667,3.29885386921513));
#42978=CARTESIAN_POINT('Ctrl Pts',(1.78327315618341,1.,3.29885386921513));
#42979=CARTESIAN_POINT('',(2.12928030988903,1.,3.62024382630768));
#42980=CARTESIAN_POINT('',(2.12928030988903,0.,3.62024382630768));
#42981=CARTESIAN_POINT('Ctrl Pts',(1.78327315618341,1.,3.29885386921513));
#42982=CARTESIAN_POINT('Ctrl Pts',(1.78326534445518,1.,3.29890219175423));
#42983=CARTESIAN_POINT('Ctrl Pts',(1.78329283591905,1.,3.29909749657808));
#42984=CARTESIAN_POINT('Ctrl Pts',(1.78353803106924,1.,3.299705498242));
#42985=CARTESIAN_POINT('Ctrl Pts',(1.78432384788174,1.,3.30119637003393));
#42986=CARTESIAN_POINT('Ctrl Pts',(1.78610045419846,1.,3.30422155559112));
#42987=CARTESIAN_POINT('Ctrl Pts',(1.78888832245873,1.,3.30873412266788));
#42988=CARTESIAN_POINT('Ctrl Pts',(1.79242331349949,1.,3.31428038326424));
#42989=CARTESIAN_POINT('Ctrl Pts',(1.79652817033251,1.,3.3205535510082));
#42990=CARTESIAN_POINT('Ctrl Pts',(1.80100380443406,1.,3.32721088039578));
#42991=CARTESIAN_POINT('Ctrl Pts',(1.80565802981102,1.,3.33392460276808));
#42992=CARTESIAN_POINT('Ctrl Pts',(1.81033399625352,1.,3.34043216147606));
#42993=CARTESIAN_POINT('Ctrl Pts',(1.81494618732853,1.,3.34660014370673));
#42994=CARTESIAN_POINT('Ctrl Pts',(1.81948458796829,1.,3.35243086937598));
#42995=CARTESIAN_POINT('Ctrl Pts',(1.82398496829301,1.,3.35800801557424));
#42996=CARTESIAN_POINT('Ctrl Pts',(1.82850752153199,1.,3.36345722124158));
#42997=CARTESIAN_POINT('Ctrl Pts',(1.83311391452322,1.,3.36890396271836));
#42998=CARTESIAN_POINT('Ctrl Pts',(1.83784072967077,1.,3.37442462015853));
#42999=CARTESIAN_POINT('Ctrl Pts',(1.84269016931643,1.,3.38002968341157));
#43000=CARTESIAN_POINT('Ctrl Pts',(1.84764441927753,1.,3.38569092349592));
#43001=CARTESIAN_POINT('Ctrl Pts',(1.85267433291769,1.,3.39135802549398));
#43002=CARTESIAN_POINT('Ctrl Pts',(1.85774972037062,1.,3.39697816833067));
#43003=CARTESIAN_POINT('Ctrl Pts',(1.86285057051245,1.,3.40251742305476));
#43004=CARTESIAN_POINT('Ctrl Pts',(1.86797231196654,1.,3.40797080000549));
#43005=CARTESIAN_POINT('Ctrl Pts',(1.87311957248121,1.,3.41335043875209));
#43006=CARTESIAN_POINT('Ctrl Pts',(1.87830245689344,1.,3.41867858383771));
#43007=CARTESIAN_POINT('Ctrl Pts',(1.8835320506206,1.,3.42397908819736));
#43008=CARTESIAN_POINT('Ctrl Pts',(1.88881571322009,1.,3.42926852222158));
#43009=CARTESIAN_POINT('Ctrl Pts',(1.89415420002542,1.,3.43455074411571));
#43010=CARTESIAN_POINT('Ctrl Pts',(1.89954426803384,1.,3.4398218567809));
#43011=CARTESIAN_POINT('Ctrl Pts',(1.90498026502304,1.,3.44507323983368));
#43012=CARTESIAN_POINT('Ctrl Pts',(1.91045605593639,1.,3.45029522038888));
#43013=CARTESIAN_POINT('Ctrl Pts',(1.91596694784063,1.,3.4554807430995));
#43014=CARTESIAN_POINT('Ctrl Pts',(1.92151118213212,1.,3.46062821722485));
#43015=CARTESIAN_POINT('Ctrl Pts',(1.92708888591158,1.,3.46573953254084));
#43016=CARTESIAN_POINT('Ctrl Pts',(1.93270136427081,1.,3.47081872409781));
#43017=CARTESIAN_POINT('Ctrl Pts',(1.93835026973887,1.,3.47587040389915));
#43018=CARTESIAN_POINT('Ctrl Pts',(1.94403680554065,1.,3.48089825770416));
#43019=CARTESIAN_POINT('Ctrl Pts',(1.94976096795911,1.,3.48590361610814));
#43020=CARTESIAN_POINT('Ctrl Pts',(1.95552193112084,1.,3.49088618670987));
#43021=CARTESIAN_POINT('Ctrl Pts',(1.961318367765,1.,3.49584466573064));
#43022=CARTESIAN_POINT('Ctrl Pts',(1.96714879724052,1.,3.50077740176267));
#43023=CARTESIAN_POINT('Ctrl Pts',(1.97301191162968,1.,3.5056830186108));
#43024=CARTESIAN_POINT('Ctrl Pts',(1.97890693666288,1.,3.51056110478287));
#43025=CARTESIAN_POINT('Ctrl Pts',(1.9848335106103,1.,3.51541198728301));
#43026=CARTESIAN_POINT('Ctrl Pts',(1.99079153006112,1.,3.52023644289142));
#43027=CARTESIAN_POINT('Ctrl Pts',(1.99678100339295,1.,3.52503542491728));
#43028=CARTESIAN_POINT('Ctrl Pts',(2.00280191090366,1.,3.52980980250224));
#43029=CARTESIAN_POINT('Ctrl Pts',(2.00885403604746,1.,3.53456004727424));
#43030=CARTESIAN_POINT('Ctrl Pts',(2.01493698847351,1.,3.53928627453642));
#43031=CARTESIAN_POINT('Ctrl Pts',(2.02105027983104,1.,3.54398838254136));
#43032=CARTESIAN_POINT('Ctrl Pts',(2.02719338376175,1.,3.54866616282227));
#43033=CARTESIAN_POINT('Ctrl Pts',(2.03336579658133,1.,3.55331941293949));
#43034=CARTESIAN_POINT('Ctrl Pts',(2.03956711119976,1.,3.55794807264844));
#43035=CARTESIAN_POINT('Ctrl Pts',(2.04579702158876,1.,3.56255223871505));
#43036=CARTESIAN_POINT('Ctrl Pts',(2.05205528172911,1.,3.56713209977904));
#43037=CARTESIAN_POINT('Ctrl Pts',(2.05834167687425,1.,3.5716878942334));
#43038=CARTESIAN_POINT('Ctrl Pts',(2.06465599229234,1.,3.57621986224402));
#43039=CARTESIAN_POINT('Ctrl Pts',(2.07099797606,1.,3.58072819250872));
#43040=CARTESIAN_POINT('Ctrl Pts',(2.07736732842524,1.,3.58521300039988));
#43041=CARTESIAN_POINT('Ctrl Pts',(2.08376373049196,1.,3.58967435355834));
#43042=CARTESIAN_POINT('Ctrl Pts',(2.09018686331706,1.,3.5941122862608));
#43043=CARTESIAN_POINT('Ctrl Pts',(2.09663642986579,1.,3.59852681775396));
#43044=CARTESIAN_POINT('Ctrl Pts',(2.10311217727687,1.,3.60291797087849));
#43045=CARTESIAN_POINT('Ctrl Pts',(2.10961391333497,1.,3.60728578530968));
#43046=CARTESIAN_POINT('Ctrl Pts',(2.11614149813928,1.,3.61163030607452));
#43047=CARTESIAN_POINT('Ctrl Pts',(2.12138417125349,1.,3.61508732215187));
#43048=CARTESIAN_POINT('Ctrl Pts',(2.12532774376144,1.,3.61766963589442));
#43049=CARTESIAN_POINT('Ctrl Pts',(2.12796193131142,1.,3.61938653648716));
#43050=CARTESIAN_POINT('Ctrl Pts',(2.12928030988903,1.,3.62024382630768));
#43051=CARTESIAN_POINT('Origin',(2.12928030988903,0.,3.62024382630768));
#43052=CARTESIAN_POINT('',(2.25898783642071,1.,3.54075895182139));
#43053=CARTESIAN_POINT('Origin',(0.,0.,0.));
#43054=CARTESIAN_POINT('',(1.62064718014256,1.,3.38171594275687));
#43055=CARTESIAN_POINT('Origin',(0.,1.,0.));
#43056=CARTESIAN_POINT('Ctrl Pts',(1.62064718014256,1.,3.38171594275687));
#43057=CARTESIAN_POINT('Ctrl Pts',(1.62064718014256,0.666666666666667,3.38171594275687));
#43058=CARTESIAN_POINT('Ctrl Pts',(1.62064718014256,0.333333333333333,3.38171594275687));
#43059=CARTESIAN_POINT('Ctrl Pts',(1.62064718014256,-0.333333333333333,
3.38171594275687));
#43060=CARTESIAN_POINT('Ctrl Pts',(1.62064718014256,-0.666666666666667,
3.38171594275687));
#43061=CARTESIAN_POINT('Ctrl Pts',(1.62064718014256,-1.,3.38171594275687));
#43062=CARTESIAN_POINT('Ctrl Pts',(1.67727921511438,-1.,3.85054988729471));
#43063=CARTESIAN_POINT('Ctrl Pts',(1.67727921511438,1.,3.85054988729471));
#43064=CARTESIAN_POINT('Ctrl Pts',(1.6773605765671,-1.,3.84897939431104));
#43065=CARTESIAN_POINT('Ctrl Pts',(1.6773605765671,1.,3.84897939431104));
#43066=CARTESIAN_POINT('Ctrl Pts',(1.67751991140661,-1.,3.84583912297567));
#43067=CARTESIAN_POINT('Ctrl Pts',(1.67751991140661,1.,3.84583912297567));
#43068=CARTESIAN_POINT('Ctrl Pts',(1.67774874946867,-1.,3.8411308598706));
#43069=CARTESIAN_POINT('Ctrl Pts',(1.67774874946867,1.,3.8411308598706));
#43070=CARTESIAN_POINT('Ctrl Pts',(1.67803353065273,-1.,3.83485746516115));
#43071=CARTESIAN_POINT('Ctrl Pts',(1.67803353065273,1.,3.83485746516115));
#43072=CARTESIAN_POINT('Ctrl Pts',(1.67835555760094,-1.,3.82702289288453));
#43073=CARTESIAN_POINT('Ctrl Pts',(1.67835555760094,1.,3.82702289288453));
#43074=CARTESIAN_POINT('Ctrl Pts',(1.67864354606363,-1.,3.81919554100522));
#43075=CARTESIAN_POINT('Ctrl Pts',(1.67864354606363,1.,3.81919554100522));
#43076=CARTESIAN_POINT('Ctrl Pts',(1.67889737738311,-1.,3.81137549624273));
#43077=CARTESIAN_POINT('Ctrl Pts',(1.67889737738311,1.,3.81137549624273));
#43078=CARTESIAN_POINT('Ctrl Pts',(1.67911690648128,-1.,3.80356289078481));
#43079=CARTESIAN_POINT('Ctrl Pts',(1.67911690648128,1.,3.80356289078481));
#43080=CARTESIAN_POINT('Ctrl Pts',(1.67930196625203,-1.,3.7957579157763));
#43081=CARTESIAN_POINT('Ctrl Pts',(1.67930196625203,1.,3.7957579157763));
#43082=CARTESIAN_POINT('Ctrl Pts',(1.67945236653175,-1.,3.78796080021026));
#43083=CARTESIAN_POINT('Ctrl Pts',(1.67945236653175,1.,3.78796080021026));
#43084=CARTESIAN_POINT('Ctrl Pts',(1.67956789211943,-1.,3.78017178196859));
#43085=CARTESIAN_POINT('Ctrl Pts',(1.67956789211943,1.,3.78017178196859));
#43086=CARTESIAN_POINT('Ctrl Pts',(1.67964830084946,-1.,3.77239107928394));
#43087=CARTESIAN_POINT('Ctrl Pts',(1.67964830084946,1.,3.77239107928394));
#43088=CARTESIAN_POINT('Ctrl Pts',(1.67969332319322,-1.,3.76461886684523));
#43089=CARTESIAN_POINT('Ctrl Pts',(1.67969332319322,1.,3.76461886684523));
#43090=CARTESIAN_POINT('Ctrl Pts',(1.67970265841379,-1.,3.75685523754816));
#43091=CARTESIAN_POINT('Ctrl Pts',(1.67970265841379,1.,3.75685523754816));
#43092=CARTESIAN_POINT('Ctrl Pts',(1.67967598599665,-1.,3.74910022394845));
#43093=CARTESIAN_POINT('Ctrl Pts',(1.67967598599665,1.,3.74910022394845));
#43094=CARTESIAN_POINT('Ctrl Pts',(1.67961298685316,-1.,3.74135385965622));
#43095=CARTESIAN_POINT('Ctrl Pts',(1.67961298685316,1.,3.74135385965622));
#43096=CARTESIAN_POINT('Ctrl Pts',(1.67951336376434,-1.,3.73361623282617));
#43097=CARTESIAN_POINT('Ctrl Pts',(1.67951336376434,1.,3.73361623282617));
#43098=CARTESIAN_POINT('Ctrl Pts',(1.67937685856627,-1.,3.72588753416339));
#43099=CARTESIAN_POINT('Ctrl Pts',(1.67937685856627,1.,3.72588753416339));
#43100=CARTESIAN_POINT('Ctrl Pts',(1.6792032807165,-1.,3.71816812842188));
#43101=CARTESIAN_POINT('Ctrl Pts',(1.6792032807165,1.,3.71816812842188));
#43102=CARTESIAN_POINT('Ctrl Pts',(1.67899249793398,-1.,3.71045854208195));
#43103=CARTESIAN_POINT('Ctrl Pts',(1.67899249793398,1.,3.71045854208195));
#43104=CARTESIAN_POINT('Ctrl Pts',(1.6787443694862,-1.,3.70275932350998));
#43105=CARTESIAN_POINT('Ctrl Pts',(1.6787443694862,1.,3.70275932350998));
#43106=CARTESIAN_POINT('Ctrl Pts',(1.67845869064304,-1.,3.69507092759545));
#43107=CARTESIAN_POINT('Ctrl Pts',(1.67845869064304,1.,3.69507092759545));
#43108=CARTESIAN_POINT('Ctrl Pts',(1.67813513867973,-1.,3.68739360236505));
#43109=CARTESIAN_POINT('Ctrl Pts',(1.67813513867973,1.,3.68739360236505));
#43110=CARTESIAN_POINT('Ctrl Pts',(1.67777320475872,-1.,3.6797272457918));
#43111=CARTESIAN_POINT('Ctrl Pts',(1.67777320475872,1.,3.6797272457918));
#43112=CARTESIAN_POINT('Ctrl Pts',(1.67737217414901,-1.,3.67207136294639));
#43113=CARTESIAN_POINT('Ctrl Pts',(1.67737217414901,1.,3.67207136294639));
#43114=CARTESIAN_POINT('Ctrl Pts',(1.67693128053153,-1.,3.66442538671018));
#43115=CARTESIAN_POINT('Ctrl Pts',(1.67693128053153,1.,3.66442538671018));
#43116=CARTESIAN_POINT('Ctrl Pts',(1.67644983469459,-1.,3.65678894416442));
#43117=CARTESIAN_POINT('Ctrl Pts',(1.67644983469459,1.,3.65678894416442));
#43118=CARTESIAN_POINT('Ctrl Pts',(1.6759273594669,-1.,3.64916213574663));
#43119=CARTESIAN_POINT('Ctrl Pts',(1.6759273594669,1.,3.64916213574663));
#43120=CARTESIAN_POINT('Ctrl Pts',(1.67536373264839,-1.,3.6415458297232));
#43121=CARTESIAN_POINT('Ctrl Pts',(1.67536373264839,1.,3.6415458297232));
#43122=CARTESIAN_POINT('Ctrl Pts',(1.67475929882962,-1.,3.63394189312902));
#43123=CARTESIAN_POINT('Ctrl Pts',(1.67475929882962,1.,3.63394189312902));
#43124=CARTESIAN_POINT('Ctrl Pts',(1.67411452372265,-1.,3.62635249450908));
#43125=CARTESIAN_POINT('Ctrl Pts',(1.67411452372265,1.,3.62635249450908));
#43126=CARTESIAN_POINT('Ctrl Pts',(1.67342968196223,-1.,3.61877947398179));
#43127=CARTESIAN_POINT('Ctrl Pts',(1.67342968196223,1.,3.61877947398179));
#43128=CARTESIAN_POINT('Ctrl Pts',(1.67270452466968,-1.,3.61122367156182));
#43129=CARTESIAN_POINT('Ctrl Pts',(1.67270452466968,1.,3.61122367156182));
#43130=CARTESIAN_POINT('Ctrl Pts',(1.67193797318598,-1.,3.60368430815203));
#43131=CARTESIAN_POINT('Ctrl Pts',(1.67193797318598,1.,3.60368430815203));
#43132=CARTESIAN_POINT('Ctrl Pts',(1.67112775290706,-1.,3.59615824388808));
#43133=CARTESIAN_POINT('Ctrl Pts',(1.67112775290706,1.,3.59615824388808));
#43134=CARTESIAN_POINT('Ctrl Pts',(1.67027110397601,-1.,3.5886414309783));
#43135=CARTESIAN_POINT('Ctrl Pts',(1.67027110397601,1.,3.5886414309783));
#43136=CARTESIAN_POINT('Ctrl Pts',(1.66936552908228,-1.,3.58113044183823));
#43137=CARTESIAN_POINT('Ctrl Pts',(1.66936552908228,1.,3.58113044183823));
#43138=CARTESIAN_POINT('Ctrl Pts',(1.66840957407299,-1.,3.57362406285884));
#43139=CARTESIAN_POINT('Ctrl Pts',(1.66840957407299,1.,3.57362406285884));
#43140=CARTESIAN_POINT('Ctrl Pts',(1.66740349220308,-1.,3.56612465179429));
#43141=CARTESIAN_POINT('Ctrl Pts',(1.66740349220308,1.,3.56612465179429));
#43142=CARTESIAN_POINT('Ctrl Pts',(1.66635023293121,-1.,3.55864015233617));
#43143=CARTESIAN_POINT('Ctrl Pts',(1.66635023293121,1.,3.55864015233617));
#43144=CARTESIAN_POINT('Ctrl Pts',(1.66525401569004,-1.,3.5511812134288));
#43145=CARTESIAN_POINT('Ctrl Pts',(1.66525401569004,1.,3.5511812134288));
#43146=CARTESIAN_POINT('Ctrl Pts',(1.66411849222334,-1.,3.5437574747503));
#43147=CARTESIAN_POINT('Ctrl Pts',(1.66411849222334,1.,3.5437574747503));
#43148=CARTESIAN_POINT('Ctrl Pts',(1.66294490916113,-1.,3.53637385060225));
#43149=CARTESIAN_POINT('Ctrl Pts',(1.66294490916113,1.,3.53637385060225));
#43150=CARTESIAN_POINT('Ctrl Pts',(1.66173058912365,-1.,3.52902746211082));
#43151=CARTESIAN_POINT('Ctrl Pts',(1.66173058912365,1.,3.52902746211082));
#43152=CARTESIAN_POINT('Ctrl Pts',(1.66046645222266,-1.,3.52170261543787));
#43153=CARTESIAN_POINT('Ctrl Pts',(1.66046645222266,1.,3.52170261543787));
#43154=CARTESIAN_POINT('Ctrl Pts',(1.65913971687324,-1.,3.51437632188903));
#43155=CARTESIAN_POINT('Ctrl Pts',(1.65913971687324,1.,3.51437632188903));
#43156=CARTESIAN_POINT('Ctrl Pts',(1.65773832633617,-1.,3.5070273314651));
#43157=CARTESIAN_POINT('Ctrl Pts',(1.65773832633617,1.,3.5070273314651));
#43158=CARTESIAN_POINT('Ctrl Pts',(1.65625517961583,-1.,3.49964476477929));
#43159=CARTESIAN_POINT('Ctrl Pts',(1.65625517961583,1.,3.49964476477929));
#43160=CARTESIAN_POINT('Ctrl Pts',(1.65469162644476,-1.,3.49223525300194));
#43161=CARTESIAN_POINT('Ctrl Pts',(1.65469162644476,1.,3.49223525300194));
#43162=CARTESIAN_POINT('Ctrl Pts',(1.65306335367762,-1.,3.48483492840942));
#43163=CARTESIAN_POINT('Ctrl Pts',(1.65306335367762,1.,3.48483492840942));
#43164=CARTESIAN_POINT('Ctrl Pts',(1.65139534930353,-1.,3.47749926256543));
#43165=CARTESIAN_POINT('Ctrl Pts',(1.65139534930353,1.,3.47749926256543));
#43166=CARTESIAN_POINT('Ctrl Pts',(1.64971118698285,-1.,3.47028140996055));
#43167=CARTESIAN_POINT('Ctrl Pts',(1.64971118698285,1.,3.47028140996055));
#43168=CARTESIAN_POINT('Ctrl Pts',(1.64802323352752,-1.,3.46321237515029));
#43169=CARTESIAN_POINT('Ctrl Pts',(1.64802323352752,1.,3.46321237515029));
#43170=CARTESIAN_POINT('Ctrl Pts',(1.64632429697506,-1.,3.4562842106239));
#43171=CARTESIAN_POINT('Ctrl Pts',(1.64632429697506,1.,3.4562842106239));
#43172=CARTESIAN_POINT('Ctrl Pts',(1.64457408708059,-1.,3.44942242546693));
#43173=CARTESIAN_POINT('Ctrl Pts',(1.64457408708059,1.,3.44942242546693));
#43174=CARTESIAN_POINT('Ctrl Pts',(1.64270733821042,-1.,3.44250337701736));
#43175=CARTESIAN_POINT('Ctrl Pts',(1.64270733821042,1.,3.44250337701736));
#43176=CARTESIAN_POINT('Ctrl Pts',(1.64065778701952,-1.,3.43540451921397));
#43177=CARTESIAN_POINT('Ctrl Pts',(1.64065778701952,1.,3.43540451921397));
#43178=CARTESIAN_POINT('Ctrl Pts',(1.6383787624689,-1.,3.42804772926214));
#43179=CARTESIAN_POINT('Ctrl Pts',(1.6383787624689,1.,3.42804772926214));
#43180=CARTESIAN_POINT('Ctrl Pts',(1.63586250099804,-1.,3.4204397459095));
#43181=CARTESIAN_POINT('Ctrl Pts',(1.63586250099804,1.,3.4204397459095));
#43182=CARTESIAN_POINT('Ctrl Pts',(1.63316667054156,-1.,3.41272817148719));
#43183=CARTESIAN_POINT('Ctrl Pts',(1.63316667054156,1.,3.41272817148719));
#43184=CARTESIAN_POINT('Ctrl Pts',(1.63041148964996,-1.,3.40519422740596));
#43185=CARTESIAN_POINT('Ctrl Pts',(1.63041148964996,1.,3.40519422740596));
#43186=CARTESIAN_POINT('Ctrl Pts',(1.62774916464571,-1.,3.39818605298342));
#43187=CARTESIAN_POINT('Ctrl Pts',(1.62774916464571,1.,3.39818605298342));
#43188=CARTESIAN_POINT('Ctrl Pts',(1.62533996116793,-1.,3.39206617497078));
#43189=CARTESIAN_POINT('Ctrl Pts',(1.62533996116793,1.,3.39206617497078));
#43190=CARTESIAN_POINT('Ctrl Pts',(1.62332788556183,-1.,3.38715832178929));
#43191=CARTESIAN_POINT('Ctrl Pts',(1.62332788556183,1.,3.38715832178929));
#43192=CARTESIAN_POINT('Ctrl Pts',(1.62181089631134,-1.,3.38368201668123));
#43193=CARTESIAN_POINT('Ctrl Pts',(1.62181089631134,1.,3.38368201668123));
#43194=CARTESIAN_POINT('Ctrl Pts',(1.62103022180917,-1.,3.38212861099481));
#43195=CARTESIAN_POINT('Ctrl Pts',(1.62103022180917,1.,3.38212861099481));
#43196=CARTESIAN_POINT('Ctrl Pts',(1.6206953236804,-1.,3.38166984193496));
#43197=CARTESIAN_POINT('Ctrl Pts',(1.6206953236804,1.,3.38166984193496));
#43198=CARTESIAN_POINT('Ctrl Pts',(1.62058335162421,-1.,3.38167767992546));
#43199=CARTESIAN_POINT('Ctrl Pts',(1.62058335162421,1.,3.38167767992546));
#43200=CARTESIAN_POINT('Ctrl Pts',(1.62055519152808,-1.,3.38176002566879));
#43201=CARTESIAN_POINT('Ctrl Pts',(1.62055519152808,1.,3.38176002566879));
#43202=CARTESIAN_POINT('',(1.67727921511438,1.,3.85054988729471));
#43203=CARTESIAN_POINT('Ctrl Pts',(1.67727921511438,1.,3.85054988729471));
#43204=CARTESIAN_POINT('Ctrl Pts',(1.6773605765671,1.,3.84897939431104));
#43205=CARTESIAN_POINT('Ctrl Pts',(1.67751991140661,1.,3.84583912297567));
#43206=CARTESIAN_POINT('Ctrl Pts',(1.67774874946867,1.,3.8411308598706));
#43207=CARTESIAN_POINT('Ctrl Pts',(1.67803353065273,1.,3.83485746516115));
#43208=CARTESIAN_POINT('Ctrl Pts',(1.67835555760094,1.,3.82702289288453));
#43209=CARTESIAN_POINT('Ctrl Pts',(1.67864354606363,1.,3.81919554100522));
#43210=CARTESIAN_POINT('Ctrl Pts',(1.67889737738311,1.,3.81137549624273));
#43211=CARTESIAN_POINT('Ctrl Pts',(1.67911690648128,1.,3.80356289078481));
#43212=CARTESIAN_POINT('Ctrl Pts',(1.67930196625203,1.,3.7957579157763));
#43213=CARTESIAN_POINT('Ctrl Pts',(1.67945236653175,1.,3.78796080021026));
#43214=CARTESIAN_POINT('Ctrl Pts',(1.67956789211943,1.,3.78017178196859));
#43215=CARTESIAN_POINT('Ctrl Pts',(1.67964830084946,1.,3.77239107928394));
#43216=CARTESIAN_POINT('Ctrl Pts',(1.67969332319322,1.,3.76461886684523));
#43217=CARTESIAN_POINT('Ctrl Pts',(1.67970265841379,1.,3.75685523754816));
#43218=CARTESIAN_POINT('Ctrl Pts',(1.67967598599665,1.,3.74910022394845));
#43219=CARTESIAN_POINT('Ctrl Pts',(1.67961298685316,1.,3.74135385965622));
#43220=CARTESIAN_POINT('Ctrl Pts',(1.67951336376434,1.,3.73361623282617));
#43221=CARTESIAN_POINT('Ctrl Pts',(1.67937685856627,1.,3.72588753416339));
#43222=CARTESIAN_POINT('Ctrl Pts',(1.6792032807165,1.,3.71816812842188));
#43223=CARTESIAN_POINT('Ctrl Pts',(1.67899249793398,1.,3.71045854208195));
#43224=CARTESIAN_POINT('Ctrl Pts',(1.6787443694862,1.,3.70275932350998));
#43225=CARTESIAN_POINT('Ctrl Pts',(1.67845869064304,1.,3.69507092759545));
#43226=CARTESIAN_POINT('Ctrl Pts',(1.67813513867973,1.,3.68739360236505));
#43227=CARTESIAN_POINT('Ctrl Pts',(1.67777320475872,1.,3.6797272457918));
#43228=CARTESIAN_POINT('Ctrl Pts',(1.67737217414901,1.,3.67207136294639));
#43229=CARTESIAN_POINT('Ctrl Pts',(1.67693128053153,1.,3.66442538671018));
#43230=CARTESIAN_POINT('Ctrl Pts',(1.67644983469459,1.,3.65678894416442));
#43231=CARTESIAN_POINT('Ctrl Pts',(1.6759273594669,1.,3.64916213574663));
#43232=CARTESIAN_POINT('Ctrl Pts',(1.67536373264839,1.,3.6415458297232));
#43233=CARTESIAN_POINT('Ctrl Pts',(1.67475929882962,1.,3.63394189312902));
#43234=CARTESIAN_POINT('Ctrl Pts',(1.67411452372265,1.,3.62635249450908));
#43235=CARTESIAN_POINT('Ctrl Pts',(1.67342968196223,1.,3.61877947398179));
#43236=CARTESIAN_POINT('Ctrl Pts',(1.67270452466968,1.,3.61122367156182));
#43237=CARTESIAN_POINT('Ctrl Pts',(1.67193797318598,1.,3.60368430815203));
#43238=CARTESIAN_POINT('Ctrl Pts',(1.67112775290706,1.,3.59615824388808));
#43239=CARTESIAN_POINT('Ctrl Pts',(1.67027110397601,1.,3.5886414309783));
#43240=CARTESIAN_POINT('Ctrl Pts',(1.66936552908228,1.,3.58113044183823));
#43241=CARTESIAN_POINT('Ctrl Pts',(1.66840957407299,1.,3.57362406285884));
#43242=CARTESIAN_POINT('Ctrl Pts',(1.66740349220308,1.,3.56612465179429));
#43243=CARTESIAN_POINT('Ctrl Pts',(1.66635023293121,1.,3.55864015233617));
#43244=CARTESIAN_POINT('Ctrl Pts',(1.66525401569004,1.,3.5511812134288));
#43245=CARTESIAN_POINT('Ctrl Pts',(1.66411849222334,1.,3.5437574747503));
#43246=CARTESIAN_POINT('Ctrl Pts',(1.66294490916113,1.,3.53637385060225));
#43247=CARTESIAN_POINT('Ctrl Pts',(1.66173058912365,1.,3.52902746211082));
#43248=CARTESIAN_POINT('Ctrl Pts',(1.66046645222266,1.,3.52170261543787));
#43249=CARTESIAN_POINT('Ctrl Pts',(1.65913971687324,1.,3.51437632188903));
#43250=CARTESIAN_POINT('Ctrl Pts',(1.65773832633617,1.,3.5070273314651));
#43251=CARTESIAN_POINT('Ctrl Pts',(1.65625517961583,1.,3.49964476477929));
#43252=CARTESIAN_POINT('Ctrl Pts',(1.65469162644476,1.,3.49223525300194));
#43253=CARTESIAN_POINT('Ctrl Pts',(1.65306335367762,1.,3.48483492840942));
#43254=CARTESIAN_POINT('Ctrl Pts',(1.65139534930353,1.,3.47749926256543));
#43255=CARTESIAN_POINT('Ctrl Pts',(1.64971118698285,1.,3.47028140996055));
#43256=CARTESIAN_POINT('Ctrl Pts',(1.64802323352752,1.,3.46321237515029));
#43257=CARTESIAN_POINT('Ctrl Pts',(1.64632429697506,1.,3.4562842106239));
#43258=CARTESIAN_POINT('Ctrl Pts',(1.64457408708059,1.,3.44942242546693));
#43259=CARTESIAN_POINT('Ctrl Pts',(1.64270733821042,1.,3.44250337701736));
#43260=CARTESIAN_POINT('Ctrl Pts',(1.64065778701952,1.,3.43540451921397));
#43261=CARTESIAN_POINT('Ctrl Pts',(1.6383787624689,1.,3.42804772926214));
#43262=CARTESIAN_POINT('Ctrl Pts',(1.63586250099804,1.,3.4204397459095));
#43263=CARTESIAN_POINT('Ctrl Pts',(1.63316667054156,1.,3.41272817148719));
#43264=CARTESIAN_POINT('Ctrl Pts',(1.63041148964996,1.,3.40519422740596));
#43265=CARTESIAN_POINT('Ctrl Pts',(1.62774916464571,1.,3.39818605298342));
#43266=CARTESIAN_POINT('Ctrl Pts',(1.62533996116793,1.,3.39206617497078));
#43267=CARTESIAN_POINT('Ctrl Pts',(1.62332788556183,1.,3.38715832178929));
#43268=CARTESIAN_POINT('Ctrl Pts',(1.62192472202795,1.,3.3839428576331));
#43269=CARTESIAN_POINT('Ctrl Pts',(1.62118047294574,1.,3.38243080602536));
#43270=CARTESIAN_POINT('Ctrl Pts',(1.62083271136059,1.,3.38187506457001));
#43271=CARTESIAN_POINT('Ctrl Pts',(1.62069086551626,1.,3.38173802621243));
#43272=CARTESIAN_POINT('Ctrl Pts',(1.62064718014256,1.,3.38171594275687));
#43273=CARTESIAN_POINT('',(1.67727921511438,0.,3.85054988729471));
#43274=CARTESIAN_POINT('Ctrl Pts',(1.24535988127942,-1.,3.53717101171257));
#43275=CARTESIAN_POINT('Ctrl Pts',(1.24535988127942,1.,3.53717101171257));
#43276=CARTESIAN_POINT('Ctrl Pts',(1.24528174185147,-1.,3.53713269667534));
#43277=CARTESIAN_POINT('Ctrl Pts',(1.24528174185147,1.,3.53713269667534));
#43278=CARTESIAN_POINT('Ctrl Pts',(1.2451970233558,-1.,3.53720633058152));
#43279=CARTESIAN_POINT('Ctrl Pts',(1.2451970233558,1.,3.53720633058152));
#43280=CARTESIAN_POINT('Ctrl Pts',(1.24528461333177,-1.,3.53776753803428));
#43281=CARTESIAN_POINT('Ctrl Pts',(1.24528461333177,1.,3.53776753803428));
#43282=CARTESIAN_POINT('Ctrl Pts',(1.24583101679199,-1.,3.53941798196293));
#43283=CARTESIAN_POINT('Ctrl Pts',(1.24583101679199,1.,3.53941798196293));
#43284=CARTESIAN_POINT('Ctrl Pts',(1.2472164623202,-1.,3.54294877426113));
#43285=CARTESIAN_POINT('Ctrl Pts',(1.2472164623202,1.,3.54294877426113));
#43286=CARTESIAN_POINT('Ctrl Pts',(1.24926408627938,-1.,3.54784190282889));
#43287=CARTESIAN_POINT('Ctrl Pts',(1.24926408627938,1.,3.54784190282889));
#43288=CARTESIAN_POINT('Ctrl Pts',(1.25188792940508,-1.,3.5538728741862));
#43289=CARTESIAN_POINT('Ctrl Pts',(1.25188792940508,1.,3.5538728741862));
#43290=CARTESIAN_POINT('Ctrl Pts',(1.25496090899873,-1.,3.56071094990825));
#43291=CARTESIAN_POINT('Ctrl Pts',(1.25496090899873,1.,3.56071094990825));
#43292=CARTESIAN_POINT('Ctrl Pts',(1.25834000485626,-1.,3.56798645995025));
#43293=CARTESIAN_POINT('Ctrl Pts',(1.25834000485626,1.,3.56798645995025));
#43294=CARTESIAN_POINT('Ctrl Pts',(1.26188667142784,-1.,3.5753456065164));
#43295=CARTESIAN_POINT('Ctrl Pts',(1.26188667142784,1.,3.5753456065164));
#43296=CARTESIAN_POINT('Ctrl Pts',(1.26548706249891,-1.,3.58250452868699));
#43297=CARTESIAN_POINT('Ctrl Pts',(1.26548706249891,1.,3.58250452868699));
#43298=CARTESIAN_POINT('Ctrl Pts',(1.26907758484766,-1.,3.5893180784647));
#43299=CARTESIAN_POINT('Ctrl Pts',(1.26907758484766,1.,3.5893180784647));
#43300=CARTESIAN_POINT('Ctrl Pts',(1.27264798379365,-1.,3.59578698050164));
#43301=CARTESIAN_POINT('Ctrl Pts',(1.27264798379365,1.,3.59578698050164));
#43302=CARTESIAN_POINT('Ctrl Pts',(1.27622049908664,-1.,3.60199947736404));
#43303=CARTESIAN_POINT('Ctrl Pts',(1.27622049908664,1.,3.60199947736404));
#43304=CARTESIAN_POINT('Ctrl Pts',(1.27983492861703,-1.,3.60808907746372));
#43305=CARTESIAN_POINT('Ctrl Pts',(1.27983492861703,1.,3.60808907746372));
#43306=CARTESIAN_POINT('Ctrl Pts',(1.28353255117754,-1.,3.61418935913793));
#43307=CARTESIAN_POINT('Ctrl Pts',(1.28353255117754,1.,3.61418935913793));
#43308=CARTESIAN_POINT('Ctrl Pts',(1.2873375502936,-1.,3.62038148492295));
#43309=CARTESIAN_POINT('Ctrl Pts',(1.2873375502936,1.,3.62038148492295));
#43310=CARTESIAN_POINT('Ctrl Pts',(1.29125046021853,-1.,3.62667616004299));
#43311=CARTESIAN_POINT('Ctrl Pts',(1.29125046021853,1.,3.62667616004299));
#43312=CARTESIAN_POINT('Ctrl Pts',(1.29525810207744,-1.,3.63304271630995));
#43313=CARTESIAN_POINT('Ctrl Pts',(1.29525810207744,1.,3.63304271630995));
#43314=CARTESIAN_POINT('Ctrl Pts',(1.29933955906463,-1.,3.6394268987279));
#43315=CARTESIAN_POINT('Ctrl Pts',(1.29933955906463,1.,3.6394268987279));
#43316=CARTESIAN_POINT('Ctrl Pts',(1.30347327603778,-1.,3.64577181380125));
#43317=CARTESIAN_POINT('Ctrl Pts',(1.30347327603778,1.,3.64577181380125));
#43318=CARTESIAN_POINT('Ctrl Pts',(1.30764479590051,-1.,3.65204081987101));
#43319=CARTESIAN_POINT('Ctrl Pts',(1.30764479590051,1.,3.65204081987101));
#43320=CARTESIAN_POINT('Ctrl Pts',(1.31185038411231,-1.,3.65822827358655));
#43321=CARTESIAN_POINT('Ctrl Pts',(1.31185038411231,1.,3.65822827358655));
#43322=CARTESIAN_POINT('Ctrl Pts',(1.31609271239922,-1.,3.66434688899822));
#43323=CARTESIAN_POINT('Ctrl Pts',(1.31609271239922,1.,3.66434688899822));
#43324=CARTESIAN_POINT('Ctrl Pts',(1.3203782813777,-1.,3.67042021752668));
#43325=CARTESIAN_POINT('Ctrl Pts',(1.3203782813777,1.,3.67042021752668));
#43326=CARTESIAN_POINT('Ctrl Pts',(1.32471430856413,-1.,3.67647355257906));
#43327=CARTESIAN_POINT('Ctrl Pts',(1.32471430856413,1.,3.67647355257906));
#43328=CARTESIAN_POINT('Ctrl Pts',(1.32910547072734,-1.,3.68252441182534));
#43329=CARTESIAN_POINT('Ctrl Pts',(1.32910547072734,1.,3.68252441182534));
#43330=CARTESIAN_POINT('Ctrl Pts',(1.33355191034515,-1.,3.68857672413013));
#43331=CARTESIAN_POINT('Ctrl Pts',(1.33355191034515,1.,3.68857672413013));
#43332=CARTESIAN_POINT('Ctrl Pts',(1.33805103398214,-1.,3.69462613305692));
#43333=CARTESIAN_POINT('Ctrl Pts',(1.33805103398214,1.,3.69462613305692));
#43334=CARTESIAN_POINT('Ctrl Pts',(1.3425986075293,-1.,3.70066324015112));
#43335=CARTESIAN_POINT('Ctrl Pts',(1.3425986075293,1.,3.70066324015112));
#43336=CARTESIAN_POINT('Ctrl Pts',(1.34719008463535,-1.,3.7066775318825));
#43337=CARTESIAN_POINT('Ctrl Pts',(1.34719008463535,1.,3.7066775318825));
#43338=CARTESIAN_POINT('Ctrl Pts',(1.35182193384426,-1.,3.71266130563061));
#43339=CARTESIAN_POINT('Ctrl Pts',(1.35182193384426,1.,3.71266130563061));
#43340=CARTESIAN_POINT('Ctrl Pts',(1.35649266705038,-1.,3.71861271513318));
#43341=CARTESIAN_POINT('Ctrl Pts',(1.35649266705038,1.,3.71861271513318));
#43342=CARTESIAN_POINT('Ctrl Pts',(1.36120211416353,-1.,3.72453364678279));
#43343=CARTESIAN_POINT('Ctrl Pts',(1.36120211416353,1.,3.72453364678279));
#43344=CARTESIAN_POINT('Ctrl Pts',(1.36595093298674,-1.,3.73042829011293));
#43345=CARTESIAN_POINT('Ctrl Pts',(1.36595093298674,1.,3.73042829011293));
#43346=CARTESIAN_POINT('Ctrl Pts',(1.37074003422739,-1.,3.73630145885809));
#43347=CARTESIAN_POINT('Ctrl Pts',(1.37074003422739,1.,3.73630145885809));
#43348=CARTESIAN_POINT('Ctrl Pts',(1.3755700297169,-1.,3.7421569816256));
#43349=CARTESIAN_POINT('Ctrl Pts',(1.3755700297169,1.,3.7421569816256));
#43350=CARTESIAN_POINT('Ctrl Pts',(1.38044070763302,-1.,3.74799617204744));
#43351=CARTESIAN_POINT('Ctrl Pts',(1.38044070763302,1.,3.74799617204744));
#43352=CARTESIAN_POINT('Ctrl Pts',(1.38535129801185,-1.,3.75381861212728));
#43353=CARTESIAN_POINT('Ctrl Pts',(1.38535129801185,1.,3.75381861212728));
#43354=CARTESIAN_POINT('Ctrl Pts',(1.39030069388926,-1.,3.75962280650875));
#43355=CARTESIAN_POINT('Ctrl Pts',(1.39030069388926,1.,3.75962280650875));
#43356=CARTESIAN_POINT('Ctrl Pts',(1.39528769118054,-1.,3.76540689249078));
#43357=CARTESIAN_POINT('Ctrl Pts',(1.39528769118054,1.,3.76540689249078));
#43358=CARTESIAN_POINT('Ctrl Pts',(1.40031121335495,-1.,3.77116930621804));
#43359=CARTESIAN_POINT('Ctrl Pts',(1.40031121335495,1.,3.77116930621804));
#43360=CARTESIAN_POINT('Ctrl Pts',(1.40537056004702,-1.,3.77690952014209));
#43361=CARTESIAN_POINT('Ctrl Pts',(1.40537056004702,1.,3.77690952014209));
#43362=CARTESIAN_POINT('Ctrl Pts',(1.41046532282567,-1.,3.78262780065406));
#43363=CARTESIAN_POINT('Ctrl Pts',(1.41046532282567,1.,3.78262780065406));
#43364=CARTESIAN_POINT('Ctrl Pts',(1.41559527803808,-1.,3.78832489879369));
#43365=CARTESIAN_POINT('Ctrl Pts',(1.41559527803808,1.,3.78832489879369));
#43366=CARTESIAN_POINT('Ctrl Pts',(1.42076028482828,-1.,3.7940017574439));
#43367=CARTESIAN_POINT('Ctrl Pts',(1.42076028482828,1.,3.7940017574439));
#43368=CARTESIAN_POINT('Ctrl Pts',(1.42596018777301,-1.,3.79965923196365));
#43369=CARTESIAN_POINT('Ctrl Pts',(1.42596018777301,1.,3.79965923196365));
#43370=CARTESIAN_POINT('Ctrl Pts',(1.43119469921364,-1.,3.80529775429916));
#43371=CARTESIAN_POINT('Ctrl Pts',(1.43119469921364,1.,3.80529775429916));
#43372=CARTESIAN_POINT('Ctrl Pts',(1.43646341556783,-1.,3.81091737726965));
#43373=CARTESIAN_POINT('Ctrl Pts',(1.43646341556783,1.,3.81091737726965));
#43374=CARTESIAN_POINT('Ctrl Pts',(1.441765870414,-1.,3.8165179239855));
#43375=CARTESIAN_POINT('Ctrl Pts',(1.441765870414,1.,3.8165179239855));
#43376=CARTESIAN_POINT('Ctrl Pts',(1.44710157648562,-1.,3.82209910620591));
#43377=CARTESIAN_POINT('Ctrl Pts',(1.44710157648562,1.,3.82209910620591));
#43378=CARTESIAN_POINT('Ctrl Pts',(1.45247006796807,-1.,3.82766064519));
#43379=CARTESIAN_POINT('Ctrl Pts',(1.45247006796807,1.,3.82766064519));
#43380=CARTESIAN_POINT('Ctrl Pts',(1.45787095220763,-1.,3.83320241775199));
#43381=CARTESIAN_POINT('Ctrl Pts',(1.45787095220763,1.,3.83320241775199));
#43382=CARTESIAN_POINT('Ctrl Pts',(1.46330391180621,-1.,3.83872447159309));
#43383=CARTESIAN_POINT('Ctrl Pts',(1.46330391180621,1.,3.83872447159309));
#43384=CARTESIAN_POINT('Ctrl Pts',(1.46876867426374,-1.,3.84422695454469));
#43385=CARTESIAN_POINT('Ctrl Pts',(1.46876867426374,1.,3.84422695454469));
#43386=CARTESIAN_POINT('Ctrl Pts',(1.47426499018467,-1.,3.84971006847096));
#43387=CARTESIAN_POINT('Ctrl Pts',(1.47426499018467,1.,3.84971006847096));
#43388=CARTESIAN_POINT('Ctrl Pts',(1.47979260991063,-1.,3.85517401698952));
#43389=CARTESIAN_POINT('Ctrl Pts',(1.47979260991063,1.,3.85517401698952));
#43390=CARTESIAN_POINT('Ctrl Pts',(1.48535125510102,-1.,3.86061894706551));
#43391=CARTESIAN_POINT('Ctrl Pts',(1.48535125510102,1.,3.86061894706551));
#43392=CARTESIAN_POINT('Ctrl Pts',(1.49094061164604,-1.,3.86604492575933));
#43393=CARTESIAN_POINT('Ctrl Pts',(1.49094061164604,1.,3.86604492575933));
#43394=CARTESIAN_POINT('Ctrl Pts',(1.4965603539944,-1.,3.8714519699927));
#43395=CARTESIAN_POINT('Ctrl Pts',(1.4965603539944,1.,3.8714519699927));
#43396=CARTESIAN_POINT('Ctrl Pts',(1.50221016176766,-1.,3.87684006372665));
#43397=CARTESIAN_POINT('Ctrl Pts',(1.50221016176766,1.,3.87684006372665));
#43398=CARTESIAN_POINT('Ctrl Pts',(1.50788973857719,-1.,3.88220917950443));
#43399=CARTESIAN_POINT('Ctrl Pts',(1.50788973857719,1.,3.88220917950443));
#43400=CARTESIAN_POINT('Ctrl Pts',(1.51359883110181,-1.,3.88755930032927));
#43401=CARTESIAN_POINT('Ctrl Pts',(1.51359883110181,1.,3.88755930032927));
#43402=CARTESIAN_POINT('Ctrl Pts',(1.51933724328609,-1.,3.89289043531893));
#43403=CARTESIAN_POINT('Ctrl Pts',(1.51933724328609,1.,3.89289043531893));
#43404=CARTESIAN_POINT('Ctrl Pts',(1.52510482990784,-1.,3.8982026070607));
#43405=CARTESIAN_POINT('Ctrl Pts',(1.52510482990784,1.,3.8982026070607));
#43406=CARTESIAN_POINT('Ctrl Pts',(1.5297421605556,-1.,3.90243719629755));
#43407=CARTESIAN_POINT('Ctrl Pts',(1.5297421605556,1.,3.90243719629755));
#43408=CARTESIAN_POINT('Ctrl Pts',(1.53323321827311,-1.,3.90560462812846));
#43409=CARTESIAN_POINT('Ctrl Pts',(1.53323321827311,1.,3.90560462812846));
#43410=CARTESIAN_POINT('Ctrl Pts',(1.53556639217742,-1.,3.90771246854607));
#43411=CARTESIAN_POINT('Ctrl Pts',(1.53556639217742,1.,3.90771246854607));
#43412=CARTESIAN_POINT('Ctrl Pts',(1.53673442965255,-1.,3.90876544355381));
#43413=CARTESIAN_POINT('Ctrl Pts',(1.53673442965255,1.,3.90876544355381));
#43414=CARTESIAN_POINT('',(1.24526366418208,1.,3.5372048861591));
#43415=CARTESIAN_POINT('Ctrl Pts',(1.24526366418208,-1.,3.5372048861591));
#43416=CARTESIAN_POINT('Ctrl Pts',(1.24526366418208,-0.666666666666667,
3.5372048861591));
#43417=CARTESIAN_POINT('Ctrl Pts',(1.24526366418208,-0.333333333333333,
3.5372048861591));
#43418=CARTESIAN_POINT('Ctrl Pts',(1.24526366418208,0.333333333333333,3.5372048861591));
#43419=CARTESIAN_POINT('Ctrl Pts',(1.24526366418208,0.666666666666667,3.5372048861591));
#43420=CARTESIAN_POINT('Ctrl Pts',(1.24526366418208,1.,3.5372048861591));
#43421=CARTESIAN_POINT('',(1.53673442965255,1.,3.90876544355381));
#43422=CARTESIAN_POINT('',(1.53673442965255,0.,3.90876544355381));
#43423=CARTESIAN_POINT('Ctrl Pts',(1.24526366418208,1.,3.5372048861591));
#43424=CARTESIAN_POINT('Ctrl Pts',(1.24524838931864,1.,3.53725139174402));
#43425=CARTESIAN_POINT('Ctrl Pts',(1.24524498991133,1.,3.53744859265385));
#43426=CARTESIAN_POINT('Ctrl Pts',(1.2453920538873,1.,3.53808746578052));
#43427=CARTESIAN_POINT('Ctrl Pts',(1.24593497225964,1.,3.53968291129942));
#43428=CARTESIAN_POINT('Ctrl Pts',(1.2472164623202,1.,3.54294877426113));
#43429=CARTESIAN_POINT('Ctrl Pts',(1.24926408627938,1.,3.54784190282889));
#43430=CARTESIAN_POINT('Ctrl Pts',(1.25188792940508,1.,3.5538728741862));
#43431=CARTESIAN_POINT('Ctrl Pts',(1.25496090899873,1.,3.56071094990825));
#43432=CARTESIAN_POINT('Ctrl Pts',(1.25834000485626,1.,3.56798645995025));
#43433=CARTESIAN_POINT('Ctrl Pts',(1.26188667142784,1.,3.5753456065164));
#43434=CARTESIAN_POINT('Ctrl Pts',(1.26548706249891,1.,3.58250452868699));
#43435=CARTESIAN_POINT('Ctrl Pts',(1.26907758484766,1.,3.5893180784647));
#43436=CARTESIAN_POINT('Ctrl Pts',(1.27264798379365,1.,3.59578698050164));
#43437=CARTESIAN_POINT('Ctrl Pts',(1.27622049908664,1.,3.60199947736404));
#43438=CARTESIAN_POINT('Ctrl Pts',(1.27983492861703,1.,3.60808907746372));
#43439=CARTESIAN_POINT('Ctrl Pts',(1.28353255117754,1.,3.61418935913793));
#43440=CARTESIAN_POINT('Ctrl Pts',(1.2873375502936,1.,3.62038148492295));
#43441=CARTESIAN_POINT('Ctrl Pts',(1.29125046021853,1.,3.62667616004299));
#43442=CARTESIAN_POINT('Ctrl Pts',(1.29525810207744,1.,3.63304271630995));
#43443=CARTESIAN_POINT('Ctrl Pts',(1.29933955906463,1.,3.6394268987279));
#43444=CARTESIAN_POINT('Ctrl Pts',(1.30347327603778,1.,3.64577181380125));
#43445=CARTESIAN_POINT('Ctrl Pts',(1.30764479590051,1.,3.65204081987101));
#43446=CARTESIAN_POINT('Ctrl Pts',(1.31185038411231,1.,3.65822827358655));
#43447=CARTESIAN_POINT('Ctrl Pts',(1.31609271239922,1.,3.66434688899822));
#43448=CARTESIAN_POINT('Ctrl Pts',(1.3203782813777,1.,3.67042021752668));
#43449=CARTESIAN_POINT('Ctrl Pts',(1.32471430856413,1.,3.67647355257906));
#43450=CARTESIAN_POINT('Ctrl Pts',(1.32910547072734,1.,3.68252441182534));
#43451=CARTESIAN_POINT('Ctrl Pts',(1.33355191034515,1.,3.68857672413013));
#43452=CARTESIAN_POINT('Ctrl Pts',(1.33805103398214,1.,3.69462613305692));
#43453=CARTESIAN_POINT('Ctrl Pts',(1.3425986075293,1.,3.70066324015112));
#43454=CARTESIAN_POINT('Ctrl Pts',(1.34719008463535,1.,3.7066775318825));
#43455=CARTESIAN_POINT('Ctrl Pts',(1.35182193384426,1.,3.71266130563061));
#43456=CARTESIAN_POINT('Ctrl Pts',(1.35649266705038,1.,3.71861271513318));
#43457=CARTESIAN_POINT('Ctrl Pts',(1.36120211416353,1.,3.72453364678279));
#43458=CARTESIAN_POINT('Ctrl Pts',(1.36595093298674,1.,3.73042829011293));
#43459=CARTESIAN_POINT('Ctrl Pts',(1.37074003422739,1.,3.73630145885809));
#43460=CARTESIAN_POINT('Ctrl Pts',(1.3755700297169,1.,3.7421569816256));
#43461=CARTESIAN_POINT('Ctrl Pts',(1.38044070763302,1.,3.74799617204744));
#43462=CARTESIAN_POINT('Ctrl Pts',(1.38535129801185,1.,3.75381861212728));
#43463=CARTESIAN_POINT('Ctrl Pts',(1.39030069388926,1.,3.75962280650875));
#43464=CARTESIAN_POINT('Ctrl Pts',(1.39528769118054,1.,3.76540689249078));
#43465=CARTESIAN_POINT('Ctrl Pts',(1.40031121335495,1.,3.77116930621804));
#43466=CARTESIAN_POINT('Ctrl Pts',(1.40537056004702,1.,3.77690952014209));
#43467=CARTESIAN_POINT('Ctrl Pts',(1.41046532282567,1.,3.78262780065406));
#43468=CARTESIAN_POINT('Ctrl Pts',(1.41559527803808,1.,3.78832489879369));
#43469=CARTESIAN_POINT('Ctrl Pts',(1.42076028482828,1.,3.7940017574439));
#43470=CARTESIAN_POINT('Ctrl Pts',(1.42596018777301,1.,3.79965923196365));
#43471=CARTESIAN_POINT('Ctrl Pts',(1.43119469921364,1.,3.80529775429916));
#43472=CARTESIAN_POINT('Ctrl Pts',(1.43646341556783,1.,3.81091737726965));
#43473=CARTESIAN_POINT('Ctrl Pts',(1.441765870414,1.,3.8165179239855));
#43474=CARTESIAN_POINT('Ctrl Pts',(1.44710157648562,1.,3.82209910620591));
#43475=CARTESIAN_POINT('Ctrl Pts',(1.45247006796807,1.,3.82766064519));
#43476=CARTESIAN_POINT('Ctrl Pts',(1.45787095220763,1.,3.83320241775199));
#43477=CARTESIAN_POINT('Ctrl Pts',(1.46330391180621,1.,3.83872447159309));
#43478=CARTESIAN_POINT('Ctrl Pts',(1.46876867426374,1.,3.84422695454469));
#43479=CARTESIAN_POINT('Ctrl Pts',(1.47426499018467,1.,3.84971006847096));
#43480=CARTESIAN_POINT('Ctrl Pts',(1.47979260991063,1.,3.85517401698952));
#43481=CARTESIAN_POINT('Ctrl Pts',(1.48535125510102,1.,3.86061894706551));
#43482=CARTESIAN_POINT('Ctrl Pts',(1.49094061164604,1.,3.86604492575933));
#43483=CARTESIAN_POINT('Ctrl Pts',(1.4965603539944,1.,3.8714519699927));
#43484=CARTESIAN_POINT('Ctrl Pts',(1.50221016176766,1.,3.87684006372665));
#43485=CARTESIAN_POINT('Ctrl Pts',(1.50788973857719,1.,3.88220917950443));
#43486=CARTESIAN_POINT('Ctrl Pts',(1.51359883110181,1.,3.88755930032927));
#43487=CARTESIAN_POINT('Ctrl Pts',(1.51933724328609,1.,3.89289043531893));
#43488=CARTESIAN_POINT('Ctrl Pts',(1.52510482990784,1.,3.8982026070607));
#43489=CARTESIAN_POINT('Ctrl Pts',(1.5297421605556,1.,3.90243719629755));
#43490=CARTESIAN_POINT('Ctrl Pts',(1.53323321827311,1.,3.90560462812846));
#43491=CARTESIAN_POINT('Ctrl Pts',(1.53556639217742,1.,3.90771246854607));
#43492=CARTESIAN_POINT('Ctrl Pts',(1.53673442965255,1.,3.90876544355381));
#43493=CARTESIAN_POINT('Origin',(1.53673442965255,0.,3.90876544355381));
#43494=CARTESIAN_POINT('',(1.67727921511438,1.,3.85054988729471));
#43495=CARTESIAN_POINT('Origin',(0.,0.,0.));
#43496=CARTESIAN_POINT('',(1.071677399622,1.,3.59360648251021));
#43497=CARTESIAN_POINT('Origin',(0.,1.,0.));
#43498=CARTESIAN_POINT('Ctrl Pts',(1.071677399622,1.,3.59360648251021));
#43499=CARTESIAN_POINT('Ctrl Pts',(1.071677399622,0.666666666666667,3.59360648251021));
#43500=CARTESIAN_POINT('Ctrl Pts',(1.071677399622,0.333333333333333,3.59360648251021));
#43501=CARTESIAN_POINT('Ctrl Pts',(1.071677399622,-0.333333333333333,3.59360648251021));
#43502=CARTESIAN_POINT('Ctrl Pts',(1.071677399622,-0.666666666666667,3.59360648251021));
#43503=CARTESIAN_POINT('Ctrl Pts',(1.071677399622,-1.,3.59360648251021));
#43504=CARTESIAN_POINT('Ctrl Pts',(1.05427041296137,-1.,4.06552750530042));
#43505=CARTESIAN_POINT('Ctrl Pts',(1.05427041296137,1.,4.06552750530042));
#43506=CARTESIAN_POINT('Ctrl Pts',(1.05459645194934,-1.,4.06398907542679));
#43507=CARTESIAN_POINT('Ctrl Pts',(1.05459645194934,1.,4.06398907542679));
#43508=CARTESIAN_POINT('Ctrl Pts',(1.05524507177901,-1.,4.06091239150293));
#43509=CARTESIAN_POINT('Ctrl Pts',(1.05524507177901,1.,4.06091239150293));
#43510=CARTESIAN_POINT('Ctrl Pts',(1.0562076270849,-1.,4.05629789308941));
#43511=CARTESIAN_POINT('Ctrl Pts',(1.0562076270849,1.,4.05629789308941));
#43512=CARTESIAN_POINT('Ctrl Pts',(1.05747027728537,-1.,4.05014628387112));
#43513=CARTESIAN_POINT('Ctrl Pts',(1.05747027728537,1.,4.05014628387112));
#43514=CARTESIAN_POINT('Ctrl Pts',(1.05901393667039,-1.,4.04245854429333));
#43515=CARTESIAN_POINT('Ctrl Pts',(1.05901393667039,1.,4.04245854429333));
#43516=CARTESIAN_POINT('Ctrl Pts',(1.06052284712114,-1.,4.03477261142549));
#43517=CARTESIAN_POINT('Ctrl Pts',(1.06052284712114,1.,4.03477261142549));
#43518=CARTESIAN_POINT('Ctrl Pts',(1.06199687787488,-1.,4.02708855235732));
#43519=CARTESIAN_POINT('Ctrl Pts',(1.06199687787488,1.,4.02708855235732));
#43520=CARTESIAN_POINT('Ctrl Pts',(1.06343586496094,-1.,4.0194064749539));
#43521=CARTESIAN_POINT('Ctrl Pts',(1.06343586496094,1.,4.0194064749539));
#43522=CARTESIAN_POINT('Ctrl Pts',(1.06483961342894,-1.,4.0117265418656));
#43523=CARTESIAN_POINT('Ctrl Pts',(1.06483961342894,1.,4.0117265418656));
#43524=CARTESIAN_POINT('Ctrl Pts',(1.06620789963406,-1.,4.00404894951804));
#43525=CARTESIAN_POINT('Ctrl Pts',(1.06620789963406,1.,4.00404894951804));
#43526=CARTESIAN_POINT('Ctrl Pts',(1.06754047381188,-1.,3.99637389919958));
#43527=CARTESIAN_POINT('Ctrl Pts',(1.06754047381188,1.,3.99637389919958));
#43528=CARTESIAN_POINT('Ctrl Pts',(1.06883706263912,-1.,3.98870156857298));
#43529=CARTESIAN_POINT('Ctrl Pts',(1.06883706263912,1.,3.98870156857298));
#43530=CARTESIAN_POINT('Ctrl Pts',(1.07009737257815,-1.,3.98103208801289));
#43531=CARTESIAN_POINT('Ctrl Pts',(1.07009737257815,1.,3.98103208801289));
#43532=CARTESIAN_POINT('Ctrl Pts',(1.07132109206252,-1.,3.97336550222571));
#43533=CARTESIAN_POINT('Ctrl Pts',(1.07132109206252,1.,3.97336550222571));
#43534=CARTESIAN_POINT('Ctrl Pts',(1.07250789943095,-1.,3.96570179322681));
#43535=CARTESIAN_POINT('Ctrl Pts',(1.07250789943095,1.,3.96570179322681));
#43536=CARTESIAN_POINT('Ctrl Pts',(1.07365747426551,-1.,3.95804094429606));
#43537=CARTESIAN_POINT('Ctrl Pts',(1.07365747426551,1.,3.95804094429606));
#43538=CARTESIAN_POINT('Ctrl Pts',(1.07476950921607,-1.,3.95038299600754));
#43539=CARTESIAN_POINT('Ctrl Pts',(1.07476950921607,1.,3.95038299600754));
#43540=CARTESIAN_POINT('Ctrl Pts',(1.07584371946428,-1.,3.94272809633271));
#43541=CARTESIAN_POINT('Ctrl Pts',(1.07584371946428,1.,3.94272809633271));
#43542=CARTESIAN_POINT('Ctrl Pts',(1.07687985975348,-1.,3.93507657572743));
#43543=CARTESIAN_POINT('Ctrl Pts',(1.07687985975348,1.,3.93507657572743));
#43544=CARTESIAN_POINT('Ctrl Pts',(1.07787771707155,-1.,3.92742893349684));
#43545=CARTESIAN_POINT('Ctrl Pts',(1.07787771707155,1.,3.92742893349684));
#43546=CARTESIAN_POINT('Ctrl Pts',(1.07883706663524,-1.,3.91978568924062));
#43547=CARTESIAN_POINT('Ctrl Pts',(1.07883706663524,1.,3.91978568924062));
#43548=CARTESIAN_POINT('Ctrl Pts',(1.0797576350746,-1.,3.91214726022096));
#43549=CARTESIAN_POINT('Ctrl Pts',(1.0797576350746,1.,3.91214726022096));
#43550=CARTESIAN_POINT('Ctrl Pts',(1.08063906483822,-1.,3.90451384092564));
#43551=CARTESIAN_POINT('Ctrl Pts',(1.08063906483822,1.,3.90451384092564));
#43552=CARTESIAN_POINT('Ctrl Pts',(1.08148086931373,-1.,3.89688525098408));
#43553=CARTESIAN_POINT('Ctrl Pts',(1.08148086931373,1.,3.89688525098408));
#43554=CARTESIAN_POINT('Ctrl Pts',(1.08228241999363,-1.,3.88926088975182));
#43555=CARTESIAN_POINT('Ctrl Pts',(1.08228241999363,1.,3.88926088975182));
#43556=CARTESIAN_POINT('Ctrl Pts',(1.08304304871042,-1.,3.88164007721365));
#43557=CARTESIAN_POINT('Ctrl Pts',(1.08304304871042,1.,3.88164007721365));
#43558=CARTESIAN_POINT('Ctrl Pts',(1.0837621330751,-1.,3.87402233722563));
#43559=CARTESIAN_POINT('Ctrl Pts',(1.0837621330751,1.,3.87402233722563));
#43560=CARTESIAN_POINT('Ctrl Pts',(1.08443918607926,-1.,3.86640769434269));
#43561=CARTESIAN_POINT('Ctrl Pts',(1.08443918607926,1.,3.86640769434269));
#43562=CARTESIAN_POINT('Ctrl Pts',(1.08507395120054,-1.,3.85879698702511));
#43563=CARTESIAN_POINT('Ctrl Pts',(1.08507395120054,1.,3.85879698702511));
#43564=CARTESIAN_POINT('Ctrl Pts',(1.08566647671838,-1.,3.85119211322732));
#43565=CARTESIAN_POINT('Ctrl Pts',(1.08566647671838,1.,3.85119211322732));
#43566=CARTESIAN_POINT('Ctrl Pts',(1.08621688337601,-1.,3.84359528764934));
#43567=CARTESIAN_POINT('Ctrl Pts',(1.08621688337601,1.,3.84359528764934));
#43568=CARTESIAN_POINT('Ctrl Pts',(1.08672515456901,-1.,3.83600837071702));
#43569=CARTESIAN_POINT('Ctrl Pts',(1.08672515456901,1.,3.83600837071702));
#43570=CARTESIAN_POINT('Ctrl Pts',(1.08719091307558,-1.,3.82843215316985));
#43571=CARTESIAN_POINT('Ctrl Pts',(1.08719091307558,1.,3.82843215316985));
#43572=CARTESIAN_POINT('Ctrl Pts',(1.08761321539442,-1.,3.82086569676321));
#43573=CARTESIAN_POINT('Ctrl Pts',(1.08761321539442,1.,3.82086569676321));
#43574=CARTESIAN_POINT('Ctrl Pts',(1.08799030610861,-1.,3.81330554446324));
#43575=CARTESIAN_POINT('Ctrl Pts',(1.08799030610861,1.,3.81330554446324));
#43576=CARTESIAN_POINT('Ctrl Pts',(1.08832009255378,-1.,3.80574726657656));
#43577=CARTESIAN_POINT('Ctrl Pts',(1.08832009255378,1.,3.80574726657656));
#43578=CARTESIAN_POINT('Ctrl Pts',(1.08860064435775,-1.,3.79818708705252));
#43579=CARTESIAN_POINT('Ctrl Pts',(1.08860064435775,1.,3.79818708705252));
#43580=CARTESIAN_POINT('Ctrl Pts',(1.08883071512097,-1.,3.79062357974401));
#43581=CARTESIAN_POINT('Ctrl Pts',(1.08883071512097,1.,3.79062357974401));
#43582=CARTESIAN_POINT('Ctrl Pts',(1.08901018614638,-1.,3.78305911299511));
#43583=CARTESIAN_POINT('Ctrl Pts',(1.08901018614638,1.,3.78305911299511));
#43584=CARTESIAN_POINT('Ctrl Pts',(1.08914072791275,-1.,3.7755019940944));
#43585=CARTESIAN_POINT('Ctrl Pts',(1.08914072791275,1.,3.7755019940944));
#43586=CARTESIAN_POINT('Ctrl Pts',(1.08922484204263,-1.,3.76796340094469));
#43587=CARTESIAN_POINT('Ctrl Pts',(1.08922484204263,1.,3.76796340094469));
#43588=CARTESIAN_POINT('Ctrl Pts',(1.08926462734287,-1.,3.76045342580226));
#43589=CARTESIAN_POINT('Ctrl Pts',(1.08926462734287,1.,3.76045342580226));
#43590=CARTESIAN_POINT('Ctrl Pts',(1.08926054632927,-1.,3.75297711748138));
#43591=CARTESIAN_POINT('Ctrl Pts',(1.08926054632927,1.,3.75297711748138));
#43592=CARTESIAN_POINT('Ctrl Pts',(1.08921040494013,-1.,3.74553121371745));
#43593=CARTESIAN_POINT('Ctrl Pts',(1.08921040494013,1.,3.74553121371745));
#43594=CARTESIAN_POINT('Ctrl Pts',(1.08910769013288,-1.,3.73809879348209));
#43595=CARTESIAN_POINT('Ctrl Pts',(1.08910769013288,1.,3.73809879348209));
#43596=CARTESIAN_POINT('Ctrl Pts',(1.08894337390925,-1.,3.73065515162949));
#43597=CARTESIAN_POINT('Ctrl Pts',(1.08894337390925,1.,3.73065515162949));
#43598=CARTESIAN_POINT('Ctrl Pts',(1.08870887220072,-1.,3.72317741369364));
#43599=CARTESIAN_POINT('Ctrl Pts',(1.08870887220072,1.,3.72317741369364));
#43600=CARTESIAN_POINT('Ctrl Pts',(1.08839887334776,-1.,3.71565372339063));
#43601=CARTESIAN_POINT('Ctrl Pts',(1.08839887334776,1.,3.71565372339063));
#43602=CARTESIAN_POINT('Ctrl Pts',(1.0880136731219,-1.,3.70809084139476));
#43603=CARTESIAN_POINT('Ctrl Pts',(1.0880136731219,1.,3.70809084139476));
#43604=CARTESIAN_POINT('Ctrl Pts',(1.08756311291324,-1.,3.70052690909884));
#43605=CARTESIAN_POINT('Ctrl Pts',(1.08756311291324,1.,3.70052690909884));
#43606=CARTESIAN_POINT('Ctrl Pts',(1.08706319540291,-1.,3.69302062410229));
#43607=CARTESIAN_POINT('Ctrl Pts',(1.08706319540291,1.,3.69302062410229));
#43608=CARTESIAN_POINT('Ctrl Pts',(1.08652888882609,-1.,3.68562817420864));
#43609=CARTESIAN_POINT('Ctrl Pts',(1.08652888882609,1.,3.68562817420864));
#43610=CARTESIAN_POINT('Ctrl Pts',(1.08596755755768,-1.,3.67838211685148));
#43611=CARTESIAN_POINT('Ctrl Pts',(1.08596755755768,1.,3.67838211685148));
#43612=CARTESIAN_POINT('Ctrl Pts',(1.0853733414448,-1.,3.67127347729632));
#43613=CARTESIAN_POINT('Ctrl Pts',(1.0853733414448,1.,3.67127347729632));
#43614=CARTESIAN_POINT('Ctrl Pts',(1.0847180992287,-1.,3.66422237895256));
#43615=CARTESIAN_POINT('Ctrl Pts',(1.0847180992287,1.,3.66422237895256));
#43616=CARTESIAN_POINT('Ctrl Pts',(1.08395671077761,-1.,3.65709649161004));
#43617=CARTESIAN_POINT('Ctrl Pts',(1.08395671077761,1.,3.65709649161004));
#43618=CARTESIAN_POINT('Ctrl Pts',(1.08304289898577,-1.,3.64976441208197));
#43619=CARTESIAN_POINT('Ctrl Pts',(1.08304289898577,1.,3.64976441208197));
#43620=CARTESIAN_POINT('Ctrl Pts',(1.08194278850972,-1.,3.64214167843595));
#43621=CARTESIAN_POINT('Ctrl Pts',(1.08194278850972,1.,3.64214167843595));
#43622=CARTESIAN_POINT('Ctrl Pts',(1.08064765719887,-1.,3.63423373196602));
#43623=CARTESIAN_POINT('Ctrl Pts',(1.08064765719887,1.,3.63423373196602));
#43624=CARTESIAN_POINT('Ctrl Pts',(1.07919137290815,-1.,3.62619537902616));
#43625=CARTESIAN_POINT('Ctrl Pts',(1.07919137290815,1.,3.62619537902616));
#43626=CARTESIAN_POINT('Ctrl Pts',(1.07764868137729,-1.,3.61832318504957));
#43627=CARTESIAN_POINT('Ctrl Pts',(1.07764868137729,1.,3.61832318504957));
#43628=CARTESIAN_POINT('Ctrl Pts',(1.07611545402841,-1.,3.61098481349577));
#43629=CARTESIAN_POINT('Ctrl Pts',(1.07611545402841,1.,3.61098481349577));
#43630=CARTESIAN_POINT('Ctrl Pts',(1.0746932716863,-1.,3.6045633988796));
#43631=CARTESIAN_POINT('Ctrl Pts',(1.0746932716863,1.,3.6045633988796));
#43632=CARTESIAN_POINT('Ctrl Pts',(1.0734737254567,-1.,3.59940121154383));
#43633=CARTESIAN_POINT('Ctrl Pts',(1.0734737254567,1.,3.59940121154383));
#43634=CARTESIAN_POINT('Ctrl Pts',(1.07251922679108,-1.,3.59573039611837));
#43635=CARTESIAN_POINT('Ctrl Pts',(1.07251922679108,1.,3.59573039611837));
#43636=CARTESIAN_POINT('Ctrl Pts',(1.07199116987503,-1.,3.59407399103556));
#43637=CARTESIAN_POINT('Ctrl Pts',(1.07199116987503,1.,3.59407399103556));
#43638=CARTESIAN_POINT('Ctrl Pts',(1.07173216219041,-1.,3.59356848057451));
#43639=CARTESIAN_POINT('Ctrl Pts',(1.07173216219041,1.,3.59356848057451));
#43640=CARTESIAN_POINT('Ctrl Pts',(1.07162034256419,-1.,3.59355870577763));
#43641=CARTESIAN_POINT('Ctrl Pts',(1.07162034256419,1.,3.59355870577763));
#43642=CARTESIAN_POINT('Ctrl Pts',(1.07157964745328,-1.,3.59363563249864));
#43643=CARTESIAN_POINT('Ctrl Pts',(1.07157964745328,1.,3.59363563249864));
#43644=CARTESIAN_POINT('',(1.05427041296137,1.,4.06552750530042));
#43645=CARTESIAN_POINT('Ctrl Pts',(1.05427041296137,1.,4.06552750530042));
#43646=CARTESIAN_POINT('Ctrl Pts',(1.05459645194934,1.,4.06398907542679));
#43647=CARTESIAN_POINT('Ctrl Pts',(1.05524507177901,1.,4.06091239150293));
#43648=CARTESIAN_POINT('Ctrl Pts',(1.0562076270849,1.,4.05629789308941));
#43649=CARTESIAN_POINT('Ctrl Pts',(1.05747027728537,1.,4.05014628387112));
#43650=CARTESIAN_POINT('Ctrl Pts',(1.05901393667039,1.,4.04245854429333));
#43651=CARTESIAN_POINT('Ctrl Pts',(1.06052284712114,1.,4.03477261142549));
#43652=CARTESIAN_POINT('Ctrl Pts',(1.06199687787488,1.,4.02708855235732));
#43653=CARTESIAN_POINT('Ctrl Pts',(1.06343586496094,1.,4.0194064749539));
#43654=CARTESIAN_POINT('Ctrl Pts',(1.06483961342894,1.,4.0117265418656));
#43655=CARTESIAN_POINT('Ctrl Pts',(1.06620789963406,1.,4.00404894951804));
#43656=CARTESIAN_POINT('Ctrl Pts',(1.06754047381188,1.,3.99637389919958));
#43657=CARTESIAN_POINT('Ctrl Pts',(1.06883706263912,1.,3.98870156857298));
#43658=CARTESIAN_POINT('Ctrl Pts',(1.07009737257815,1.,3.98103208801289));
#43659=CARTESIAN_POINT('Ctrl Pts',(1.07132109206252,1.,3.97336550222571));
#43660=CARTESIAN_POINT('Ctrl Pts',(1.07250789943095,1.,3.96570179322681));
#43661=CARTESIAN_POINT('Ctrl Pts',(1.07365747426551,1.,3.95804094429606));
#43662=CARTESIAN_POINT('Ctrl Pts',(1.07476950921607,1.,3.95038299600754));
#43663=CARTESIAN_POINT('Ctrl Pts',(1.07584371946428,1.,3.94272809633271));
#43664=CARTESIAN_POINT('Ctrl Pts',(1.07687985975348,1.,3.93507657572743));
#43665=CARTESIAN_POINT('Ctrl Pts',(1.07787771707155,1.,3.92742893349684));
#43666=CARTESIAN_POINT('Ctrl Pts',(1.07883706663524,1.,3.91978568924062));
#43667=CARTESIAN_POINT('Ctrl Pts',(1.0797576350746,1.,3.91214726022096));
#43668=CARTESIAN_POINT('Ctrl Pts',(1.08063906483822,1.,3.90451384092564));
#43669=CARTESIAN_POINT('Ctrl Pts',(1.08148086931373,1.,3.89688525098408));
#43670=CARTESIAN_POINT('Ctrl Pts',(1.08228241999363,1.,3.88926088975182));
#43671=CARTESIAN_POINT('Ctrl Pts',(1.08304304871042,1.,3.88164007721365));
#43672=CARTESIAN_POINT('Ctrl Pts',(1.0837621330751,1.,3.87402233722563));
#43673=CARTESIAN_POINT('Ctrl Pts',(1.08443918607926,1.,3.86640769434269));
#43674=CARTESIAN_POINT('Ctrl Pts',(1.08507395120054,1.,3.85879698702511));
#43675=CARTESIAN_POINT('Ctrl Pts',(1.08566647671838,1.,3.85119211322732));
#43676=CARTESIAN_POINT('Ctrl Pts',(1.08621688337601,1.,3.84359528764934));
#43677=CARTESIAN_POINT('Ctrl Pts',(1.08672515456901,1.,3.83600837071702));
#43678=CARTESIAN_POINT('Ctrl Pts',(1.08719091307558,1.,3.82843215316985));
#43679=CARTESIAN_POINT('Ctrl Pts',(1.08761321539442,1.,3.82086569676321));
#43680=CARTESIAN_POINT('Ctrl Pts',(1.08799030610861,1.,3.81330554446324));
#43681=CARTESIAN_POINT('Ctrl Pts',(1.08832009255378,1.,3.80574726657656));
#43682=CARTESIAN_POINT('Ctrl Pts',(1.08860064435775,1.,3.79818708705252));
#43683=CARTESIAN_POINT('Ctrl Pts',(1.08883071512097,1.,3.79062357974401));
#43684=CARTESIAN_POINT('Ctrl Pts',(1.08901018614638,1.,3.78305911299511));
#43685=CARTESIAN_POINT('Ctrl Pts',(1.08914072791275,1.,3.7755019940944));
#43686=CARTESIAN_POINT('Ctrl Pts',(1.08922484204263,1.,3.76796340094469));
#43687=CARTESIAN_POINT('Ctrl Pts',(1.08926462734287,1.,3.76045342580226));
#43688=CARTESIAN_POINT('Ctrl Pts',(1.08926054632927,1.,3.75297711748138));
#43689=CARTESIAN_POINT('Ctrl Pts',(1.08921040494013,1.,3.74553121371745));
#43690=CARTESIAN_POINT('Ctrl Pts',(1.08910769013288,1.,3.73809879348209));
#43691=CARTESIAN_POINT('Ctrl Pts',(1.08894337390925,1.,3.73065515162949));
#43692=CARTESIAN_POINT('Ctrl Pts',(1.08870887220072,1.,3.72317741369364));
#43693=CARTESIAN_POINT('Ctrl Pts',(1.08839887334776,1.,3.71565372339063));
#43694=CARTESIAN_POINT('Ctrl Pts',(1.0880136731219,1.,3.70809084139476));
#43695=CARTESIAN_POINT('Ctrl Pts',(1.08756311291324,1.,3.70052690909884));
#43696=CARTESIAN_POINT('Ctrl Pts',(1.08706319540291,1.,3.69302062410229));
#43697=CARTESIAN_POINT('Ctrl Pts',(1.08652888882609,1.,3.68562817420864));
#43698=CARTESIAN_POINT('Ctrl Pts',(1.08596755755768,1.,3.67838211685148));
#43699=CARTESIAN_POINT('Ctrl Pts',(1.0853733414448,1.,3.67127347729632));
#43700=CARTESIAN_POINT('Ctrl Pts',(1.0847180992287,1.,3.66422237895256));
#43701=CARTESIAN_POINT('Ctrl Pts',(1.08395671077761,1.,3.65709649161004));
#43702=CARTESIAN_POINT('Ctrl Pts',(1.08304289898577,1.,3.64976441208197));
#43703=CARTESIAN_POINT('Ctrl Pts',(1.08194278850972,1.,3.64214167843595));
#43704=CARTESIAN_POINT('Ctrl Pts',(1.08064765719887,1.,3.63423373196602));
#43705=CARTESIAN_POINT('Ctrl Pts',(1.07919137290815,1.,3.62619537902616));
#43706=CARTESIAN_POINT('Ctrl Pts',(1.07764868137729,1.,3.61832318504957));
#43707=CARTESIAN_POINT('Ctrl Pts',(1.07611545402841,1.,3.61098481349577));
#43708=CARTESIAN_POINT('Ctrl Pts',(1.0746932716863,1.,3.6045633988796));
#43709=CARTESIAN_POINT('Ctrl Pts',(1.0734737254567,1.,3.59940121154383));
#43710=CARTESIAN_POINT('Ctrl Pts',(1.07259084660947,1.,3.59600583195037));
#43711=CARTESIAN_POINT('Ctrl Pts',(1.07209229745284,1.,3.59439597));
#43712=CARTESIAN_POINT('Ctrl Pts',(1.07183575450716,1.,3.59379266874663));
#43713=CARTESIAN_POINT('Ctrl Pts',(1.07171709254271,1.,3.59363512797985));
#43714=CARTESIAN_POINT('Ctrl Pts',(1.071677399622,1.,3.59360648251021));
#43715=CARTESIAN_POINT('',(1.05427041296137,0.,4.06552750530042));
#43716=CARTESIAN_POINT('Ctrl Pts',(0.67669197961156,-1.,3.68843977377012));
#43717=CARTESIAN_POINT('Ctrl Pts',(0.67669197961156,1.,3.68843977377012));
#43718=CARTESIAN_POINT('Ctrl Pts',(0.676620796001989,-1.,3.68838970675497));
#43719=CARTESIAN_POINT('Ctrl Pts',(0.676620796001989,1.,3.68838970675497));
#43720=CARTESIAN_POINT('Ctrl Pts',(0.676525601650855,-1.,3.68844918121303));
#43721=CARTESIAN_POINT('Ctrl Pts',(0.676525601650855,1.,3.68844918121303));
#43722=CARTESIAN_POINT('Ctrl Pts',(0.676524321061226,-1.,3.68901718136181));
#43723=CARTESIAN_POINT('Ctrl Pts',(0.676524321061226,1.,3.68901718136181));
#43724=CARTESIAN_POINT('Ctrl Pts',(0.67680581107509,-1.,3.69073278191994));
#43725=CARTESIAN_POINT('Ctrl Pts',(0.67680581107509,1.,3.69073278191994));
#43726=CARTESIAN_POINT('Ctrl Pts',(0.677621861865497,-1.,3.69443683573598));
#43727=CARTESIAN_POINT('Ctrl Pts',(0.677621861865497,1.,3.69443683573598));
#43728=CARTESIAN_POINT('Ctrl Pts',(0.678878822226026,-1.,3.69959004073005));
#43729=CARTESIAN_POINT('Ctrl Pts',(0.678878822226026,1.,3.69959004073005));
#43730=CARTESIAN_POINT('Ctrl Pts',(0.680526909710876,-1.,3.70595722031785));
#43731=CARTESIAN_POINT('Ctrl Pts',(0.680526909710876,1.,3.70595722031785));
#43732=CARTESIAN_POINT('Ctrl Pts',(0.682492345108929,-1.,3.71319182789943));
#43733=CARTESIAN_POINT('Ctrl Pts',(0.682492345108929,1.,3.71319182789943));
#43734=CARTESIAN_POINT('Ctrl Pts',(0.684691698167848,-1.,3.7209063713926));
#43735=CARTESIAN_POINT('Ctrl Pts',(0.684691698167848,1.,3.7209063713926));
#43736=CARTESIAN_POINT('Ctrl Pts',(0.687043475232354,-1.,3.72872973554051));
#43737=CARTESIAN_POINT('Ctrl Pts',(0.687043475232354,1.,3.72872973554051));
#43738=CARTESIAN_POINT('Ctrl Pts',(0.689479637354813,-1.,3.73636374475077));
#43739=CARTESIAN_POINT('Ctrl Pts',(0.689479637354813,1.,3.73636374475077));
#43740=CARTESIAN_POINT('Ctrl Pts',(0.69196008040082,-1.,3.74365508986712));
#43741=CARTESIAN_POINT('Ctrl Pts',(0.69196008040082,1.,3.74365508986712));
#43742=CARTESIAN_POINT('Ctrl Pts',(0.694474562581492,-1.,3.75060288243455));
#43743=CARTESIAN_POINT('Ctrl Pts',(0.694474562581492,1.,3.75060288243455));
#43744=CARTESIAN_POINT('Ctrl Pts',(0.697031245659743,-1.,3.75729775767023));
#43745=CARTESIAN_POINT('Ctrl Pts',(0.697031245659743,1.,3.75729775767023));
#43746=CARTESIAN_POINT('Ctrl Pts',(0.699648552230917,-1.,3.76387780603759));
#43747=CARTESIAN_POINT('Ctrl Pts',(0.699648552230917,1.,3.76387780603759));
#43748=CARTESIAN_POINT('Ctrl Pts',(0.702346356621551,-1.,3.77048141872872));
#43749=CARTESIAN_POINT('Ctrl Pts',(0.702346356621551,1.,3.77048141872872));
#43750=CARTESIAN_POINT('Ctrl Pts',(0.705135847999816,-1.,3.77719254217129));
#43751=CARTESIAN_POINT('Ctrl Pts',(0.705135847999816,1.,3.77719254217129));
#43752=CARTESIAN_POINT('Ctrl Pts',(0.708015879375459,-1.,3.78402183336605));
#43753=CARTESIAN_POINT('Ctrl Pts',(0.708015879375459,1.,3.78402183336605));
#43754=CARTESIAN_POINT('Ctrl Pts',(0.710978231689016,-1.,3.79093694007094));
#43755=CARTESIAN_POINT('Ctrl Pts',(0.710978231689016,1.,3.79093694007094));
#43756=CARTESIAN_POINT('Ctrl Pts',(0.71401073300664,-1.,3.79788100314975));
#43757=CARTESIAN_POINT('Ctrl Pts',(0.71401073300664,1.,3.79788100314975));
#43758=CARTESIAN_POINT('Ctrl Pts',(0.717100993669114,-1.,3.80479445759309));
#43759=CARTESIAN_POINT('Ctrl Pts',(0.717100993669114,1.,3.80479445759309));
#43760=CARTESIAN_POINT('Ctrl Pts',(0.720240466589236,-1.,3.81163885127344));
#43761=CARTESIAN_POINT('Ctrl Pts',(0.720240466589236,1.,3.81163885127344));
#43762=CARTESIAN_POINT('Ctrl Pts',(0.723426346019422,-1.,3.81840802610835));
#43763=CARTESIAN_POINT('Ctrl Pts',(0.723426346019422,1.,3.81840802610835));
#43764=CARTESIAN_POINT('Ctrl Pts',(0.726659281876663,-1.,3.82511495756713));
#43765=CARTESIAN_POINT('Ctrl Pts',(0.726659281876663,1.,3.82511495756713));
#43766=CARTESIAN_POINT('Ctrl Pts',(0.729942010490167,-1.,3.83178392403383));
#43767=CARTESIAN_POINT('Ctrl Pts',(0.729942010490167,1.,3.83178392403383));
#43768=CARTESIAN_POINT('Ctrl Pts',(0.733277703756078,-1.,3.83844103658009));
#43769=CARTESIAN_POINT('Ctrl Pts',(0.733277703756078,1.,3.83844103658009));
#43770=CARTESIAN_POINT('Ctrl Pts',(0.736668240497117,-1.,3.84510432881213));
#43771=CARTESIAN_POINT('Ctrl Pts',(0.736668240497117,1.,3.84510432881213));
#43772=CARTESIAN_POINT('Ctrl Pts',(0.740113146827137,-1.,3.85177770351216));
#43773=CARTESIAN_POINT('Ctrl Pts',(0.740113146827137,1.,3.85177770351216));
#43774=CARTESIAN_POINT('Ctrl Pts',(0.743610542737012,-1.,3.85845645217594));
#43775=CARTESIAN_POINT('Ctrl Pts',(0.743610542737012,1.,3.85845645217594));
#43776=CARTESIAN_POINT('Ctrl Pts',(0.747157716488871,-1.,3.86513062969889));
#43777=CARTESIAN_POINT('Ctrl Pts',(0.747157716488871,1.,3.86513062969889));
#43778=CARTESIAN_POINT('Ctrl Pts',(0.750751822383027,-1.,3.87178914078374));
#43779=CARTESIAN_POINT('Ctrl Pts',(0.750751822383027,1.,3.87178914078374));
#43780=CARTESIAN_POINT('Ctrl Pts',(0.754390577396856,-1.,3.87842382520065));
#43781=CARTESIAN_POINT('Ctrl Pts',(0.754390577396856,1.,3.87842382520065));
#43782=CARTESIAN_POINT('Ctrl Pts',(0.758072800564801,-1.,3.88503262662689));
#43783=CARTESIAN_POINT('Ctrl Pts',(0.758072800564801,1.,3.88503262662689));
#43784=CARTESIAN_POINT('Ctrl Pts',(0.761798028793969,-1.,3.89161738162245));
#43785=CARTESIAN_POINT('Ctrl Pts',(0.761798028793969,1.,3.89161738162245));
#43786=CARTESIAN_POINT('Ctrl Pts',(0.765566256401295,-1.,3.89818233104378));
#43787=CARTESIAN_POINT('Ctrl Pts',(0.765566256401295,1.,3.89818233104378));
#43788=CARTESIAN_POINT('Ctrl Pts',(0.769377629847873,-1.,3.90473237182633));
#43789=CARTESIAN_POINT('Ctrl Pts',(0.769377629847873,1.,3.90473237182633));
#43790=CARTESIAN_POINT('Ctrl Pts',(0.77323215450632,-1.,3.91127138115243));
#43791=CARTESIAN_POINT('Ctrl Pts',(0.77323215450632,1.,3.91127138115243));
#43792=CARTESIAN_POINT('Ctrl Pts',(0.777129415664956,-1.,3.9178006233448));
#43793=CARTESIAN_POINT('Ctrl Pts',(0.777129415664956,1.,3.9178006233448));
#43794=CARTESIAN_POINT('Ctrl Pts',(0.781068718228451,-1.,3.92431956510441));
#43795=CARTESIAN_POINT('Ctrl Pts',(0.781068718228451,1.,3.92431956510441));
#43796=CARTESIAN_POINT('Ctrl Pts',(0.785049202786507,-1.,3.93082655631789));
#43797=CARTESIAN_POINT('Ctrl Pts',(0.785049202786507,1.,3.93082655631789));
#43798=CARTESIAN_POINT('Ctrl Pts',(0.789069971469332,-1.,3.93731956885676));
#43799=CARTESIAN_POINT('Ctrl Pts',(0.789069971469332,1.,3.93731956885676));
#43800=CARTESIAN_POINT('Ctrl Pts',(0.79313020564096,-1.,3.94379688971283));
#43801=CARTESIAN_POINT('Ctrl Pts',(0.79313020564096,1.,3.94379688971283));
#43802=CARTESIAN_POINT('Ctrl Pts',(0.797229296085315,-1.,3.95025788827136));
#43803=CARTESIAN_POINT('Ctrl Pts',(0.797229296085315,1.,3.95025788827136));
#43804=CARTESIAN_POINT('Ctrl Pts',(0.801366797727049,-1.,3.95670276375108));
#43805=CARTESIAN_POINT('Ctrl Pts',(0.801366797727049,1.,3.95670276375108));
#43806=CARTESIAN_POINT('Ctrl Pts',(0.805542372178361,-1.,3.96313222295815));
#43807=CARTESIAN_POINT('Ctrl Pts',(0.805542372178361,1.,3.96313222295815));
#43808=CARTESIAN_POINT('Ctrl Pts',(0.80975573281809,-1.,3.96954717513232));
#43809=CARTESIAN_POINT('Ctrl Pts',(0.80975573281809,1.,3.96954717513232));
#43810=CARTESIAN_POINT('Ctrl Pts',(0.814006592328843,-1.,3.97594844078811));
#43811=CARTESIAN_POINT('Ctrl Pts',(0.814006592328843,1.,3.97594844078811));
#43812=CARTESIAN_POINT('Ctrl Pts',(0.818294599022293,-1.,3.98233640155404));
#43813=CARTESIAN_POINT('Ctrl Pts',(0.818294599022293,1.,3.98233640155404));
#43814=CARTESIAN_POINT('Ctrl Pts',(0.822619346022118,-1.,3.98871104646485));
#43815=CARTESIAN_POINT('Ctrl Pts',(0.822619346022118,1.,3.98871104646485));
#43816=CARTESIAN_POINT('Ctrl Pts',(0.826980400320789,-1.,3.99507212784431));
#43817=CARTESIAN_POINT('Ctrl Pts',(0.826980400320789,1.,3.99507212784431));
#43818=CARTESIAN_POINT('Ctrl Pts',(0.831377325741622,-1.,4.00141928477507));
#43819=CARTESIAN_POINT('Ctrl Pts',(0.831377325741622,1.,4.00141928477507));
#43820=CARTESIAN_POINT('Ctrl Pts',(0.835809705809645,-1.,4.00775216907856));
#43821=CARTESIAN_POINT('Ctrl Pts',(0.835809705809645,1.,4.00775216907856));
#43822=CARTESIAN_POINT('Ctrl Pts',(0.840277171975854,-1.,4.01407059766103));
#43823=CARTESIAN_POINT('Ctrl Pts',(0.840277171975854,1.,4.01407059766103));
#43824=CARTESIAN_POINT('Ctrl Pts',(0.844779403287745,-1.,4.02037456798441));
#43825=CARTESIAN_POINT('Ctrl Pts',(0.844779403287745,1.,4.02037456798441));
#43826=CARTESIAN_POINT('Ctrl Pts',(0.849316107474244,-1.,4.02666418343164));
#43827=CARTESIAN_POINT('Ctrl Pts',(0.849316107474244,1.,4.02666418343164));
#43828=CARTESIAN_POINT('Ctrl Pts',(0.853887006631755,-1.,4.03293960436756));
#43829=CARTESIAN_POINT('Ctrl Pts',(0.853887006631755,1.,4.03293960436756));
#43830=CARTESIAN_POINT('Ctrl Pts',(0.858491822322827,-1.,4.03920099284773));
#43831=CARTESIAN_POINT('Ctrl Pts',(0.858491822322827,1.,4.03920099284773));
#43832=CARTESIAN_POINT('Ctrl Pts',(0.863130256643258,-1.,4.04544845048584));
#43833=CARTESIAN_POINT('Ctrl Pts',(0.863130256643258,1.,4.04544845048584));
#43834=CARTESIAN_POINT('Ctrl Pts',(0.867801988859917,-1.,4.05168199437909));
#43835=CARTESIAN_POINT('Ctrl Pts',(0.867801988859917,1.,4.05168199437909));
#43836=CARTESIAN_POINT('Ctrl Pts',(0.872506694782446,-1.,4.0579015903134));
#43837=CARTESIAN_POINT('Ctrl Pts',(0.872506694782446,1.,4.0579015903134));
#43838=CARTESIAN_POINT('Ctrl Pts',(0.877244060485837,-1.,4.06410717232905));
#43839=CARTESIAN_POINT('Ctrl Pts',(0.877244060485837,1.,4.06410717232905));
#43840=CARTESIAN_POINT('Ctrl Pts',(0.882013797525691,-1.,4.07029866694192));
#43841=CARTESIAN_POINT('Ctrl Pts',(0.882013797525691,1.,4.07029866694192));
#43842=CARTESIAN_POINT('Ctrl Pts',(0.886815658358501,-1.,4.07647601773635));
#43843=CARTESIAN_POINT('Ctrl Pts',(0.886815658358501,1.,4.07647601773635));
#43844=CARTESIAN_POINT('Ctrl Pts',(0.891649447916277,-1.,4.08263920304799));
#43845=CARTESIAN_POINT('Ctrl Pts',(0.891649447916277,1.,4.08263920304799));
#43846=CARTESIAN_POINT('Ctrl Pts',(0.896515019231333,-1.,4.08878822246833));
#43847=CARTESIAN_POINT('Ctrl Pts',(0.896515019231333,1.,4.08878822246833));
#43848=CARTESIAN_POINT('Ctrl Pts',(0.900432820941674,-1.,4.09369611522387));
#43849=CARTESIAN_POINT('Ctrl Pts',(0.900432820941674,1.,4.09369611522387));
#43850=CARTESIAN_POINT('Ctrl Pts',(0.903385402441587,-1.,4.09737067245935));
#43851=CARTESIAN_POINT('Ctrl Pts',(0.903385402441587,1.,4.09737067245935));
#43852=CARTESIAN_POINT('Ctrl Pts',(0.905360112215337,-1.,4.09981755067523));
#43853=CARTESIAN_POINT('Ctrl Pts',(0.905360112215337,1.,4.09981755067523));
#43854=CARTESIAN_POINT('Ctrl Pts',(0.906349047628865,-1.,4.10104028313088));
#43855=CARTESIAN_POINT('Ctrl Pts',(0.906349047628865,1.,4.10104028313088));
#43856=CARTESIAN_POINT('',(0.676591647975428,1.,3.68845817949586));
#43857=CARTESIAN_POINT('Ctrl Pts',(0.676591647975428,-1.,3.68845817949586));
#43858=CARTESIAN_POINT('Ctrl Pts',(0.676591647975428,-0.666666666666667,
3.68845817949586));
#43859=CARTESIAN_POINT('Ctrl Pts',(0.676591647975428,-0.333333333333333,
3.68845817949586));
#43860=CARTESIAN_POINT('Ctrl Pts',(0.676591647975428,0.333333333333333,
3.68845817949586));
#43861=CARTESIAN_POINT('Ctrl Pts',(0.676591647975428,0.666666666666667,
3.68845817949586));
#43862=CARTESIAN_POINT('Ctrl Pts',(0.676591647975428,1.,3.68845817949586));
#43863=CARTESIAN_POINT('',(0.906349047628865,1.,4.10104028313088));
#43864=CARTESIAN_POINT('',(0.906349047628865,0.,4.10104028313088));
#43865=CARTESIAN_POINT('Ctrl Pts',(0.676591647975428,1.,3.68845817949586));
#43866=CARTESIAN_POINT('Ctrl Pts',(0.676569286094606,1.,3.68850172300477));
#43867=CARTESIAN_POINT('Ctrl Pts',(0.676535079520806,1.,3.68869596425969));
#43868=CARTESIAN_POINT('Ctrl Pts',(0.676580391119396,1.,3.68934997767243));
#43869=CARTESIAN_POINT('Ctrl Pts',(0.676867042599401,1.,3.69101071175464));
#43870=CARTESIAN_POINT('Ctrl Pts',(0.677621861865497,1.,3.69443683573598));
#43871=CARTESIAN_POINT('Ctrl Pts',(0.678878822226026,1.,3.69959004073005));
#43872=CARTESIAN_POINT('Ctrl Pts',(0.680526909710876,1.,3.70595722031785));
#43873=CARTESIAN_POINT('Ctrl Pts',(0.682492345108929,1.,3.71319182789943));
#43874=CARTESIAN_POINT('Ctrl Pts',(0.684691698167848,1.,3.7209063713926));
#43875=CARTESIAN_POINT('Ctrl Pts',(0.687043475232354,1.,3.72872973554051));
#43876=CARTESIAN_POINT('Ctrl Pts',(0.689479637354813,1.,3.73636374475077));
#43877=CARTESIAN_POINT('Ctrl Pts',(0.69196008040082,1.,3.74365508986712));
#43878=CARTESIAN_POINT('Ctrl Pts',(0.694474562581492,1.,3.75060288243455));
#43879=CARTESIAN_POINT('Ctrl Pts',(0.697031245659743,1.,3.75729775767023));
#43880=CARTESIAN_POINT('Ctrl Pts',(0.699648552230917,1.,3.76387780603759));
#43881=CARTESIAN_POINT('Ctrl Pts',(0.702346356621551,1.,3.77048141872872));
#43882=CARTESIAN_POINT('Ctrl Pts',(0.705135847999816,1.,3.77719254217129));
#43883=CARTESIAN_POINT('Ctrl Pts',(0.708015879375459,1.,3.78402183336605));
#43884=CARTESIAN_POINT('Ctrl Pts',(0.710978231689016,1.,3.79093694007094));
#43885=CARTESIAN_POINT('Ctrl Pts',(0.71401073300664,1.,3.79788100314975));
#43886=CARTESIAN_POINT('Ctrl Pts',(0.717100993669114,1.,3.80479445759309));
#43887=CARTESIAN_POINT('Ctrl Pts',(0.720240466589236,1.,3.81163885127344));
#43888=CARTESIAN_POINT('Ctrl Pts',(0.723426346019422,1.,3.81840802610835));
#43889=CARTESIAN_POINT('Ctrl Pts',(0.726659281876663,1.,3.82511495756713));
#43890=CARTESIAN_POINT('Ctrl Pts',(0.729942010490167,1.,3.83178392403383));
#43891=CARTESIAN_POINT('Ctrl Pts',(0.733277703756078,1.,3.83844103658009));
#43892=CARTESIAN_POINT('Ctrl Pts',(0.736668240497117,1.,3.84510432881213));
#43893=CARTESIAN_POINT('Ctrl Pts',(0.740113146827137,1.,3.85177770351216));
#43894=CARTESIAN_POINT('Ctrl Pts',(0.743610542737012,1.,3.85845645217594));
#43895=CARTESIAN_POINT('Ctrl Pts',(0.747157716488871,1.,3.86513062969889));
#43896=CARTESIAN_POINT('Ctrl Pts',(0.750751822383027,1.,3.87178914078374));
#43897=CARTESIAN_POINT('Ctrl Pts',(0.754390577396856,1.,3.87842382520065));
#43898=CARTESIAN_POINT('Ctrl Pts',(0.758072800564801,1.,3.88503262662689));
#43899=CARTESIAN_POINT('Ctrl Pts',(0.761798028793969,1.,3.89161738162245));
#43900=CARTESIAN_POINT('Ctrl Pts',(0.765566256401295,1.,3.89818233104378));
#43901=CARTESIAN_POINT('Ctrl Pts',(0.769377629847873,1.,3.90473237182633));
#43902=CARTESIAN_POINT('Ctrl Pts',(0.77323215450632,1.,3.91127138115243));
#43903=CARTESIAN_POINT('Ctrl Pts',(0.777129415664956,1.,3.9178006233448));
#43904=CARTESIAN_POINT('Ctrl Pts',(0.781068718228451,1.,3.92431956510441));
#43905=CARTESIAN_POINT('Ctrl Pts',(0.785049202786507,1.,3.93082655631789));
#43906=CARTESIAN_POINT('Ctrl Pts',(0.789069971469332,1.,3.93731956885676));
#43907=CARTESIAN_POINT('Ctrl Pts',(0.79313020564096,1.,3.94379688971283));
#43908=CARTESIAN_POINT('Ctrl Pts',(0.797229296085315,1.,3.95025788827136));
#43909=CARTESIAN_POINT('Ctrl Pts',(0.801366797727049,1.,3.95670276375108));
#43910=CARTESIAN_POINT('Ctrl Pts',(0.805542372178361,1.,3.96313222295815));
#43911=CARTESIAN_POINT('Ctrl Pts',(0.80975573281809,1.,3.96954717513232));
#43912=CARTESIAN_POINT('Ctrl Pts',(0.814006592328843,1.,3.97594844078811));
#43913=CARTESIAN_POINT('Ctrl Pts',(0.818294599022293,1.,3.98233640155404));
#43914=CARTESIAN_POINT('Ctrl Pts',(0.822619346022118,1.,3.98871104646485));
#43915=CARTESIAN_POINT('Ctrl Pts',(0.826980400320789,1.,3.99507212784431));
#43916=CARTESIAN_POINT('Ctrl Pts',(0.831377325741622,1.,4.00141928477507));
#43917=CARTESIAN_POINT('Ctrl Pts',(0.835809705809645,1.,4.00775216907856));
#43918=CARTESIAN_POINT('Ctrl Pts',(0.840277171975854,1.,4.01407059766103));
#43919=CARTESIAN_POINT('Ctrl Pts',(0.844779403287745,1.,4.02037456798441));
#43920=CARTESIAN_POINT('Ctrl Pts',(0.849316107474244,1.,4.02666418343164));
#43921=CARTESIAN_POINT('Ctrl Pts',(0.853887006631755,1.,4.03293960436756));
#43922=CARTESIAN_POINT('Ctrl Pts',(0.858491822322827,1.,4.03920099284773));
#43923=CARTESIAN_POINT('Ctrl Pts',(0.863130256643258,1.,4.04544845048584));
#43924=CARTESIAN_POINT('Ctrl Pts',(0.867801988859917,1.,4.05168199437909));
#43925=CARTESIAN_POINT('Ctrl Pts',(0.872506694782446,1.,4.0579015903134));
#43926=CARTESIAN_POINT('Ctrl Pts',(0.877244060485837,1.,4.06410717232905));
#43927=CARTESIAN_POINT('Ctrl Pts',(0.882013797525691,1.,4.07029866694192));
#43928=CARTESIAN_POINT('Ctrl Pts',(0.886815658358501,1.,4.07647601773635));
#43929=CARTESIAN_POINT('Ctrl Pts',(0.891649447916277,1.,4.08263920304799));
#43930=CARTESIAN_POINT('Ctrl Pts',(0.896515019231333,1.,4.08878822246833));
#43931=CARTESIAN_POINT('Ctrl Pts',(0.900432820941674,1.,4.09369611522387));
#43932=CARTESIAN_POINT('Ctrl Pts',(0.903385402441587,1.,4.09737067245935));
#43933=CARTESIAN_POINT('Ctrl Pts',(0.905360112215337,1.,4.09981755067523));
#43934=CARTESIAN_POINT('Ctrl Pts',(0.906349047628865,1.,4.10104028313088));
#43935=CARTESIAN_POINT('Origin',(0.906349047628865,0.,4.10104028313088));
#43936=CARTESIAN_POINT('',(1.05427041296137,1.,4.06552750530042));
#43937=CARTESIAN_POINT('Origin',(0.,0.,0.));
#43938=CARTESIAN_POINT('',(0.496319364829374,1.,3.71701050416802));
#43939=CARTESIAN_POINT('Origin',(0.,1.,0.));
#43940=CARTESIAN_POINT('Ctrl Pts',(0.496319364829373,1.,3.71701050416802));
#43941=CARTESIAN_POINT('Ctrl Pts',(0.496319364829373,0.666666666666667,
3.71701050416802));
#43942=CARTESIAN_POINT('Ctrl Pts',(0.496319364829373,0.333333333333333,
3.71701050416802));
#43943=CARTESIAN_POINT('Ctrl Pts',(0.496319364829373,-0.333333333333333,
3.71701050416802));
#43944=CARTESIAN_POINT('Ctrl Pts',(0.496319364829373,-0.666666666666667,
3.71701050416802));
#43945=CARTESIAN_POINT('Ctrl Pts',(0.496319364829373,-1.,3.71701050416802));
#43946=CARTESIAN_POINT('Ctrl Pts',(0.405301974318349,-1.,4.18039834341342));
#43947=CARTESIAN_POINT('Ctrl Pts',(0.405301974318349,1.,4.18039834341342));
#43948=CARTESIAN_POINT('Ctrl Pts',(0.40586466267963,-1.,4.17892985789908));
#43949=CARTESIAN_POINT('Ctrl Pts',(0.40586466267963,1.,4.17892985789908));
#43950=CARTESIAN_POINT('Ctrl Pts',(0.406986596326602,-1.,4.17599251955585));
#43951=CARTESIAN_POINT('Ctrl Pts',(0.406986596326602,1.,4.17599251955585));
#43952=CARTESIAN_POINT('Ctrl Pts',(0.408659167570152,-1.,4.17158541009947));
#43953=CARTESIAN_POINT('Ctrl Pts',(0.408659167570152,1.,4.17158541009947));
#43954=CARTESIAN_POINT('Ctrl Pts',(0.410868596148613,-1.,4.16570705940731));
#43955=CARTESIAN_POINT('Ctrl Pts',(0.410868596148613,1.,4.16570705940731));
#43956=CARTESIAN_POINT('Ctrl Pts',(0.413595877953268,-1.,4.1583554501909));
#43957=CARTESIAN_POINT('Ctrl Pts',(0.413595877953268,1.,4.1583554501909));
#43958=CARTESIAN_POINT('Ctrl Pts',(0.416288556008986,-1.,4.15100018950989));
#43959=CARTESIAN_POINT('Ctrl Pts',(0.416288556008986,1.,4.15100018950989));
#43960=CARTESIAN_POINT('Ctrl Pts',(0.418946490667799,-1.,4.14364132317223));
#43961=CARTESIAN_POINT('Ctrl Pts',(0.418946490667799,1.,4.14364132317223));
#43962=CARTESIAN_POINT('Ctrl Pts',(0.421569503103971,-1.,4.13627893206433));
#43963=CARTESIAN_POINT('Ctrl Pts',(0.421569503103971,1.,4.13627893206433));
#43964=CARTESIAN_POINT('Ctrl Pts',(0.424157375323155,-1.,4.1289131463371));
#43965=CARTESIAN_POINT('Ctrl Pts',(0.424157375323155,1.,4.1289131463371));
#43966=CARTESIAN_POINT('Ctrl Pts',(0.426709855706242,-1.,4.1215441250121));
#43967=CARTESIAN_POINT('Ctrl Pts',(0.426709855706242,1.,4.1215441250121));
#43968=CARTESIAN_POINT('Ctrl Pts',(0.429226666075372,-1.,4.1141720278277));
#43969=CARTESIAN_POINT('Ctrl Pts',(0.429226666075372,1.,4.1141720278277));
#43970=CARTESIAN_POINT('Ctrl Pts',(0.431707508679771,-1.,4.10679698750219));
#43971=CARTESIAN_POINT('Ctrl Pts',(0.431707508679771,1.,4.10679698750219));
#43972=CARTESIAN_POINT('Ctrl Pts',(0.434152073200642,-1.,4.09941908688567));
#43973=CARTESIAN_POINT('Ctrl Pts',(0.434152073200642,1.,4.09941908688567));
#43974=CARTESIAN_POINT('Ctrl Pts',(0.436560044913814,-1.,4.09203832139439));
#43975=CARTESIAN_POINT('Ctrl Pts',(0.436560044913814,1.,4.09203832139439));
#43976=CARTESIAN_POINT('Ctrl Pts',(0.438931108931613,-1.,4.08465462294625));
#43977=CARTESIAN_POINT('Ctrl Pts',(0.438931108931613,1.,4.08465462294625));
#43978=CARTESIAN_POINT('Ctrl Pts',(0.441264951396587,-1.,4.07726792490256));
#43979=CARTESIAN_POINT('Ctrl Pts',(0.441264951396587,1.,4.07726792490256));
#43980=CARTESIAN_POINT('Ctrl Pts',(0.443561262395407,-1.,4.0698782192577));
#43981=CARTESIAN_POINT('Ctrl Pts',(0.443561262395407,1.,4.0698782192577));
#43982=CARTESIAN_POINT('Ctrl Pts',(0.445819737468477,-1.,4.06248560760596));
#43983=CARTESIAN_POINT('Ctrl Pts',(0.445819737468477,1.,4.06248560760596));
#43984=CARTESIAN_POINT('Ctrl Pts',(0.448040082683976,-1.,4.05509037796815));
#43985=CARTESIAN_POINT('Ctrl Pts',(0.448040082683976,1.,4.05509037796815));
#43986=CARTESIAN_POINT('Ctrl Pts',(0.450222009543773,-1.,4.0476929901797));
#43987=CARTESIAN_POINT('Ctrl Pts',(0.450222009543773,1.,4.0476929901797));
#43988=CARTESIAN_POINT('Ctrl Pts',(0.452365214748778,-1.,4.0402939222793));
#43989=CARTESIAN_POINT('Ctrl Pts',(0.452365214748778,1.,4.0402939222793));
#43990=CARTESIAN_POINT('Ctrl Pts',(0.454469363020495,-1.,4.03289354362745));
#43991=CARTESIAN_POINT('Ctrl Pts',(0.454469363020495,1.,4.03289354362745));
#43992=CARTESIAN_POINT('Ctrl Pts',(0.456534070784968,-1.,4.02549199038414));
#43993=CARTESIAN_POINT('Ctrl Pts',(0.456534070784968,1.,4.02549199038414));
#43994=CARTESIAN_POINT('Ctrl Pts',(0.458558885637,-1.,4.01808900827647));
#43995=CARTESIAN_POINT('Ctrl Pts',(0.458558885637,1.,4.01808900827647));
#43996=CARTESIAN_POINT('Ctrl Pts',(0.460543280768577,-1.,4.01068390573469));
#43997=CARTESIAN_POINT('Ctrl Pts',(0.460543280768577,1.,4.01068390573469));
#43998=CARTESIAN_POINT('Ctrl Pts',(0.462486702616251,-1.,4.00327590659129));
#43999=CARTESIAN_POINT('Ctrl Pts',(0.462486702616251,1.,4.00327590659129));
#44000=CARTESIAN_POINT('Ctrl Pts',(0.464388610938994,-1.,3.99586444320135));
#44001=CARTESIAN_POINT('Ctrl Pts',(0.464388610938994,1.,3.99586444320135));
#44002=CARTESIAN_POINT('Ctrl Pts',(0.466248520883034,-1.,3.98844946363258));
#44003=CARTESIAN_POINT('Ctrl Pts',(0.466248520883034,1.,3.98844946363258));
#44004=CARTESIAN_POINT('Ctrl Pts',(0.468066047920139,-1.,3.98103175589349));
#44005=CARTESIAN_POINT('Ctrl Pts',(0.468066047920139,1.,3.98103175589349));
#44006=CARTESIAN_POINT('Ctrl Pts',(0.469840942829878,-1.,3.97361320212413));
#44007=CARTESIAN_POINT('Ctrl Pts',(0.469840942829878,1.,3.97361320212413));
#44008=CARTESIAN_POINT('Ctrl Pts',(0.471572978413493,-1.,3.96619600864626));
#44009=CARTESIAN_POINT('Ctrl Pts',(0.471572978413493,1.,3.96619600864626));
#44010=CARTESIAN_POINT('Ctrl Pts',(0.473261847236295,-1.,3.95878201038332));
#44011=CARTESIAN_POINT('Ctrl Pts',(0.473261847236295,1.,3.95878201038332));
#44012=CARTESIAN_POINT('Ctrl Pts',(0.47490705302179,-1.,3.95137192932898));
#44013=CARTESIAN_POINT('Ctrl Pts',(0.47490705302179,1.,3.95137192932898));
#44014=CARTESIAN_POINT('Ctrl Pts',(0.476507810658534,-1.,3.94396469119385));
#44015=CARTESIAN_POINT('Ctrl Pts',(0.476507810658534,1.,3.94396469119385));
#44016=CARTESIAN_POINT('Ctrl Pts',(0.478062927140957,-1.,3.93655660689819));
#44017=CARTESIAN_POINT('Ctrl Pts',(0.478062927140957,1.,3.93655660689819));
#44018=CARTESIAN_POINT('Ctrl Pts',(0.479571028525565,-1.,3.92914297392067));
#44019=CARTESIAN_POINT('Ctrl Pts',(0.479571028525565,1.,3.92914297392067));
#44020=CARTESIAN_POINT('Ctrl Pts',(0.481030798910735,-1.,3.92171976072334));
#44021=CARTESIAN_POINT('Ctrl Pts',(0.481030798910735,1.,3.92171976072334));
#44022=CARTESIAN_POINT('Ctrl Pts',(0.482441230340708,-1.,3.91428536373749));
#44023=CARTESIAN_POINT('Ctrl Pts',(0.482441230340708,1.,3.91428536373749));
#44024=CARTESIAN_POINT('Ctrl Pts',(0.48380183508916,-1.,3.90684210358063));
#44025=CARTESIAN_POINT('Ctrl Pts',(0.48380183508916,1.,3.90684210358063));
#44026=CARTESIAN_POINT('Ctrl Pts',(0.485112963522245,-1.,3.89939844658529));
#44027=CARTESIAN_POINT('Ctrl Pts',(0.485112963522245,1.,3.89939844658529));
#44028=CARTESIAN_POINT('Ctrl Pts',(0.486375337854133,-1.,3.89196582437574));
#44029=CARTESIAN_POINT('Ctrl Pts',(0.486375337854133,1.,3.89196582437574));
#44030=CARTESIAN_POINT('Ctrl Pts',(0.487589452275179,-1.,3.88455453328156));
#44031=CARTESIAN_POINT('Ctrl Pts',(0.487589452275179,1.,3.88455453328156));
#44032=CARTESIAN_POINT('Ctrl Pts',(0.488754973798281,-1.,3.87716963231115));
#44033=CARTESIAN_POINT('Ctrl Pts',(0.488754973798281,1.,3.87716963231115));
#44034=CARTESIAN_POINT('Ctrl Pts',(0.489870245704899,-1.,3.86980755613694));
#44035=CARTESIAN_POINT('Ctrl Pts',(0.489870245704899,1.,3.86980755613694));
#44036=CARTESIAN_POINT('Ctrl Pts',(0.490931482170849,-1.,3.86245057319215));
#44037=CARTESIAN_POINT('Ctrl Pts',(0.490931482170849,1.,3.86245057319215));
#44038=CARTESIAN_POINT('Ctrl Pts',(0.49193363108376,-1.,3.85507287020223));
#44039=CARTESIAN_POINT('Ctrl Pts',(0.49193363108376,1.,3.85507287020223));
#44040=CARTESIAN_POINT('Ctrl Pts',(0.492871792414095,-1.,3.84765051147965));
#44041=CARTESIAN_POINT('Ctrl Pts',(0.492871792414095,1.,3.84765051147965));
#44042=CARTESIAN_POINT('Ctrl Pts',(0.493742574629117,-1.,3.84017095578438));
#44043=CARTESIAN_POINT('Ctrl Pts',(0.493742574629117,1.,3.84017095578438));
#44044=CARTESIAN_POINT('Ctrl Pts',(0.494545212256425,-1.,3.8326409268245));
#44045=CARTESIAN_POINT('Ctrl Pts',(0.494545212256425,1.,3.8326409268245));
#44046=CARTESIAN_POINT('Ctrl Pts',(0.495283458893903,-1.,3.82509963594156));
#44047=CARTESIAN_POINT('Ctrl Pts',(0.495283458893903,1.,3.82509963594156));
#44048=CARTESIAN_POINT('Ctrl Pts',(0.495963937875571,-1.,3.81760756144099));
#44049=CARTESIAN_POINT('Ctrl Pts',(0.495963937875571,1.,3.81760756144099));
#44050=CARTESIAN_POINT('Ctrl Pts',(0.496592643443789,-1.,3.81022254090909));
#44051=CARTESIAN_POINT('Ctrl Pts',(0.496592643443789,1.,3.81022254090909));
#44052=CARTESIAN_POINT('Ctrl Pts',(0.49717175620109,-1.,3.80297788298545));
#44053=CARTESIAN_POINT('Ctrl Pts',(0.49717175620109,1.,3.80297788298545));
#44054=CARTESIAN_POINT('Ctrl Pts',(0.49769689210058,-1.,3.79586380669959));
#44055=CARTESIAN_POINT('Ctrl Pts',(0.49769689210058,1.,3.79586380669959));
#44056=CARTESIAN_POINT('Ctrl Pts',(0.498152751800819,-1.,3.78879701661152));
#44057=CARTESIAN_POINT('Ctrl Pts',(0.498152751800819,1.,3.78879701661152));
#44058=CARTESIAN_POINT('Ctrl Pts',(0.498515471679378,-1.,3.78163975337189));
#44059=CARTESIAN_POINT('Ctrl Pts',(0.498515471679378,1.,3.78163975337189));
#44060=CARTESIAN_POINT('Ctrl Pts',(0.498759900365686,-1.,3.77425499225089));
#44061=CARTESIAN_POINT('Ctrl Pts',(0.498759900365686,1.,3.77425499225089));
#44062=CARTESIAN_POINT('Ctrl Pts',(0.498865792335185,-1.,3.76655401191144));
#44063=CARTESIAN_POINT('Ctrl Pts',(0.498865792335185,1.,3.76655401191144));
#44064=CARTESIAN_POINT('Ctrl Pts',(0.498823681615513,-1.,3.75854082221127));
#44065=CARTESIAN_POINT('Ctrl Pts',(0.498823681615513,1.,3.75854082221127));
#44066=CARTESIAN_POINT('Ctrl Pts',(0.498642802042929,-1.,3.75037362168103));
#44067=CARTESIAN_POINT('Ctrl Pts',(0.498642802042929,1.,3.75037362168103));
#44068=CARTESIAN_POINT('Ctrl Pts',(0.498350586058176,-1.,3.74235701735109));
#44069=CARTESIAN_POINT('Ctrl Pts',(0.498350586058176,1.,3.74235701735109));
#44070=CARTESIAN_POINT('Ctrl Pts',(0.497984209510495,-1.,3.73486914372834));
#44071=CARTESIAN_POINT('Ctrl Pts',(0.497984209510495,1.,3.73486914372834));
#44072=CARTESIAN_POINT('Ctrl Pts',(0.497584067153279,-1.,3.72830430904794));
#44073=CARTESIAN_POINT('Ctrl Pts',(0.497584067153279,1.,3.72830430904794));
#44074=CARTESIAN_POINT('Ctrl Pts',(0.497187079575794,-1.,3.72301489774241));
#44075=CARTESIAN_POINT('Ctrl Pts',(0.497187079575794,1.,3.72301489774241));
#44076=CARTESIAN_POINT('Ctrl Pts',(0.496818574419988,-1.,3.71923995965807));
#44077=CARTESIAN_POINT('Ctrl Pts',(0.496818574419988,1.,3.71923995965807));
#44078=CARTESIAN_POINT('Ctrl Pts',(0.496556137603856,-1.,3.71752134136931));
#44079=CARTESIAN_POINT('Ctrl Pts',(0.496556137603856,1.,3.71752134136931));
#44080=CARTESIAN_POINT('Ctrl Pts',(0.496379397992181,-1.,3.71698153685229));
#44081=CARTESIAN_POINT('Ctrl Pts',(0.496379397992181,1.,3.71698153685229));
#44082=CARTESIAN_POINT('Ctrl Pts',(0.496270484166233,-1.,3.71695438995598));
#44083=CARTESIAN_POINT('Ctrl Pts',(0.496270484166233,1.,3.71695438995598));
#44084=CARTESIAN_POINT('Ctrl Pts',(0.496218256089211,-1.,3.71702400346349));
#44085=CARTESIAN_POINT('Ctrl Pts',(0.496218256089211,1.,3.71702400346349));
#44086=CARTESIAN_POINT('',(0.405301974318349,1.,4.18039834341342));
#44087=CARTESIAN_POINT('Ctrl Pts',(0.405301974318349,1.,4.18039834341342));
#44088=CARTESIAN_POINT('Ctrl Pts',(0.40586466267963,1.,4.17892985789908));
#44089=CARTESIAN_POINT('Ctrl Pts',(0.406986596326602,1.,4.17599251955585));
#44090=CARTESIAN_POINT('Ctrl Pts',(0.408659167570152,1.,4.17158541009947));
#44091=CARTESIAN_POINT('Ctrl Pts',(0.410868596148613,1.,4.16570705940731));
#44092=CARTESIAN_POINT('Ctrl Pts',(0.413595877953268,1.,4.1583554501909));
#44093=CARTESIAN_POINT('Ctrl Pts',(0.416288556008986,1.,4.15100018950989));
#44094=CARTESIAN_POINT('Ctrl Pts',(0.418946490667799,1.,4.14364132317223));
#44095=CARTESIAN_POINT('Ctrl Pts',(0.421569503103971,1.,4.13627893206433));
#44096=CARTESIAN_POINT('Ctrl Pts',(0.424157375323155,1.,4.1289131463371));
#44097=CARTESIAN_POINT('Ctrl Pts',(0.426709855706242,1.,4.1215441250121));
#44098=CARTESIAN_POINT('Ctrl Pts',(0.429226666075372,1.,4.1141720278277));
#44099=CARTESIAN_POINT('Ctrl Pts',(0.431707508679771,1.,4.10679698750219));
#44100=CARTESIAN_POINT('Ctrl Pts',(0.434152073200642,1.,4.09941908688567));
#44101=CARTESIAN_POINT('Ctrl Pts',(0.436560044913814,1.,4.09203832139439));
#44102=CARTESIAN_POINT('Ctrl Pts',(0.438931108931613,1.,4.08465462294625));
#44103=CARTESIAN_POINT('Ctrl Pts',(0.441264951396587,1.,4.07726792490256));
#44104=CARTESIAN_POINT('Ctrl Pts',(0.443561262395407,1.,4.0698782192577));
#44105=CARTESIAN_POINT('Ctrl Pts',(0.445819737468477,1.,4.06248560760596));
#44106=CARTESIAN_POINT('Ctrl Pts',(0.448040082683976,1.,4.05509037796815));
#44107=CARTESIAN_POINT('Ctrl Pts',(0.450222009543773,1.,4.0476929901797));
#44108=CARTESIAN_POINT('Ctrl Pts',(0.452365214748778,1.,4.0402939222793));
#44109=CARTESIAN_POINT('Ctrl Pts',(0.454469363020495,1.,4.03289354362745));
#44110=CARTESIAN_POINT('Ctrl Pts',(0.456534070784968,1.,4.02549199038414));
#44111=CARTESIAN_POINT('Ctrl Pts',(0.458558885637,1.,4.01808900827647));
#44112=CARTESIAN_POINT('Ctrl Pts',(0.460543280768577,1.,4.01068390573469));
#44113=CARTESIAN_POINT('Ctrl Pts',(0.462486702616251,1.,4.00327590659129));
#44114=CARTESIAN_POINT('Ctrl Pts',(0.464388610938994,1.,3.99586444320135));
#44115=CARTESIAN_POINT('Ctrl Pts',(0.466248520883034,1.,3.98844946363258));
#44116=CARTESIAN_POINT('Ctrl Pts',(0.468066047920139,1.,3.98103175589349));
#44117=CARTESIAN_POINT('Ctrl Pts',(0.469840942829878,1.,3.97361320212413));
#44118=CARTESIAN_POINT('Ctrl Pts',(0.471572978413493,1.,3.96619600864626));
#44119=CARTESIAN_POINT('Ctrl Pts',(0.473261847236295,1.,3.95878201038332));
#44120=CARTESIAN_POINT('Ctrl Pts',(0.47490705302179,1.,3.95137192932898));
#44121=CARTESIAN_POINT('Ctrl Pts',(0.476507810658534,1.,3.94396469119385));
#44122=CARTESIAN_POINT('Ctrl Pts',(0.478062927140957,1.,3.93655660689819));
#44123=CARTESIAN_POINT('Ctrl Pts',(0.479571028525565,1.,3.92914297392067));
#44124=CARTESIAN_POINT('Ctrl Pts',(0.481030798910735,1.,3.92171976072334));
#44125=CARTESIAN_POINT('Ctrl Pts',(0.482441230340708,1.,3.91428536373749));
#44126=CARTESIAN_POINT('Ctrl Pts',(0.48380183508916,1.,3.90684210358063));
#44127=CARTESIAN_POINT('Ctrl Pts',(0.485112963522245,1.,3.89939844658529));
#44128=CARTESIAN_POINT('Ctrl Pts',(0.486375337854133,1.,3.89196582437574));
#44129=CARTESIAN_POINT('Ctrl Pts',(0.487589452275179,1.,3.88455453328156));
#44130=CARTESIAN_POINT('Ctrl Pts',(0.488754973798281,1.,3.87716963231115));
#44131=CARTESIAN_POINT('Ctrl Pts',(0.489870245704899,1.,3.86980755613694));
#44132=CARTESIAN_POINT('Ctrl Pts',(0.490931482170849,1.,3.86245057319215));
#44133=CARTESIAN_POINT('Ctrl Pts',(0.49193363108376,1.,3.85507287020223));
#44134=CARTESIAN_POINT('Ctrl Pts',(0.492871792414095,1.,3.84765051147965));
#44135=CARTESIAN_POINT('Ctrl Pts',(0.493742574629117,1.,3.84017095578438));
#44136=CARTESIAN_POINT('Ctrl Pts',(0.494545212256425,1.,3.8326409268245));
#44137=CARTESIAN_POINT('Ctrl Pts',(0.495283458893903,1.,3.82509963594156));
#44138=CARTESIAN_POINT('Ctrl Pts',(0.495963937875571,1.,3.81760756144099));
#44139=CARTESIAN_POINT('Ctrl Pts',(0.496592643443789,1.,3.81022254090909));
#44140=CARTESIAN_POINT('Ctrl Pts',(0.49717175620109,1.,3.80297788298545));
#44141=CARTESIAN_POINT('Ctrl Pts',(0.49769689210058,1.,3.79586380669959));
#44142=CARTESIAN_POINT('Ctrl Pts',(0.498152751800819,1.,3.78879701661152));
#44143=CARTESIAN_POINT('Ctrl Pts',(0.498515471679378,1.,3.78163975337189));
#44144=CARTESIAN_POINT('Ctrl Pts',(0.498759900365686,1.,3.77425499225089));
#44145=CARTESIAN_POINT('Ctrl Pts',(0.498865792335185,1.,3.76655401191144));
#44146=CARTESIAN_POINT('Ctrl Pts',(0.498823681615513,1.,3.75854082221127));
#44147=CARTESIAN_POINT('Ctrl Pts',(0.498642802042929,1.,3.75037362168103));
#44148=CARTESIAN_POINT('Ctrl Pts',(0.498350586058176,1.,3.74235701735109));
#44149=CARTESIAN_POINT('Ctrl Pts',(0.497984209510495,1.,3.73486914372834));
#44150=CARTESIAN_POINT('Ctrl Pts',(0.497584067153279,1.,3.72830430904794));
#44151=CARTESIAN_POINT('Ctrl Pts',(0.497187079575794,1.,3.72301489774241));
#44152=CARTESIAN_POINT('Ctrl Pts',(0.496846224822534,1.,3.7195232082259));
#44153=CARTESIAN_POINT('Ctrl Pts',(0.496605651526313,1.,3.71785517607694));
#44154=CARTESIAN_POINT('Ctrl Pts',(0.496446644158827,1.,3.71721917030465));
#44155=CARTESIAN_POINT('Ctrl Pts',(0.496354087925645,1.,3.71704500630521));
#44156=CARTESIAN_POINT('Ctrl Pts',(0.496319364829374,1.,3.71701050416802));
#44157=CARTESIAN_POINT('',(0.405301974318349,0.,4.18039834341342));
#44158=CARTESIAN_POINT('Ctrl Pts',(0.0913616755937418,-1.,3.74888690736767));
#44159=CARTESIAN_POINT('Ctrl Pts',(0.0913616755937418,1.,3.74888690736767));
#44160=CARTESIAN_POINT('Ctrl Pts',(0.0912992005792582,-1.,3.74882632119067));
#44161=CARTESIAN_POINT('Ctrl Pts',(0.0912992005792582,1.,3.74882632119067));
#44162=CARTESIAN_POINT('Ctrl Pts',(0.0911958743735231,-1.,3.74887017174206));
#44163=CARTESIAN_POINT('Ctrl Pts',(0.0911958743735231,1.,3.74887017174206));
#44164=CARTESIAN_POINT('Ctrl Pts',(0.0911057547506597,-1.,3.74943097853811));
#44165=CARTESIAN_POINT('Ctrl Pts',(0.0911057547506597,1.,3.74943097853811));
#44166=CARTESIAN_POINT('Ctrl Pts',(0.0911154000998139,-1.,3.75116949194623));
#44167=CARTESIAN_POINT('Ctrl Pts',(0.0911154000998139,1.,3.75116949194623));
#44168=CARTESIAN_POINT('Ctrl Pts',(0.0913419622736395,-1.,3.75495560118212));
#44169=CARTESIAN_POINT('Ctrl Pts',(0.0913419622736395,1.,3.75495560118212));
#44170=CARTESIAN_POINT('Ctrl Pts',(0.0917773084998332,-1.,3.76024199359303));
#44171=CARTESIAN_POINT('Ctrl Pts',(0.0917773084998332,1.,3.76024199359303));
#44172=CARTESIAN_POINT('Ctrl Pts',(0.0924090589602688,-1.,3.76678860031841));
#44173=CARTESIAN_POINT('Ctrl Pts',(0.0924090589602688,1.,3.76678860031841));
#44174=CARTESIAN_POINT('Ctrl Pts',(0.0932185546203175,-1.,3.77424159971059));
#44175=CARTESIAN_POINT('Ctrl Pts',(0.0932185546203175,1.,3.77424159971059));
#44176=CARTESIAN_POINT('Ctrl Pts',(0.0941840095090811,-1.,3.782205218991));
#44177=CARTESIAN_POINT('Ctrl Pts',(0.0941840095090811,1.,3.782205218991));
#44178=CARTESIAN_POINT('Ctrl Pts',(0.0952829885100798,-1.,3.79030016353111));
#44179=CARTESIAN_POINT('Ctrl Pts',(0.0952829885100798,1.,3.79030016353111));
#44180=CARTESIAN_POINT('Ctrl Pts',(0.0964949352873128,-1.,3.79822128513845));
#44181=CARTESIAN_POINT('Ctrl Pts',(0.0964949352873128,1.,3.79822128513845));
#44182=CARTESIAN_POINT('Ctrl Pts',(0.097804222290664,-1.,3.80581088847809));
#44183=CARTESIAN_POINT('Ctrl Pts',(0.097804222290664,1.,3.80581088847809));
#44184=CARTESIAN_POINT('Ctrl Pts',(0.0992008728096511,-1.,3.81306649386461));
#44185=CARTESIAN_POINT('Ctrl Pts',(0.0992008728096511,1.,3.81306649386461));
#44186=CARTESIAN_POINT('Ctrl Pts',(0.100678769650632,-1.,3.82007889742625));
#44187=CARTESIAN_POINT('Ctrl Pts',(0.100678769650632,1.,3.82007889742625));
#44188=CARTESIAN_POINT('Ctrl Pts',(0.102234506488456,-1.,3.82698737143255));
#44189=CARTESIAN_POINT('Ctrl Pts',(0.102234506488456,1.,3.82698737143255));
#44190=CARTESIAN_POINT('Ctrl Pts',(0.103866063811622,-1.,3.83393171228002));
#44191=CARTESIAN_POINT('Ctrl Pts',(0.103866063811622,1.,3.83393171228002));
#44192=CARTESIAN_POINT('Ctrl Pts',(0.105571360916569,-1.,3.84099658324803));
#44193=CARTESIAN_POINT('Ctrl Pts',(0.105571360916569,1.,3.84099658324803));
#44194=CARTESIAN_POINT('Ctrl Pts',(0.107347597812183,-1.,3.84819233070317));
#44195=CARTESIAN_POINT('Ctrl Pts',(0.107347597812183,1.,3.84819233070317));
#44196=CARTESIAN_POINT('Ctrl Pts',(0.109191717634943,-1.,3.855485714969));
#44197=CARTESIAN_POINT('Ctrl Pts',(0.109191717634943,1.,3.855485714969));
#44198=CARTESIAN_POINT('Ctrl Pts',(0.11110059303626,-1.,3.86281867282965));
#44199=CARTESIAN_POINT('Ctrl Pts',(0.11110059303626,1.,3.86281867282965));
#44200=CARTESIAN_POINT('Ctrl Pts',(0.113071304914561,-1.,3.87013043445014));
#44201=CARTESIAN_POINT('Ctrl Pts',(0.113071304914561,1.,3.87013043445014));
#44202=CARTESIAN_POINT('Ctrl Pts',(0.115101426649469,-1.,3.87738168405343));
#44203=CARTESIAN_POINT('Ctrl Pts',(0.115101426649469,1.,3.87738168405343));
#44204=CARTESIAN_POINT('Ctrl Pts',(0.117189150373144,-1.,3.88456590045767));
#44205=CARTESIAN_POINT('Ctrl Pts',(0.117189150373144,1.,3.88456590045767));
#44206=CARTESIAN_POINT('Ctrl Pts',(0.119333088190417,-1.,3.89169600105201));
#44207=CARTESIAN_POINT('Ctrl Pts',(0.119333088190417,1.,3.89169600105201));
#44208=CARTESIAN_POINT('Ctrl Pts',(0.121532144765723,-1.,3.89879639336952));
#44209=CARTESIAN_POINT('Ctrl Pts',(0.121532144765723,1.,3.89879639336952));
#44210=CARTESIAN_POINT('Ctrl Pts',(0.123785368272377,-1.,3.90589336320508));
#44211=CARTESIAN_POINT('Ctrl Pts',(0.123785368272377,1.,3.90589336320508));
#44212=CARTESIAN_POINT('Ctrl Pts',(0.126091793324136,-1.,3.91300501605392));
#44213=CARTESIAN_POINT('Ctrl Pts',(0.126091793324136,1.,3.91300501605392));
#44214=CARTESIAN_POINT('Ctrl Pts',(0.128450341339527,-1.,3.92013513251642));
#44215=CARTESIAN_POINT('Ctrl Pts',(0.128450341339527,1.,3.92013513251642));
#44216=CARTESIAN_POINT('Ctrl Pts',(0.130859892027798,-1.,3.9272787679596));
#44217=CARTESIAN_POINT('Ctrl Pts',(0.130859892027798,1.,3.9272787679596));
#44218=CARTESIAN_POINT('Ctrl Pts',(0.133319322794189,-1.,3.93442567551035));
#44219=CARTESIAN_POINT('Ctrl Pts',(0.133319322794189,1.,3.93442567551035));
#44220=CARTESIAN_POINT('Ctrl Pts',(0.135827558661187,-1.,3.94156445130744));
#44221=CARTESIAN_POINT('Ctrl Pts',(0.135827558661187,1.,3.94156445130744));
#44222=CARTESIAN_POINT('Ctrl Pts',(0.138383621255159,-1.,3.94868667844355));
#44223=CARTESIAN_POINT('Ctrl Pts',(0.138383621255159,1.,3.94868667844355));
#44224=CARTESIAN_POINT('Ctrl Pts',(0.140986665829936,-1.,3.95579014116899));
#44225=CARTESIAN_POINT('Ctrl Pts',(0.140986665829936,1.,3.95579014116899));
#44226=CARTESIAN_POINT('Ctrl Pts',(0.143635947692791,-1.,3.96287658098896));
#44227=CARTESIAN_POINT('Ctrl Pts',(0.143635947692791,1.,3.96287658098896));
#44228=CARTESIAN_POINT('Ctrl Pts',(0.146330797814513,-1.,3.96995018565891));
#44229=CARTESIAN_POINT('Ctrl Pts',(0.146330797814513,1.,3.96995018565891));
#44230=CARTESIAN_POINT('Ctrl Pts',(0.149070594803543,-1.,3.97701581473643));
#44231=CARTESIAN_POINT('Ctrl Pts',(0.149070594803543,1.,3.97701581473643));
#44232=CARTESIAN_POINT('Ctrl Pts',(0.151854737441405,-1.,3.9840772985098));
#44233=CARTESIAN_POINT('Ctrl Pts',(0.151854737441405,1.,3.9840772985098));
#44234=CARTESIAN_POINT('Ctrl Pts',(0.154682618338563,-1.,3.99113582086059));
#44235=CARTESIAN_POINT('Ctrl Pts',(0.154682618338563,1.,3.99113582086059));
#44236=CARTESIAN_POINT('Ctrl Pts',(0.157553634383809,-1.,3.99819074631874));
#44237=CARTESIAN_POINT('Ctrl Pts',(0.157553634383809,1.,3.99819074631874));
#44238=CARTESIAN_POINT('Ctrl Pts',(0.160467194882218,-1.,4.00524031064509));
#44239=CARTESIAN_POINT('Ctrl Pts',(0.160467194882218,1.,4.00524031064509));
#44240=CARTESIAN_POINT('Ctrl Pts',(0.163422730287458,-1.,4.01228237022301));
#44241=CARTESIAN_POINT('Ctrl Pts',(0.163422730287458,1.,4.01228237022301));
#44242=CARTESIAN_POINT('Ctrl Pts',(0.166419700015847,-1.,4.01931510507143));
#44243=CARTESIAN_POINT('Ctrl Pts',(0.166419700015847,1.,4.01931510507143));
#44244=CARTESIAN_POINT('Ctrl Pts',(0.169457601001653,-1.,4.0263377970371));
#44245=CARTESIAN_POINT('Ctrl Pts',(0.169457601001653,1.,4.0263377970371));
#44246=CARTESIAN_POINT('Ctrl Pts',(0.172535962484466,-1.,4.03335057326093));
#44247=CARTESIAN_POINT('Ctrl Pts',(0.172535962484466,1.,4.03335057326093));
#44248=CARTESIAN_POINT('Ctrl Pts',(0.175654339673757,-1.,4.04035407891161));
#44249=CARTESIAN_POINT('Ctrl Pts',(0.175654339673757,1.,4.04035407891161));
#44250=CARTESIAN_POINT('Ctrl Pts',(0.178812307240715,-1.,4.04734916719722));
#44251=CARTESIAN_POINT('Ctrl Pts',(0.178812307240715,1.,4.04734916719722));
#44252=CARTESIAN_POINT('Ctrl Pts',(0.18200945304855,-1.,4.05433660358402));
#44253=CARTESIAN_POINT('Ctrl Pts',(0.18200945304855,1.,4.05433660358402));
#44254=CARTESIAN_POINT('Ctrl Pts',(0.185245370038947,-1.,4.06131670998589));
#44255=CARTESIAN_POINT('Ctrl Pts',(0.185245370038947,1.,4.06131670998589));
#44256=CARTESIAN_POINT('Ctrl Pts',(0.188519658060255,-1.,4.06828941192308));
#44257=CARTESIAN_POINT('Ctrl Pts',(0.188519658060255,1.,4.06828941192308));
#44258=CARTESIAN_POINT('Ctrl Pts',(0.191831928181081,-1.,4.07525439703137));
#44259=CARTESIAN_POINT('Ctrl Pts',(0.191831928181081,1.,4.07525439703137));
#44260=CARTESIAN_POINT('Ctrl Pts',(0.195181806054714,-1.,4.08221124060385));
#44261=CARTESIAN_POINT('Ctrl Pts',(0.195181806054714,1.,4.08221124060385));
#44262=CARTESIAN_POINT('Ctrl Pts',(0.19856893480081,-1.,4.08915953359753));
#44263=CARTESIAN_POINT('Ctrl Pts',(0.19856893480081,1.,4.08915953359753));
#44264=CARTESIAN_POINT('Ctrl Pts',(0.201992979049984,-1.,4.09609903751912));
#44265=CARTESIAN_POINT('Ctrl Pts',(0.201992979049984,1.,4.09609903751912));
#44266=CARTESIAN_POINT('Ctrl Pts',(0.205453622198233,-1.,4.10302969965374));
#44267=CARTESIAN_POINT('Ctrl Pts',(0.205453622198233,1.,4.10302969965374));
#44268=CARTESIAN_POINT('Ctrl Pts',(0.208950559400171,-1.,4.10995157639026));
#44269=CARTESIAN_POINT('Ctrl Pts',(0.208950559400171,1.,4.10995157639026));
#44270=CARTESIAN_POINT('Ctrl Pts',(0.212483491087067,-1.,4.11686478264545));
#44271=CARTESIAN_POINT('Ctrl Pts',(0.212483491087067,1.,4.11686478264545));
#44272=CARTESIAN_POINT('Ctrl Pts',(0.216052116898424,-1.,4.12376943492249));
#44273=CARTESIAN_POINT('Ctrl Pts',(0.216052116898424,1.,4.12376943492249));
#44274=CARTESIAN_POINT('Ctrl Pts',(0.219656126701851,-1.,4.13066558698156));
#44275=CARTESIAN_POINT('Ctrl Pts',(0.219656126701851,1.,4.13066558698156));
#44276=CARTESIAN_POINT('Ctrl Pts',(0.223295201038383,-1.,4.13755320553563));
#44277=CARTESIAN_POINT('Ctrl Pts',(0.223295201038383,1.,4.13755320553563));
#44278=CARTESIAN_POINT('Ctrl Pts',(0.226969025061243,-1.,4.14443220607733));
#44279=CARTESIAN_POINT('Ctrl Pts',(0.226969025061243,1.,4.14443220607733));
#44280=CARTESIAN_POINT('Ctrl Pts',(0.230677299028737,-1.,4.15130247435029));
#44281=CARTESIAN_POINT('Ctrl Pts',(0.230677299028737,1.,4.15130247435029));
#44282=CARTESIAN_POINT('Ctrl Pts',(0.234419749543142,-1.,4.1581638926525));
#44283=CARTESIAN_POINT('Ctrl Pts',(0.234419749543142,1.,4.1581638926525));
#44284=CARTESIAN_POINT('Ctrl Pts',(0.238196140933976,-1.,4.1650163665385));
#44285=CARTESIAN_POINT('Ctrl Pts',(0.238196140933976,1.,4.1650163665385));
#44286=CARTESIAN_POINT('Ctrl Pts',(0.242006283923911,-1.,4.17185984409533));
#44287=CARTESIAN_POINT('Ctrl Pts',(0.242006283923911,1.,4.17185984409533));
#44288=CARTESIAN_POINT('Ctrl Pts',(0.245850033418583,-1.,4.17869430192868));
#44289=CARTESIAN_POINT('Ctrl Pts',(0.245850033418583,1.,4.17869430192868));
#44290=CARTESIAN_POINT('Ctrl Pts',(0.248951836910963,-1.,4.18415464959491));
#44291=CARTESIAN_POINT('Ctrl Pts',(0.248951836910963,1.,4.18415464959491));
#44292=CARTESIAN_POINT('Ctrl Pts',(0.251293239837692,-1.,4.18824585244066));
#44293=CARTESIAN_POINT('Ctrl Pts',(0.251293239837692,1.,4.18824585244066));
#44294=CARTESIAN_POINT('Ctrl Pts',(0.252860861572565,-1.,4.19097151819241));
#44295=CARTESIAN_POINT('Ctrl Pts',(0.252860861572565,1.,4.19097151819241));
#44296=CARTESIAN_POINT('Ctrl Pts',(0.253646344052521,-1.,4.1923339003649));
#44297=CARTESIAN_POINT('Ctrl Pts',(0.253646344052521,1.,4.1923339003649));
#44298=CARTESIAN_POINT('',(0.0912596999166814,1.,3.74888939116255));
#44299=CARTESIAN_POINT('Ctrl Pts',(0.0912596999166821,-1.,3.74888939116255));
#44300=CARTESIAN_POINT('Ctrl Pts',(0.0912596999166821,-0.666666666666667,
3.74888939116255));
#44301=CARTESIAN_POINT('Ctrl Pts',(0.0912596999166821,-0.333333333333333,
3.74888939116255));
#44302=CARTESIAN_POINT('Ctrl Pts',(0.0912596999166821,0.333333333333333,
3.74888939116255));
#44303=CARTESIAN_POINT('Ctrl Pts',(0.0912596999166819,0.666666666666667,
3.74888939116255));
#44304=CARTESIAN_POINT('Ctrl Pts',(0.0912596999166819,1.,3.74888939116255));
#44305=CARTESIAN_POINT('',(0.253646344052521,1.,4.1923339003649));
#44306=CARTESIAN_POINT('',(0.253646344052521,0.,4.1923339003649));
#44307=CARTESIAN_POINT('Ctrl Pts',(0.0912596999166818,1.,3.74888939116255));
#44308=CARTESIAN_POINT('Ctrl Pts',(0.0912308016421978,1.,3.74892890040975));
#44309=CARTESIAN_POINT('Ctrl Pts',(0.0911666301812813,1.,3.74911539914542));
#44310=CARTESIAN_POINT('Ctrl Pts',(0.0911090736805507,1.,3.74976844886347));
#44311=CARTESIAN_POINT('Ctrl Pts',(0.0911323999574424,1.,3.75145357872422));
#44312=CARTESIAN_POINT('Ctrl Pts',(0.0913419622736395,1.,3.75495560118212));
#44313=CARTESIAN_POINT('Ctrl Pts',(0.0917773084998332,1.,3.76024199359303));
#44314=CARTESIAN_POINT('Ctrl Pts',(0.0924090589602688,1.,3.76678860031841));
#44315=CARTESIAN_POINT('Ctrl Pts',(0.0932185546203175,1.,3.77424159971059));
#44316=CARTESIAN_POINT('Ctrl Pts',(0.0941840095090811,1.,3.782205218991));
#44317=CARTESIAN_POINT('Ctrl Pts',(0.0952829885100798,1.,3.79030016353111));
#44318=CARTESIAN_POINT('Ctrl Pts',(0.0964949352873128,1.,3.79822128513845));
#44319=CARTESIAN_POINT('Ctrl Pts',(0.097804222290664,1.,3.80581088847809));
#44320=CARTESIAN_POINT('Ctrl Pts',(0.0992008728096511,1.,3.81306649386461));
#44321=CARTESIAN_POINT('Ctrl Pts',(0.100678769650632,1.,3.82007889742625));
#44322=CARTESIAN_POINT('Ctrl Pts',(0.102234506488456,1.,3.82698737143255));
#44323=CARTESIAN_POINT('Ctrl Pts',(0.103866063811622,1.,3.83393171228002));
#44324=CARTESIAN_POINT('Ctrl Pts',(0.105571360916569,1.,3.84099658324803));
#44325=CARTESIAN_POINT('Ctrl Pts',(0.107347597812183,1.,3.84819233070317));
#44326=CARTESIAN_POINT('Ctrl Pts',(0.109191717634943,1.,3.855485714969));
#44327=CARTESIAN_POINT('Ctrl Pts',(0.11110059303626,1.,3.86281867282965));
#44328=CARTESIAN_POINT('Ctrl Pts',(0.113071304914561,1.,3.87013043445014));
#44329=CARTESIAN_POINT('Ctrl Pts',(0.115101426649469,1.,3.87738168405343));
#44330=CARTESIAN_POINT('Ctrl Pts',(0.117189150373144,1.,3.88456590045767));
#44331=CARTESIAN_POINT('Ctrl Pts',(0.119333088190417,1.,3.89169600105201));
#44332=CARTESIAN_POINT('Ctrl Pts',(0.121532144765723,1.,3.89879639336952));
#44333=CARTESIAN_POINT('Ctrl Pts',(0.123785368272377,1.,3.90589336320508));
#44334=CARTESIAN_POINT('Ctrl Pts',(0.126091793324136,1.,3.91300501605392));
#44335=CARTESIAN_POINT('Ctrl Pts',(0.128450341339527,1.,3.92013513251642));
#44336=CARTESIAN_POINT('Ctrl Pts',(0.130859892027798,1.,3.9272787679596));
#44337=CARTESIAN_POINT('Ctrl Pts',(0.133319322794189,1.,3.93442567551035));
#44338=CARTESIAN_POINT('Ctrl Pts',(0.135827558661187,1.,3.94156445130744));
#44339=CARTESIAN_POINT('Ctrl Pts',(0.138383621255159,1.,3.94868667844355));
#44340=CARTESIAN_POINT('Ctrl Pts',(0.140986665829936,1.,3.95579014116899));
#44341=CARTESIAN_POINT('Ctrl Pts',(0.143635947692791,1.,3.96287658098896));
#44342=CARTESIAN_POINT('Ctrl Pts',(0.146330797814513,1.,3.96995018565891));
#44343=CARTESIAN_POINT('Ctrl Pts',(0.149070594803543,1.,3.97701581473643));
#44344=CARTESIAN_POINT('Ctrl Pts',(0.151854737441405,1.,3.9840772985098));
#44345=CARTESIAN_POINT('Ctrl Pts',(0.154682618338563,1.,3.99113582086059));
#44346=CARTESIAN_POINT('Ctrl Pts',(0.157553634383809,1.,3.99819074631874));
#44347=CARTESIAN_POINT('Ctrl Pts',(0.160467194882218,1.,4.00524031064509));
#44348=CARTESIAN_POINT('Ctrl Pts',(0.163422730287458,1.,4.01228237022301));
#44349=CARTESIAN_POINT('Ctrl Pts',(0.166419700015847,1.,4.01931510507143));
#44350=CARTESIAN_POINT('Ctrl Pts',(0.169457601001653,1.,4.0263377970371));
#44351=CARTESIAN_POINT('Ctrl Pts',(0.172535962484466,1.,4.03335057326093));
#44352=CARTESIAN_POINT('Ctrl Pts',(0.175654339673757,1.,4.04035407891161));
#44353=CARTESIAN_POINT('Ctrl Pts',(0.178812307240715,1.,4.04734916719722));
#44354=CARTESIAN_POINT('Ctrl Pts',(0.18200945304855,1.,4.05433660358402));
#44355=CARTESIAN_POINT('Ctrl Pts',(0.185245370038947,1.,4.06131670998589));
#44356=CARTESIAN_POINT('Ctrl Pts',(0.188519658060255,1.,4.06828941192308));
#44357=CARTESIAN_POINT('Ctrl Pts',(0.191831928181081,1.,4.07525439703137));
#44358=CARTESIAN_POINT('Ctrl Pts',(0.195181806054714,1.,4.08221124060385));
#44359=CARTESIAN_POINT('Ctrl Pts',(0.19856893480081,1.,4.08915953359753));
#44360=CARTESIAN_POINT('Ctrl Pts',(0.201992979049984,1.,4.09609903751912));
#44361=CARTESIAN_POINT('Ctrl Pts',(0.205453622198233,1.,4.10302969965374));
#44362=CARTESIAN_POINT('Ctrl Pts',(0.208950559400171,1.,4.10995157639026));
#44363=CARTESIAN_POINT('Ctrl Pts',(0.212483491087067,1.,4.11686478264545));
#44364=CARTESIAN_POINT('Ctrl Pts',(0.216052116898424,1.,4.12376943492249));
#44365=CARTESIAN_POINT('Ctrl Pts',(0.219656126701851,1.,4.13066558698156));
#44366=CARTESIAN_POINT('Ctrl Pts',(0.223295201038383,1.,4.13755320553563));
#44367=CARTESIAN_POINT('Ctrl Pts',(0.226969025061243,1.,4.14443220607733));
#44368=CARTESIAN_POINT('Ctrl Pts',(0.230677299028737,1.,4.15130247435029));
#44369=CARTESIAN_POINT('Ctrl Pts',(0.234419749543142,1.,4.1581638926525));
#44370=CARTESIAN_POINT('Ctrl Pts',(0.238196140933976,1.,4.1650163665385));
#44371=CARTESIAN_POINT('Ctrl Pts',(0.242006283923911,1.,4.17185984409533));
#44372=CARTESIAN_POINT('Ctrl Pts',(0.245850033418583,1.,4.17869430192868));
#44373=CARTESIAN_POINT('Ctrl Pts',(0.248951836910963,1.,4.18415464959491));
#44374=CARTESIAN_POINT('Ctrl Pts',(0.251293239837692,1.,4.18824585244066));
#44375=CARTESIAN_POINT('Ctrl Pts',(0.252860861572565,1.,4.19097151819241));
#44376=CARTESIAN_POINT('Ctrl Pts',(0.253646344052521,1.,4.1923339003649));
#44377=CARTESIAN_POINT('Origin',(0.253646344052521,0.,4.1923339003649));
#44378=CARTESIAN_POINT('',(0.405301974318349,1.,4.18039834341342));
#44379=CARTESIAN_POINT('Origin',(0.,0.,0.));
#44380=CARTESIAN_POINT('',(-0.0912596999148862,1.,3.74888939116259));
#44381=CARTESIAN_POINT('Origin',(0.,1.,0.));
#44382=CARTESIAN_POINT('Ctrl Pts',(-0.0912596999148859,1.,3.74888939116259));
#44383=CARTESIAN_POINT('Ctrl Pts',(-0.0912596999148859,0.666666666666667,
3.74888939116259));
#44384=CARTESIAN_POINT('Ctrl Pts',(-0.0912596999148859,0.333333333333333,
3.74888939116259));
#44385=CARTESIAN_POINT('Ctrl Pts',(-0.0912596999148859,-0.333333333333333,
3.74888939116259));
#44386=CARTESIAN_POINT('Ctrl Pts',(-0.0912596999148859,-0.666666666666667,
3.74888939116259));
#44387=CARTESIAN_POINT('Ctrl Pts',(-0.0912596999148859,-1.,3.74888939116259));
#44388=CARTESIAN_POINT('Ctrl Pts',(-0.253646344052522,-1.,4.1923339003649));
#44389=CARTESIAN_POINT('Ctrl Pts',(-0.253646344052522,1.,4.1923339003649));
#44390=CARTESIAN_POINT('Ctrl Pts',(-0.252860861572841,-1.,4.19097151819684));
#44391=CARTESIAN_POINT('Ctrl Pts',(-0.252860861572841,1.,4.19097151819684));
#44392=CARTESIAN_POINT('Ctrl Pts',(-0.251293239838441,-1.,4.18824585245272));
#44393=CARTESIAN_POINT('Ctrl Pts',(-0.251293239838441,1.,4.18824585245272));
#44394=CARTESIAN_POINT('Ctrl Pts',(-0.248951836912189,-1.,4.18415464961466));
#44395=CARTESIAN_POINT('Ctrl Pts',(-0.248951836912189,1.,4.18415464961466));
#44396=CARTESIAN_POINT('Ctrl Pts',(-0.245850033420019,-1.,4.1786943019518));
#44397=CARTESIAN_POINT('Ctrl Pts',(-0.245850033420019,1.,4.1786943019518));
#44398=CARTESIAN_POINT('Ctrl Pts',(-0.242006283925089,-1.,4.17185984411426));
#44399=CARTESIAN_POINT('Ctrl Pts',(-0.242006283925089,1.,4.17185984411426));
#44400=CARTESIAN_POINT('Ctrl Pts',(-0.238196140934616,-1.,4.16501636654877));
#44401=CARTESIAN_POINT('Ctrl Pts',(-0.238196140934616,1.,4.16501636654877));
#44402=CARTESIAN_POINT('Ctrl Pts',(-0.234419749543208,-1.,4.15816389265352));
#44403=CARTESIAN_POINT('Ctrl Pts',(-0.234419749543208,1.,4.15816389265352));
#44404=CARTESIAN_POINT('Ctrl Pts',(-0.230677299028383,-1.,4.15130247434459));
#44405=CARTESIAN_POINT('Ctrl Pts',(-0.230677299028383,1.,4.15130247434459));
#44406=CARTESIAN_POINT('Ctrl Pts',(-0.226969025060705,-1.,4.14443220606869));
#44407=CARTESIAN_POINT('Ctrl Pts',(-0.226969025060705,1.,4.14443220606869));
#44408=CARTESIAN_POINT('Ctrl Pts',(-0.223295201037886,-1.,4.13755320552764));
#44409=CARTESIAN_POINT('Ctrl Pts',(-0.223295201037886,1.,4.13755320552764));
#44410=CARTESIAN_POINT('Ctrl Pts',(-0.219656126701542,-1.,4.13066558697658));
#44411=CARTESIAN_POINT('Ctrl Pts',(-0.219656126701542,1.,4.13066558697658));
#44412=CARTESIAN_POINT('Ctrl Pts',(-0.216052116898352,-1.,4.12376943492132));
#44413=CARTESIAN_POINT('Ctrl Pts',(-0.216052116898352,1.,4.12376943492132));
#44414=CARTESIAN_POINT('Ctrl Pts',(-0.21248349108719,-1.,4.11686478264739));
#44415=CARTESIAN_POINT('Ctrl Pts',(-0.21248349108719,1.,4.11686478264739));
#44416=CARTESIAN_POINT('Ctrl Pts',(-0.208950559400393,-1.,4.10995157639377));
#44417=CARTESIAN_POINT('Ctrl Pts',(-0.208950559400393,1.,4.10995157639377));
#44418=CARTESIAN_POINT('Ctrl Pts',(-0.205453622198455,-1.,4.10302969965728));
#44419=CARTESIAN_POINT('Ctrl Pts',(-0.205453622198455,1.,4.10302969965728));
#44420=CARTESIAN_POINT('Ctrl Pts',(-0.201992979050136,-1.,4.09609903752152));
#44421=CARTESIAN_POINT('Ctrl Pts',(-0.201992979050136,1.,4.09609903752152));
#44422=CARTESIAN_POINT('Ctrl Pts',(-0.198568934800862,-1.,4.08915953359833));
#44423=CARTESIAN_POINT('Ctrl Pts',(-0.198568934800862,1.,4.08915953359833));
#44424=CARTESIAN_POINT('Ctrl Pts',(-0.195181806054676,-1.,4.08221124060322));
#44425=CARTESIAN_POINT('Ctrl Pts',(-0.195181806054676,1.,4.08221124060322));
#44426=CARTESIAN_POINT('Ctrl Pts',(-0.191831928180991,-1.,4.07525439702992));
#44427=CARTESIAN_POINT('Ctrl Pts',(-0.191831928180991,1.,4.07525439702992));
#44428=CARTESIAN_POINT('Ctrl Pts',(-0.188519658060156,-1.,4.06828941192148));
#44429=CARTESIAN_POINT('Ctrl Pts',(-0.188519658060156,1.,4.06828941192148));
#44430=CARTESIAN_POINT('Ctrl Pts',(-0.185245370038874,-1.,4.06131670998469));
#44431=CARTESIAN_POINT('Ctrl Pts',(-0.185245370038874,1.,4.06131670998469));
#44432=CARTESIAN_POINT('Ctrl Pts',(-0.18200945304852,-1.,4.05433660358353));
#44433=CARTESIAN_POINT('Ctrl Pts',(-0.18200945304852,1.,4.05433660358353));
#44434=CARTESIAN_POINT('Ctrl Pts',(-0.178812307240729,-1.,4.04734916719741));
#44435=CARTESIAN_POINT('Ctrl Pts',(-0.178812307240729,1.,4.04734916719741));
#44436=CARTESIAN_POINT('Ctrl Pts',(-0.175654339673798,-1.,4.04035407891222));
#44437=CARTESIAN_POINT('Ctrl Pts',(-0.175654339673798,1.,4.04035407891222));
#44438=CARTESIAN_POINT('Ctrl Pts',(-0.172535962484514,-1.,4.03335057326163));
#44439=CARTESIAN_POINT('Ctrl Pts',(-0.172535962484514,1.,4.03335057326163));
#44440=CARTESIAN_POINT('Ctrl Pts',(-0.169457601001691,-1.,4.02633779703764));
#44441=CARTESIAN_POINT('Ctrl Pts',(-0.169457601001691,1.,4.02633779703764));
#44442=CARTESIAN_POINT('Ctrl Pts',(-0.166419700015866,-1.,4.01931510507167));
#44443=CARTESIAN_POINT('Ctrl Pts',(-0.166419700015866,1.,4.01931510507167));
#44444=CARTESIAN_POINT('Ctrl Pts',(-0.163422730287457,-1.,4.01228237022296));
#44445=CARTESIAN_POINT('Ctrl Pts',(-0.163422730287457,1.,4.01228237022296));
#44446=CARTESIAN_POINT('Ctrl Pts',(-0.160467194882203,-1.,4.00524031064487));
#44447=CARTESIAN_POINT('Ctrl Pts',(-0.160467194882203,1.,4.00524031064487));
#44448=CARTESIAN_POINT('Ctrl Pts',(-0.15755363438379,-1.,3.9981907463185));
#44449=CARTESIAN_POINT('Ctrl Pts',(-0.15755363438379,1.,3.9981907463185));
#44450=CARTESIAN_POINT('Ctrl Pts',(-0.154682618338548,-1.,3.99113582086043));
#44451=CARTESIAN_POINT('Ctrl Pts',(-0.154682618338548,1.,3.99113582086043));
#44452=CARTESIAN_POINT('Ctrl Pts',(-0.151854737441398,-1.,3.98407729850975));
#44453=CARTESIAN_POINT('Ctrl Pts',(-0.151854737441398,1.,3.98407729850975));
#44454=CARTESIAN_POINT('Ctrl Pts',(-0.149070594803545,-1.,3.97701581473644));
#44455=CARTESIAN_POINT('Ctrl Pts',(-0.149070594803545,1.,3.97701581473644));
#44456=CARTESIAN_POINT('Ctrl Pts',(-0.14633079781452,-1.,3.96995018565893));
#44457=CARTESIAN_POINT('Ctrl Pts',(-0.14633079781452,1.,3.96995018565893));
#44458=CARTESIAN_POINT('Ctrl Pts',(-0.143635947692799,-1.,3.96287658098896));
#44459=CARTESIAN_POINT('Ctrl Pts',(-0.143635947692799,1.,3.96287658098896));
#44460=CARTESIAN_POINT('Ctrl Pts',(-0.140986665829942,-1.,3.95579014116894));
#44461=CARTESIAN_POINT('Ctrl Pts',(-0.140986665829942,1.,3.95579014116894));
#44462=CARTESIAN_POINT('Ctrl Pts',(-0.138383621255161,-1.,3.94868667844347));
#44463=CARTESIAN_POINT('Ctrl Pts',(-0.138383621255161,1.,3.94868667844347));
#44464=CARTESIAN_POINT('Ctrl Pts',(-0.135827558661188,-1.,3.94156445130741));
#44465=CARTESIAN_POINT('Ctrl Pts',(-0.135827558661188,1.,3.94156445130741));
#44466=CARTESIAN_POINT('Ctrl Pts',(-0.133319322794191,-1.,3.93442567551042));
#44467=CARTESIAN_POINT('Ctrl Pts',(-0.133319322794191,1.,3.93442567551042));
#44468=CARTESIAN_POINT('Ctrl Pts',(-0.130859892027802,-1.,3.92727876795977));
#44469=CARTESIAN_POINT('Ctrl Pts',(-0.130859892027802,1.,3.92727876795977));
#44470=CARTESIAN_POINT('Ctrl Pts',(-0.128450341339532,-1.,3.92013513251664));
#44471=CARTESIAN_POINT('Ctrl Pts',(-0.128450341339532,1.,3.92013513251664));
#44472=CARTESIAN_POINT('Ctrl Pts',(-0.126091793324141,-1.,3.91300501605411));
#44473=CARTESIAN_POINT('Ctrl Pts',(-0.126091793324141,1.,3.91300501605411));
#44474=CARTESIAN_POINT('Ctrl Pts',(-0.12378536827238,-1.,3.90589336320515));
#44475=CARTESIAN_POINT('Ctrl Pts',(-0.12378536827238,1.,3.90589336320515));
#44476=CARTESIAN_POINT('Ctrl Pts',(-0.121532144765721,-1.,3.89879639336939));
#44477=CARTESIAN_POINT('Ctrl Pts',(-0.121532144765721,1.,3.89879639336939));
#44478=CARTESIAN_POINT('Ctrl Pts',(-0.11933308819041,-1.,3.8916960010517));
#44479=CARTESIAN_POINT('Ctrl Pts',(-0.11933308819041,1.,3.8916960010517));
#44480=CARTESIAN_POINT('Ctrl Pts',(-0.117189150373134,-1.,3.88456590045726));
#44481=CARTESIAN_POINT('Ctrl Pts',(-0.117189150373134,1.,3.88456590045726));
#44482=CARTESIAN_POINT('Ctrl Pts',(-0.115101426649461,-1.,3.87738168405308));
#44483=CARTESIAN_POINT('Ctrl Pts',(-0.115101426649461,1.,3.87738168405308));
#44484=CARTESIAN_POINT('Ctrl Pts',(-0.113071304914559,-1.,3.87013043445001));
#44485=CARTESIAN_POINT('Ctrl Pts',(-0.113071304914559,1.,3.87013043445001));
#44486=CARTESIAN_POINT('Ctrl Pts',(-0.111100593036267,-1.,3.86281867282984));
#44487=CARTESIAN_POINT('Ctrl Pts',(-0.111100593036267,1.,3.86281867282984));
#44488=CARTESIAN_POINT('Ctrl Pts',(-0.109191717634961,-1.,3.85548571496953));
#44489=CARTESIAN_POINT('Ctrl Pts',(-0.109191717634961,1.,3.85548571496953));
#44490=CARTESIAN_POINT('Ctrl Pts',(-0.107347597812208,-1.,3.84819233070391));
#44491=CARTESIAN_POINT('Ctrl Pts',(-0.107347597812208,1.,3.84819233070391));
#44492=CARTESIAN_POINT('Ctrl Pts',(-0.105571360916593,-1.,3.84099658324873));
#44493=CARTESIAN_POINT('Ctrl Pts',(-0.105571360916593,1.,3.84099658324873));
#44494=CARTESIAN_POINT('Ctrl Pts',(-0.103866063811634,-1.,3.83393171228034));
#44495=CARTESIAN_POINT('Ctrl Pts',(-0.103866063811634,1.,3.83393171228034));
#44496=CARTESIAN_POINT('Ctrl Pts',(-0.102234506488445,-1.,3.8269873714322));
#44497=CARTESIAN_POINT('Ctrl Pts',(-0.102234506488445,1.,3.8269873714322));
#44498=CARTESIAN_POINT('Ctrl Pts',(-0.100678769650594,-1.,3.82007889742512));
#44499=CARTESIAN_POINT('Ctrl Pts',(-0.100678769650594,1.,3.82007889742512));
#44500=CARTESIAN_POINT('Ctrl Pts',(-0.0992008728095946,-1.,3.81306649386293));
#44501=CARTESIAN_POINT('Ctrl Pts',(-0.0992008728095946,1.,3.81306649386293));
#44502=CARTESIAN_POINT('Ctrl Pts',(-0.0978042222906077,-1.,3.80581088847642));
#44503=CARTESIAN_POINT('Ctrl Pts',(-0.0978042222906077,1.,3.80581088847642));
#44504=CARTESIAN_POINT('Ctrl Pts',(-0.0964949352872846,-1.,3.7982212851376));
#44505=CARTESIAN_POINT('Ctrl Pts',(-0.0964949352872846,1.,3.7982212851376));
#44506=CARTESIAN_POINT('Ctrl Pts',(-0.095282988510107,-1.,3.79030016353186));
#44507=CARTESIAN_POINT('Ctrl Pts',(-0.095282988510107,1.,3.79030016353186));
#44508=CARTESIAN_POINT('Ctrl Pts',(-0.0941840095091746,-1.,3.78220521899366));
#44509=CARTESIAN_POINT('Ctrl Pts',(-0.0941840095091746,1.,3.78220521899366));
#44510=CARTESIAN_POINT('Ctrl Pts',(-0.0932185546204576,-1.,3.77424159971456));
#44511=CARTESIAN_POINT('Ctrl Pts',(-0.0932185546204576,1.,3.77424159971456));
#44512=CARTESIAN_POINT('Ctrl Pts',(-0.0924090589604057,-1.,3.76678860032228));
#44513=CARTESIAN_POINT('Ctrl Pts',(-0.0924090589604057,1.,3.76678860032228));
#44514=CARTESIAN_POINT('Ctrl Pts',(-0.091777308499901,-1.,3.76024199359493));
#44515=CARTESIAN_POINT('Ctrl Pts',(-0.091777308499901,1.,3.76024199359493));
#44516=CARTESIAN_POINT('Ctrl Pts',(-0.0913419622735854,-1.,3.75495560118053));
#44517=CARTESIAN_POINT('Ctrl Pts',(-0.0913419622735854,1.,3.75495560118053));
#44518=CARTESIAN_POINT('Ctrl Pts',(-0.0911154000996408,-1.,3.75116949194125));
#44519=CARTESIAN_POINT('Ctrl Pts',(-0.0911154000996408,1.,3.75116949194125));
#44520=CARTESIAN_POINT('Ctrl Pts',(-0.0911057547504662,-1.,3.74943097853257));
#44521=CARTESIAN_POINT('Ctrl Pts',(-0.0911057547504662,1.,3.74943097853257));
#44522=CARTESIAN_POINT('Ctrl Pts',(-0.0911958743733928,-1.,3.7488701717383));
#44523=CARTESIAN_POINT('Ctrl Pts',(-0.0911958743733928,1.,3.7488701717383));
#44524=CARTESIAN_POINT('Ctrl Pts',(-0.0912992005792093,-1.,3.74882632118923));
#44525=CARTESIAN_POINT('Ctrl Pts',(-0.0912992005792093,1.,3.74882632118923));
#44526=CARTESIAN_POINT('Ctrl Pts',(-0.0913616755937431,-1.,3.74888690736767));
#44527=CARTESIAN_POINT('Ctrl Pts',(-0.0913616755937431,1.,3.74888690736767));
#44528=CARTESIAN_POINT('',(-0.253646344052522,1.,4.1923339003649));
#44529=CARTESIAN_POINT('Ctrl Pts',(-0.253646344052522,1.,4.1923339003649));
#44530=CARTESIAN_POINT('Ctrl Pts',(-0.252860861572841,1.,4.19097151819684));
#44531=CARTESIAN_POINT('Ctrl Pts',(-0.251293239838441,1.,4.18824585245272));
#44532=CARTESIAN_POINT('Ctrl Pts',(-0.248951836912189,1.,4.18415464961466));
#44533=CARTESIAN_POINT('Ctrl Pts',(-0.245850033420019,1.,4.1786943019518));
#44534=CARTESIAN_POINT('Ctrl Pts',(-0.242006283925089,1.,4.17185984411426));
#44535=CARTESIAN_POINT('Ctrl Pts',(-0.238196140934616,1.,4.16501636654877));
#44536=CARTESIAN_POINT('Ctrl Pts',(-0.234419749543208,1.,4.15816389265352));
#44537=CARTESIAN_POINT('Ctrl Pts',(-0.230677299028383,1.,4.15130247434459));
#44538=CARTESIAN_POINT('Ctrl Pts',(-0.226969025060705,1.,4.14443220606869));
#44539=CARTESIAN_POINT('Ctrl Pts',(-0.223295201037886,1.,4.13755320552764));
#44540=CARTESIAN_POINT('Ctrl Pts',(-0.219656126701542,1.,4.13066558697658));
#44541=CARTESIAN_POINT('Ctrl Pts',(-0.216052116898352,1.,4.12376943492132));
#44542=CARTESIAN_POINT('Ctrl Pts',(-0.21248349108719,1.,4.11686478264739));
#44543=CARTESIAN_POINT('Ctrl Pts',(-0.208950559400393,1.,4.10995157639377));
#44544=CARTESIAN_POINT('Ctrl Pts',(-0.205453622198455,1.,4.10302969965728));
#44545=CARTESIAN_POINT('Ctrl Pts',(-0.201992979050136,1.,4.09609903752152));
#44546=CARTESIAN_POINT('Ctrl Pts',(-0.198568934800862,1.,4.08915953359833));
#44547=CARTESIAN_POINT('Ctrl Pts',(-0.195181806054676,1.,4.08221124060322));
#44548=CARTESIAN_POINT('Ctrl Pts',(-0.191831928180991,1.,4.07525439702992));
#44549=CARTESIAN_POINT('Ctrl Pts',(-0.188519658060156,1.,4.06828941192148));
#44550=CARTESIAN_POINT('Ctrl Pts',(-0.185245370038874,1.,4.06131670998469));
#44551=CARTESIAN_POINT('Ctrl Pts',(-0.18200945304852,1.,4.05433660358353));
#44552=CARTESIAN_POINT('Ctrl Pts',(-0.178812307240729,1.,4.04734916719741));
#44553=CARTESIAN_POINT('Ctrl Pts',(-0.175654339673798,1.,4.04035407891222));
#44554=CARTESIAN_POINT('Ctrl Pts',(-0.172535962484514,1.,4.03335057326163));
#44555=CARTESIAN_POINT('Ctrl Pts',(-0.169457601001691,1.,4.02633779703764));
#44556=CARTESIAN_POINT('Ctrl Pts',(-0.166419700015866,1.,4.01931510507167));
#44557=CARTESIAN_POINT('Ctrl Pts',(-0.163422730287457,1.,4.01228237022296));
#44558=CARTESIAN_POINT('Ctrl Pts',(-0.160467194882203,1.,4.00524031064487));
#44559=CARTESIAN_POINT('Ctrl Pts',(-0.15755363438379,1.,3.9981907463185));
#44560=CARTESIAN_POINT('Ctrl Pts',(-0.154682618338548,1.,3.99113582086043));
#44561=CARTESIAN_POINT('Ctrl Pts',(-0.151854737441398,1.,3.98407729850975));
#44562=CARTESIAN_POINT('Ctrl Pts',(-0.149070594803545,1.,3.97701581473644));
#44563=CARTESIAN_POINT('Ctrl Pts',(-0.14633079781452,1.,3.96995018565893));
#44564=CARTESIAN_POINT('Ctrl Pts',(-0.143635947692799,1.,3.96287658098896));
#44565=CARTESIAN_POINT('Ctrl Pts',(-0.140986665829942,1.,3.95579014116894));
#44566=CARTESIAN_POINT('Ctrl Pts',(-0.138383621255161,1.,3.94868667844347));
#44567=CARTESIAN_POINT('Ctrl Pts',(-0.135827558661188,1.,3.94156445130741));
#44568=CARTESIAN_POINT('Ctrl Pts',(-0.133319322794191,1.,3.93442567551042));
#44569=CARTESIAN_POINT('Ctrl Pts',(-0.130859892027802,1.,3.92727876795977));
#44570=CARTESIAN_POINT('Ctrl Pts',(-0.128450341339532,1.,3.92013513251664));
#44571=CARTESIAN_POINT('Ctrl Pts',(-0.126091793324141,1.,3.91300501605411));
#44572=CARTESIAN_POINT('Ctrl Pts',(-0.12378536827238,1.,3.90589336320515));
#44573=CARTESIAN_POINT('Ctrl Pts',(-0.121532144765721,1.,3.89879639336939));
#44574=CARTESIAN_POINT('Ctrl Pts',(-0.11933308819041,1.,3.8916960010517));
#44575=CARTESIAN_POINT('Ctrl Pts',(-0.117189150373134,1.,3.88456590045726));
#44576=CARTESIAN_POINT('Ctrl Pts',(-0.115101426649461,1.,3.87738168405308));
#44577=CARTESIAN_POINT('Ctrl Pts',(-0.113071304914559,1.,3.87013043445001));
#44578=CARTESIAN_POINT('Ctrl Pts',(-0.111100593036267,1.,3.86281867282984));
#44579=CARTESIAN_POINT('Ctrl Pts',(-0.109191717634961,1.,3.85548571496953));
#44580=CARTESIAN_POINT('Ctrl Pts',(-0.107347597812208,1.,3.84819233070391));
#44581=CARTESIAN_POINT('Ctrl Pts',(-0.105571360916593,1.,3.84099658324873));
#44582=CARTESIAN_POINT('Ctrl Pts',(-0.103866063811634,1.,3.83393171228034));
#44583=CARTESIAN_POINT('Ctrl Pts',(-0.102234506488445,1.,3.8269873714322));
#44584=CARTESIAN_POINT('Ctrl Pts',(-0.100678769650594,1.,3.82007889742512));
#44585=CARTESIAN_POINT('Ctrl Pts',(-0.0992008728095946,1.,3.81306649386293));
#44586=CARTESIAN_POINT('Ctrl Pts',(-0.0978042222906077,1.,3.80581088847642));
#44587=CARTESIAN_POINT('Ctrl Pts',(-0.0964949352872846,1.,3.7982212851376));
#44588=CARTESIAN_POINT('Ctrl Pts',(-0.095282988510107,1.,3.79030016353186));
#44589=CARTESIAN_POINT('Ctrl Pts',(-0.0941840095091746,1.,3.78220521899366));
#44590=CARTESIAN_POINT('Ctrl Pts',(-0.0932185546204576,1.,3.77424159971456));
#44591=CARTESIAN_POINT('Ctrl Pts',(-0.0924090589604057,1.,3.76678860032228));
#44592=CARTESIAN_POINT('Ctrl Pts',(-0.091777308499901,1.,3.76024199359493));
#44593=CARTESIAN_POINT('Ctrl Pts',(-0.0913419622735854,1.,3.75495560118053));
#44594=CARTESIAN_POINT('Ctrl Pts',(-0.0911323999576145,1.,3.75145357872511));
#44595=CARTESIAN_POINT('Ctrl Pts',(-0.0911090736804573,1.,3.74976844886494));
#44596=CARTESIAN_POINT('Ctrl Pts',(-0.0911666301806427,1.,3.74911539914664));
#44597=CARTESIAN_POINT('Ctrl Pts',(-0.0912308016409236,1.,3.74892890041021));
#44598=CARTESIAN_POINT('Ctrl Pts',(-0.0912596999148861,1.,3.74888939116259));
#44599=CARTESIAN_POINT('',(-0.253646344052522,0.,4.1923339003649));
#44600=CARTESIAN_POINT('Ctrl Pts',(-0.496218256089212,-1.,3.71702400346349));
#44601=CARTESIAN_POINT('Ctrl Pts',(-0.496218256089212,1.,3.71702400346349));
#44602=CARTESIAN_POINT('Ctrl Pts',(-0.496270484166409,-1.,3.7169543899574));
#44603=CARTESIAN_POINT('Ctrl Pts',(-0.496270484166409,1.,3.7169543899574));
#44604=CARTESIAN_POINT('Ctrl Pts',(-0.49637939799264,-1.,3.71698153685602));
#44605=CARTESIAN_POINT('Ctrl Pts',(-0.49637939799264,1.,3.71698153685602));
#44606=CARTESIAN_POINT('Ctrl Pts',(-0.496556137604532,-1.,3.71752134137482));
#44607=CARTESIAN_POINT('Ctrl Pts',(-0.496556137604532,1.,3.71752134137482));
#44608=CARTESIAN_POINT('Ctrl Pts',(-0.496818574420596,-1.,3.71923995966302));
#44609=CARTESIAN_POINT('Ctrl Pts',(-0.496818574420596,1.,3.71923995966302));
#44610=CARTESIAN_POINT('Ctrl Pts',(-0.497187079575988,-1.,3.72301489774398));
#44611=CARTESIAN_POINT('Ctrl Pts',(-0.497187079575988,1.,3.72301489774398));
#44612=CARTESIAN_POINT('Ctrl Pts',(-0.497584067153049,-1.,3.72830430904606));
#44613=CARTESIAN_POINT('Ctrl Pts',(-0.497584067153049,1.,3.72830430904606));
#44614=CARTESIAN_POINT('Ctrl Pts',(-0.497984209510024,-1.,3.73486914372449));
#44615=CARTESIAN_POINT('Ctrl Pts',(-0.497984209510024,1.,3.73486914372449));
#44616=CARTESIAN_POINT('Ctrl Pts',(-0.498350586057692,-1.,3.74235701734714));
#44617=CARTESIAN_POINT('Ctrl Pts',(-0.498350586057692,1.,3.74235701734714));
#44618=CARTESIAN_POINT('Ctrl Pts',(-0.498642802042606,-1.,3.75037362167839));
#44619=CARTESIAN_POINT('Ctrl Pts',(-0.498642802042606,1.,3.75037362167839));
#44620=CARTESIAN_POINT('Ctrl Pts',(-0.498823681615422,-1.,3.75854082221053));
#44621=CARTESIAN_POINT('Ctrl Pts',(-0.498823681615422,1.,3.75854082221053));
#44622=CARTESIAN_POINT('Ctrl Pts',(-0.498865792335291,-1.,3.76655401191229));
#44623=CARTESIAN_POINT('Ctrl Pts',(-0.498865792335291,1.,3.76655401191229));
#44624=CARTESIAN_POINT('Ctrl Pts',(-0.498759900365892,-1.,3.77425499225255));
#44625=CARTESIAN_POINT('Ctrl Pts',(-0.498759900365892,1.,3.77425499225255));
#44626=CARTESIAN_POINT('Ctrl Pts',(-0.498515471679585,-1.,3.78163975337356));
#44627=CARTESIAN_POINT('Ctrl Pts',(-0.498515471679585,1.,3.78163975337356));
#44628=CARTESIAN_POINT('Ctrl Pts',(-0.498152751800958,-1.,3.78879701661264));
#44629=CARTESIAN_POINT('Ctrl Pts',(-0.498152751800958,1.,3.78879701661264));
#44630=CARTESIAN_POINT('Ctrl Pts',(-0.497696892100625,-1.,3.79586380669994));
#44631=CARTESIAN_POINT('Ctrl Pts',(-0.497696892100625,1.,3.79586380669994));
#44632=CARTESIAN_POINT('Ctrl Pts',(-0.497171756201052,-1.,3.80297788298514));
#44633=CARTESIAN_POINT('Ctrl Pts',(-0.497171756201052,1.,3.80297788298514));
#44634=CARTESIAN_POINT('Ctrl Pts',(-0.496592643443704,-1.,3.81022254090839));
#44635=CARTESIAN_POINT('Ctrl Pts',(-0.496592643443704,1.,3.81022254090839));
#44636=CARTESIAN_POINT('Ctrl Pts',(-0.49596393787548,-1.,3.81760756144025));
#44637=CARTESIAN_POINT('Ctrl Pts',(-0.49596393787548,1.,3.81760756144025));
#44638=CARTESIAN_POINT('Ctrl Pts',(-0.495283458893837,-1.,3.82509963594103));
#44639=CARTESIAN_POINT('Ctrl Pts',(-0.495283458893837,1.,3.82509963594103));
#44640=CARTESIAN_POINT('Ctrl Pts',(-0.494545212256401,-1.,3.83264092682431));
#44641=CARTESIAN_POINT('Ctrl Pts',(-0.494545212256401,1.,3.83264092682431));
#44642=CARTESIAN_POINT('Ctrl Pts',(-0.493742574629135,-1.,3.84017095578451));
#44643=CARTESIAN_POINT('Ctrl Pts',(-0.493742574629135,1.,3.84017095578451));
#44644=CARTESIAN_POINT('Ctrl Pts',(-0.492871792414141,-1.,3.84765051147999));
#44645=CARTESIAN_POINT('Ctrl Pts',(-0.492871792414141,1.,3.84765051147999));
#44646=CARTESIAN_POINT('Ctrl Pts',(-0.491933631083813,-1.,3.85507287020263));
#44647=CARTESIAN_POINT('Ctrl Pts',(-0.491933631083813,1.,3.85507287020263));
#44648=CARTESIAN_POINT('Ctrl Pts',(-0.490931482170891,-1.,3.86245057319246));
#44649=CARTESIAN_POINT('Ctrl Pts',(-0.490931482170891,1.,3.86245057319246));
#44650=CARTESIAN_POINT('Ctrl Pts',(-0.489870245704918,-1.,3.86980755613707));
#44651=CARTESIAN_POINT('Ctrl Pts',(-0.489870245704918,1.,3.86980755613707));
#44652=CARTESIAN_POINT('Ctrl Pts',(-0.488754973798274,-1.,3.87716963231109));
#44653=CARTESIAN_POINT('Ctrl Pts',(-0.488754973798274,1.,3.87716963231109));
#44654=CARTESIAN_POINT('Ctrl Pts',(-0.487589452275155,-1.,3.88455453328138));
#44655=CARTESIAN_POINT('Ctrl Pts',(-0.487589452275155,1.,3.88455453328138));
#44656=CARTESIAN_POINT('Ctrl Pts',(-0.486375337854103,-1.,3.89196582437552));
#44657=CARTESIAN_POINT('Ctrl Pts',(-0.486375337854103,1.,3.89196582437552));
#44658=CARTESIAN_POINT('Ctrl Pts',(-0.485112963522222,-1.,3.89939844658513));
#44659=CARTESIAN_POINT('Ctrl Pts',(-0.485112963522222,1.,3.89939844658513));
#44660=CARTESIAN_POINT('Ctrl Pts',(-0.48380183508915,-1.,3.90684210358056));
#44661=CARTESIAN_POINT('Ctrl Pts',(-0.48380183508915,1.,3.90684210358056));
#44662=CARTESIAN_POINT('Ctrl Pts',(-0.482441230340713,-1.,3.91428536373751));
#44663=CARTESIAN_POINT('Ctrl Pts',(-0.482441230340713,1.,3.91428536373751));
#44664=CARTESIAN_POINT('Ctrl Pts',(-0.481030798910748,-1.,3.92171976072341));
#44665=CARTESIAN_POINT('Ctrl Pts',(-0.481030798910748,1.,3.92171976072341));
#44666=CARTESIAN_POINT('Ctrl Pts',(-0.479571028525579,-1.,3.92914297392071));
#44667=CARTESIAN_POINT('Ctrl Pts',(-0.479571028525579,1.,3.92914297392071));
#44668=CARTESIAN_POINT('Ctrl Pts',(-0.478062927140965,-1.,3.93655660689819));
#44669=CARTESIAN_POINT('Ctrl Pts',(-0.478062927140965,1.,3.93655660689819));
#44670=CARTESIAN_POINT('Ctrl Pts',(-0.476507810658537,-1.,3.94396469119383));
#44671=CARTESIAN_POINT('Ctrl Pts',(-0.476507810658537,1.,3.94396469119383));
#44672=CARTESIAN_POINT('Ctrl Pts',(-0.47490705302179,-1.,3.95137192932897));
#44673=CARTESIAN_POINT('Ctrl Pts',(-0.47490705302179,1.,3.95137192932897));
#44674=CARTESIAN_POINT('Ctrl Pts',(-0.473261847236297,-1.,3.95878201038338));
#44675=CARTESIAN_POINT('Ctrl Pts',(-0.473261847236297,1.,3.95878201038338));
#44676=CARTESIAN_POINT('Ctrl Pts',(-0.471572978413504,-1.,3.96619600864643));
#44677=CARTESIAN_POINT('Ctrl Pts',(-0.471572978413504,1.,3.96619600864643));
#44678=CARTESIAN_POINT('Ctrl Pts',(-0.469840942829896,-1.,3.97361320212436));
#44679=CARTESIAN_POINT('Ctrl Pts',(-0.469840942829896,1.,3.97361320212436));
#44680=CARTESIAN_POINT('Ctrl Pts',(-0.468066047920157,-1.,3.98103175589371));
#44681=CARTESIAN_POINT('Ctrl Pts',(-0.468066047920157,1.,3.98103175589371));
#44682=CARTESIAN_POINT('Ctrl Pts',(-0.46624852088304,-1.,3.98844946363262));
#44683=CARTESIAN_POINT('Ctrl Pts',(-0.46624852088304,1.,3.98844946363262));
#44684=CARTESIAN_POINT('Ctrl Pts',(-0.464388610938975,-1.,3.9958644432011));
#44685=CARTESIAN_POINT('Ctrl Pts',(-0.464388610938975,1.,3.9958644432011));
#44686=CARTESIAN_POINT('Ctrl Pts',(-0.462486702616205,-1.,4.00327590659075));
#44687=CARTESIAN_POINT('Ctrl Pts',(-0.462486702616205,1.,4.00327590659075));
#44688=CARTESIAN_POINT('Ctrl Pts',(-0.460543280768515,-1.,4.01068390573399));
#44689=CARTESIAN_POINT('Ctrl Pts',(-0.460543280768515,1.,4.01068390573399));
#44690=CARTESIAN_POINT('Ctrl Pts',(-0.458558885636946,-1.,4.01808900827587));
#44691=CARTESIAN_POINT('Ctrl Pts',(-0.458558885636946,1.,4.01808900827587));
#44692=CARTESIAN_POINT('Ctrl Pts',(-0.456534070784951,-1.,4.02549199038394));
#44693=CARTESIAN_POINT('Ctrl Pts',(-0.456534070784951,1.,4.02549199038394));
#44694=CARTESIAN_POINT('Ctrl Pts',(-0.454469363020542,-1.,4.03289354362794));
#44695=CARTESIAN_POINT('Ctrl Pts',(-0.454469363020542,1.,4.03289354362794));
#44696=CARTESIAN_POINT('Ctrl Pts',(-0.452365214748893,-1.,4.04029392228049));
#44697=CARTESIAN_POINT('Ctrl Pts',(-0.452365214748893,1.,4.04029392228049));
#44698=CARTESIAN_POINT('Ctrl Pts',(-0.450222009543927,-1.,4.0476929901813));
#44699=CARTESIAN_POINT('Ctrl Pts',(-0.450222009543927,1.,4.0476929901813));
#44700=CARTESIAN_POINT('Ctrl Pts',(-0.448040082684115,-1.,4.0550903779696));
#44701=CARTESIAN_POINT('Ctrl Pts',(-0.448040082684115,1.,4.0550903779696));
#44702=CARTESIAN_POINT('Ctrl Pts',(-0.445819737468538,-1.,4.06248560760659));
#44703=CARTESIAN_POINT('Ctrl Pts',(-0.445819737468538,1.,4.06248560760659));
#44704=CARTESIAN_POINT('Ctrl Pts',(-0.443561262395333,-1.,4.0698782192569));
#44705=CARTESIAN_POINT('Ctrl Pts',(-0.443561262395333,1.,4.0698782192569));
#44706=CARTESIAN_POINT('Ctrl Pts',(-0.441264951396361,-1.,4.07726792490016));
#44707=CARTESIAN_POINT('Ctrl Pts',(-0.441264951396361,1.,4.07726792490016));
#44708=CARTESIAN_POINT('Ctrl Pts',(-0.43893110893128,-1.,4.08465462294273));
#44709=CARTESIAN_POINT('Ctrl Pts',(-0.43893110893128,1.,4.08465462294273));
#44710=CARTESIAN_POINT('Ctrl Pts',(-0.436560044913482,-1.,4.09203832139089));
#44711=CARTESIAN_POINT('Ctrl Pts',(-0.436560044913482,1.,4.09203832139089));
#44712=CARTESIAN_POINT('Ctrl Pts',(-0.43415207320046,-1.,4.09941908688373));
#44713=CARTESIAN_POINT('Ctrl Pts',(-0.43415207320046,1.,4.09941908688373));
#44714=CARTESIAN_POINT('Ctrl Pts',(-0.431707508679884,-1.,4.10679698750336));
#44715=CARTESIAN_POINT('Ctrl Pts',(-0.431707508679884,1.,4.10679698750336));
#44716=CARTESIAN_POINT('Ctrl Pts',(-0.429226666075845,-1.,4.11417202783267));
#44717=CARTESIAN_POINT('Ctrl Pts',(-0.429226666075845,1.,4.11417202783267));
#44718=CARTESIAN_POINT('Ctrl Pts',(-0.426709855707001,-1.,4.12154412502007));
#44719=CARTESIAN_POINT('Ctrl Pts',(-0.426709855707001,1.,4.12154412502007));
#44720=CARTESIAN_POINT('Ctrl Pts',(-0.424157375323975,-1.,4.12891314634572));
#44721=CARTESIAN_POINT('Ctrl Pts',(-0.424157375323975,1.,4.12891314634572));
#44722=CARTESIAN_POINT('Ctrl Pts',(-0.421569503104513,-1.,4.13627893207002));
#44723=CARTESIAN_POINT('Ctrl Pts',(-0.421569503104513,1.,4.13627893207002));
#44724=CARTESIAN_POINT('Ctrl Pts',(-0.418946490667703,-1.,4.14364132317121));
#44725=CARTESIAN_POINT('Ctrl Pts',(-0.418946490667703,1.,4.14364132317121));
#44726=CARTESIAN_POINT('Ctrl Pts',(-0.416288556008012,-1.,4.15100018949965));
#44727=CARTESIAN_POINT('Ctrl Pts',(-0.416288556008012,1.,4.15100018949965));
#44728=CARTESIAN_POINT('Ctrl Pts',(-0.41359587795147,-1.,4.15835545017202));
#44729=CARTESIAN_POINT('Ctrl Pts',(-0.41359587795147,1.,4.15835545017202));
#44730=CARTESIAN_POINT('Ctrl Pts',(-0.410868596146414,-1.,4.16570705938425));
#44731=CARTESIAN_POINT('Ctrl Pts',(-0.410868596146414,1.,4.16570705938425));
#44732=CARTESIAN_POINT('Ctrl Pts',(-0.408659167568273,-1.,4.17158541007977));
#44733=CARTESIAN_POINT('Ctrl Pts',(-0.408659167568273,1.,4.17158541007977));
#44734=CARTESIAN_POINT('Ctrl Pts',(-0.406986596325455,-1.,4.17599251954382));
#44735=CARTESIAN_POINT('Ctrl Pts',(-0.406986596325455,1.,4.17599251954382));
#44736=CARTESIAN_POINT('Ctrl Pts',(-0.40586466267921,-1.,4.17892985789466));
#44737=CARTESIAN_POINT('Ctrl Pts',(-0.40586466267921,1.,4.17892985789466));
#44738=CARTESIAN_POINT('Ctrl Pts',(-0.40530197431835,-1.,4.18039834341342));
#44739=CARTESIAN_POINT('Ctrl Pts',(-0.40530197431835,1.,4.18039834341342));
#44740=CARTESIAN_POINT('',(-0.496319364827592,1.,3.71701050416825));
#44741=CARTESIAN_POINT('Ctrl Pts',(-0.496319364827592,-1.,3.71701050416825));
#44742=CARTESIAN_POINT('Ctrl Pts',(-0.496319364827592,-0.666666666666667,
3.71701050416825));
#44743=CARTESIAN_POINT('Ctrl Pts',(-0.496319364827592,-0.333333333333333,
3.71701050416825));
#44744=CARTESIAN_POINT('Ctrl Pts',(-0.496319364827592,0.333333333333333,
3.71701050416825));
#44745=CARTESIAN_POINT('Ctrl Pts',(-0.496319364827592,0.666666666666667,
3.71701050416825));
#44746=CARTESIAN_POINT('Ctrl Pts',(-0.496319364827592,1.,3.71701050416825));
#44747=CARTESIAN_POINT('',(-0.40530197431835,1.,4.18039834341342));
#44748=CARTESIAN_POINT('',(-0.40530197431835,0.,4.18039834341342));
#44749=CARTESIAN_POINT('Ctrl Pts',(-0.496319364827592,1.,3.71701050416825));
#44750=CARTESIAN_POINT('Ctrl Pts',(-0.496354087924313,1.,3.71704500630495));
#44751=CARTESIAN_POINT('Ctrl Pts',(-0.496446644158005,1.,3.71721917030355));
#44752=CARTESIAN_POINT('Ctrl Pts',(-0.496605651525989,1.,3.71785517607549));
#44753=CARTESIAN_POINT('Ctrl Pts',(-0.496846224822564,1.,3.71952320822499));
#44754=CARTESIAN_POINT('Ctrl Pts',(-0.497187079575988,1.,3.72301489774398));
#44755=CARTESIAN_POINT('Ctrl Pts',(-0.497584067153049,1.,3.72830430904606));
#44756=CARTESIAN_POINT('Ctrl Pts',(-0.497984209510024,1.,3.73486914372449));
#44757=CARTESIAN_POINT('Ctrl Pts',(-0.498350586057692,1.,3.74235701734714));
#44758=CARTESIAN_POINT('Ctrl Pts',(-0.498642802042606,1.,3.75037362167839));
#44759=CARTESIAN_POINT('Ctrl Pts',(-0.498823681615422,1.,3.75854082221053));
#44760=CARTESIAN_POINT('Ctrl Pts',(-0.498865792335291,1.,3.76655401191229));
#44761=CARTESIAN_POINT('Ctrl Pts',(-0.498759900365892,1.,3.77425499225255));
#44762=CARTESIAN_POINT('Ctrl Pts',(-0.498515471679585,1.,3.78163975337356));
#44763=CARTESIAN_POINT('Ctrl Pts',(-0.498152751800958,1.,3.78879701661264));
#44764=CARTESIAN_POINT('Ctrl Pts',(-0.497696892100625,1.,3.79586380669994));
#44765=CARTESIAN_POINT('Ctrl Pts',(-0.497171756201052,1.,3.80297788298514));
#44766=CARTESIAN_POINT('Ctrl Pts',(-0.496592643443704,1.,3.81022254090839));
#44767=CARTESIAN_POINT('Ctrl Pts',(-0.49596393787548,1.,3.81760756144025));
#44768=CARTESIAN_POINT('Ctrl Pts',(-0.495283458893837,1.,3.82509963594103));
#44769=CARTESIAN_POINT('Ctrl Pts',(-0.494545212256401,1.,3.83264092682431));
#44770=CARTESIAN_POINT('Ctrl Pts',(-0.493742574629135,1.,3.84017095578451));
#44771=CARTESIAN_POINT('Ctrl Pts',(-0.492871792414141,1.,3.84765051147999));
#44772=CARTESIAN_POINT('Ctrl Pts',(-0.491933631083813,1.,3.85507287020263));
#44773=CARTESIAN_POINT('Ctrl Pts',(-0.490931482170891,1.,3.86245057319246));
#44774=CARTESIAN_POINT('Ctrl Pts',(-0.489870245704918,1.,3.86980755613707));
#44775=CARTESIAN_POINT('Ctrl Pts',(-0.488754973798274,1.,3.87716963231109));
#44776=CARTESIAN_POINT('Ctrl Pts',(-0.487589452275155,1.,3.88455453328138));
#44777=CARTESIAN_POINT('Ctrl Pts',(-0.486375337854103,1.,3.89196582437552));
#44778=CARTESIAN_POINT('Ctrl Pts',(-0.485112963522222,1.,3.89939844658513));
#44779=CARTESIAN_POINT('Ctrl Pts',(-0.48380183508915,1.,3.90684210358056));
#44780=CARTESIAN_POINT('Ctrl Pts',(-0.482441230340713,1.,3.91428536373751));
#44781=CARTESIAN_POINT('Ctrl Pts',(-0.481030798910748,1.,3.92171976072341));
#44782=CARTESIAN_POINT('Ctrl Pts',(-0.479571028525579,1.,3.92914297392071));
#44783=CARTESIAN_POINT('Ctrl Pts',(-0.478062927140965,1.,3.93655660689819));
#44784=CARTESIAN_POINT('Ctrl Pts',(-0.476507810658537,1.,3.94396469119383));
#44785=CARTESIAN_POINT('Ctrl Pts',(-0.47490705302179,1.,3.95137192932897));
#44786=CARTESIAN_POINT('Ctrl Pts',(-0.473261847236297,1.,3.95878201038338));
#44787=CARTESIAN_POINT('Ctrl Pts',(-0.471572978413504,1.,3.96619600864643));
#44788=CARTESIAN_POINT('Ctrl Pts',(-0.469840942829896,1.,3.97361320212436));
#44789=CARTESIAN_POINT('Ctrl Pts',(-0.468066047920157,1.,3.98103175589371));
#44790=CARTESIAN_POINT('Ctrl Pts',(-0.46624852088304,1.,3.98844946363262));
#44791=CARTESIAN_POINT('Ctrl Pts',(-0.464388610938975,1.,3.9958644432011));
#44792=CARTESIAN_POINT('Ctrl Pts',(-0.462486702616205,1.,4.00327590659075));
#44793=CARTESIAN_POINT('Ctrl Pts',(-0.460543280768515,1.,4.01068390573399));
#44794=CARTESIAN_POINT('Ctrl Pts',(-0.458558885636946,1.,4.01808900827587));
#44795=CARTESIAN_POINT('Ctrl Pts',(-0.456534070784951,1.,4.02549199038394));
#44796=CARTESIAN_POINT('Ctrl Pts',(-0.454469363020542,1.,4.03289354362794));
#44797=CARTESIAN_POINT('Ctrl Pts',(-0.452365214748893,1.,4.04029392228049));
#44798=CARTESIAN_POINT('Ctrl Pts',(-0.450222009543927,1.,4.0476929901813));
#44799=CARTESIAN_POINT('Ctrl Pts',(-0.448040082684115,1.,4.0550903779696));
#44800=CARTESIAN_POINT('Ctrl Pts',(-0.445819737468538,1.,4.06248560760659));
#44801=CARTESIAN_POINT('Ctrl Pts',(-0.443561262395333,1.,4.0698782192569));
#44802=CARTESIAN_POINT('Ctrl Pts',(-0.441264951396361,1.,4.07726792490016));
#44803=CARTESIAN_POINT('Ctrl Pts',(-0.43893110893128,1.,4.08465462294273));
#44804=CARTESIAN_POINT('Ctrl Pts',(-0.436560044913482,1.,4.09203832139089));
#44805=CARTESIAN_POINT('Ctrl Pts',(-0.43415207320046,1.,4.09941908688373));
#44806=CARTESIAN_POINT('Ctrl Pts',(-0.431707508679884,1.,4.10679698750336));
#44807=CARTESIAN_POINT('Ctrl Pts',(-0.429226666075845,1.,4.11417202783267));
#44808=CARTESIAN_POINT('Ctrl Pts',(-0.426709855707001,1.,4.12154412502007));
#44809=CARTESIAN_POINT('Ctrl Pts',(-0.424157375323975,1.,4.12891314634572));
#44810=CARTESIAN_POINT('Ctrl Pts',(-0.421569503104513,1.,4.13627893207002));
#44811=CARTESIAN_POINT('Ctrl Pts',(-0.418946490667703,1.,4.14364132317121));
#44812=CARTESIAN_POINT('Ctrl Pts',(-0.416288556008012,1.,4.15100018949965));
#44813=CARTESIAN_POINT('Ctrl Pts',(-0.41359587795147,1.,4.15835545017202));
#44814=CARTESIAN_POINT('Ctrl Pts',(-0.410868596146414,1.,4.16570705938425));
#44815=CARTESIAN_POINT('Ctrl Pts',(-0.408659167568273,1.,4.17158541007977));
#44816=CARTESIAN_POINT('Ctrl Pts',(-0.406986596325455,1.,4.17599251954382));
#44817=CARTESIAN_POINT('Ctrl Pts',(-0.40586466267921,1.,4.17892985789466));
#44818=CARTESIAN_POINT('Ctrl Pts',(-0.40530197431835,1.,4.18039834341342));
#44819=CARTESIAN_POINT('Origin',(-0.40530197431835,0.,4.18039834341342));
#44820=CARTESIAN_POINT('',(-0.253646344052522,1.,4.1923339003649));
#44821=CARTESIAN_POINT('Origin',(0.,0.,0.));
#44822=CARTESIAN_POINT('',(-0.676591647973661,1.,3.68845817949618));
#44823=CARTESIAN_POINT('Origin',(0.,1.,0.));
#44824=CARTESIAN_POINT('Ctrl Pts',(-0.676591647973661,1.,3.68845817949618));
#44825=CARTESIAN_POINT('Ctrl Pts',(-0.676591647973661,0.666666666666667,
3.68845817949618));
#44826=CARTESIAN_POINT('Ctrl Pts',(-0.676591647973661,0.333333333333333,
3.68845817949618));
#44827=CARTESIAN_POINT('Ctrl Pts',(-0.676591647973661,-0.333333333333333,
3.68845817949618));
#44828=CARTESIAN_POINT('Ctrl Pts',(-0.676591647973661,-0.666666666666667,
3.68845817949618));
#44829=CARTESIAN_POINT('Ctrl Pts',(-0.676591647973661,-1.,3.68845817949618));
#44830=CARTESIAN_POINT('Ctrl Pts',(-0.906349047628866,-1.,4.10104028313088));
#44831=CARTESIAN_POINT('Ctrl Pts',(-0.906349047628866,1.,4.10104028313088));
#44832=CARTESIAN_POINT('Ctrl Pts',(-0.905360112216302,-1.,4.09981755067956));
#44833=CARTESIAN_POINT('Ctrl Pts',(-0.905360112216302,1.,4.09981755067956));
#44834=CARTESIAN_POINT('Ctrl Pts',(-0.903385402444213,-1.,4.09737067247114));
#44835=CARTESIAN_POINT('Ctrl Pts',(-0.903385402444213,1.,4.09737067247114));
#44836=CARTESIAN_POINT('Ctrl Pts',(-0.900432820945975,-1.,4.09369611524319));
#44837=CARTESIAN_POINT('Ctrl Pts',(-0.900432820945975,1.,4.09369611524319));
#44838=CARTESIAN_POINT('Ctrl Pts',(-0.896515019236368,-1.,4.08878822249095));
#44839=CARTESIAN_POINT('Ctrl Pts',(-0.896515019236368,1.,4.08878822249095));
#44840=CARTESIAN_POINT('Ctrl Pts',(-0.891649447920401,-1.,4.08263920306651));
#44841=CARTESIAN_POINT('Ctrl Pts',(-0.891649447920401,1.,4.08263920306651));
#44842=CARTESIAN_POINT('Ctrl Pts',(-0.886815658360739,-1.,4.07647601774639));
#44843=CARTESIAN_POINT('Ctrl Pts',(-0.886815658360739,1.,4.07647601774639));
#44844=CARTESIAN_POINT('Ctrl Pts',(-0.882013797525916,-1.,4.07029866694292));
#44845=CARTESIAN_POINT('Ctrl Pts',(-0.882013797525916,1.,4.07029866694292));
#44846=CARTESIAN_POINT('Ctrl Pts',(-0.877244060484595,-1.,4.06410717232347));
#44847=CARTESIAN_POINT('Ctrl Pts',(-0.877244060484595,1.,4.06410717232347));
#44848=CARTESIAN_POINT('Ctrl Pts',(-0.872506694780563,-1.,4.05790159030495));
#44849=CARTESIAN_POINT('Ctrl Pts',(-0.872506694780563,1.,4.05790159030495));
#44850=CARTESIAN_POINT('Ctrl Pts',(-0.867801988858176,-1.,4.05168199437128));
#44851=CARTESIAN_POINT('Ctrl Pts',(-0.867801988858176,1.,4.05168199437128));
#44852=CARTESIAN_POINT('Ctrl Pts',(-0.863130256642173,-1.,4.04544845048097));
#44853=CARTESIAN_POINT('Ctrl Pts',(-0.863130256642173,1.,4.04544845048097));
#44854=CARTESIAN_POINT('Ctrl Pts',(-0.858491822322571,-1.,4.03920099284658));
#44855=CARTESIAN_POINT('Ctrl Pts',(-0.858491822322571,1.,4.03920099284658));
#44856=CARTESIAN_POINT('Ctrl Pts',(-0.853887006632178,-1.,4.03293960436945));
#44857=CARTESIAN_POINT('Ctrl Pts',(-0.853887006632178,1.,4.03293960436945));
#44858=CARTESIAN_POINT('Ctrl Pts',(-0.849316107475012,-1.,4.02666418343508));
#44859=CARTESIAN_POINT('Ctrl Pts',(-0.849316107475012,1.,4.02666418343508));
#44860=CARTESIAN_POINT('Ctrl Pts',(-0.844779403288517,-1.,4.02037456798787));
#44861=CARTESIAN_POINT('Ctrl Pts',(-0.844779403288517,1.,4.02037456798787));
#44862=CARTESIAN_POINT('Ctrl Pts',(-0.84027717197638,-1.,4.01407059766338));
#44863=CARTESIAN_POINT('Ctrl Pts',(-0.84027717197638,1.,4.01407059766338));
#44864=CARTESIAN_POINT('Ctrl Pts',(-0.835809705809822,-1.,4.00775216907934));
#44865=CARTESIAN_POINT('Ctrl Pts',(-0.835809705809822,1.,4.00775216907934));
#44866=CARTESIAN_POINT('Ctrl Pts',(-0.831377325741487,-1.,4.00141928477447));
#44867=CARTESIAN_POINT('Ctrl Pts',(-0.831377325741487,1.,4.00141928477447));
#44868=CARTESIAN_POINT('Ctrl Pts',(-0.826980400320473,-1.,3.99507212784289));
#44869=CARTESIAN_POINT('Ctrl Pts',(-0.826980400320473,1.,3.99507212784289));
#44870=CARTESIAN_POINT('Ctrl Pts',(-0.822619346021769,-1.,3.98871104646328));
#44871=CARTESIAN_POINT('Ctrl Pts',(-0.822619346021769,1.,3.98871104646328));
#44872=CARTESIAN_POINT('Ctrl Pts',(-0.818294599022033,-1.,3.98233640155287));
#44873=CARTESIAN_POINT('Ctrl Pts',(-0.818294599022033,1.,3.98233640155287));
#44874=CARTESIAN_POINT('Ctrl Pts',(-0.814006592328737,-1.,3.97594844078763));
#44875=CARTESIAN_POINT('Ctrl Pts',(-0.814006592328737,1.,3.97594844078763));
#44876=CARTESIAN_POINT('Ctrl Pts',(-0.809755732818134,-1.,3.96954717513251));
#44877=CARTESIAN_POINT('Ctrl Pts',(-0.809755732818134,1.,3.96954717513251));
#44878=CARTESIAN_POINT('Ctrl Pts',(-0.805542372178496,-1.,3.96313222295874));
#44879=CARTESIAN_POINT('Ctrl Pts',(-0.805542372178496,1.,3.96313222295874));
#44880=CARTESIAN_POINT('Ctrl Pts',(-0.801366797727206,-1.,3.95670276375176));
#44881=CARTESIAN_POINT('Ctrl Pts',(-0.801366797727206,1.,3.95670276375176));
#44882=CARTESIAN_POINT('Ctrl Pts',(-0.797229296085438,-1.,3.95025788827189));
#44883=CARTESIAN_POINT('Ctrl Pts',(-0.797229296085438,1.,3.95025788827189));
#44884=CARTESIAN_POINT('Ctrl Pts',(-0.793130205641017,-1.,3.94379688971307));
#44885=CARTESIAN_POINT('Ctrl Pts',(-0.793130205641017,1.,3.94379688971307));
#44886=CARTESIAN_POINT('Ctrl Pts',(-0.789069971469323,-1.,3.93731956885671));
#44887=CARTESIAN_POINT('Ctrl Pts',(-0.789069971469323,1.,3.93731956885671));
#44888=CARTESIAN_POINT('Ctrl Pts',(-0.785049202786458,-1.,3.93082655631768));
#44889=CARTESIAN_POINT('Ctrl Pts',(-0.785049202786458,1.,3.93082655631768));
#44890=CARTESIAN_POINT('Ctrl Pts',(-0.781068718228395,-1.,3.92431956510418));
#44891=CARTESIAN_POINT('Ctrl Pts',(-0.781068718228395,1.,3.92431956510418));
#44892=CARTESIAN_POINT('Ctrl Pts',(-0.777129415664915,-1.,3.91780062334464));
#44893=CARTESIAN_POINT('Ctrl Pts',(-0.777129415664915,1.,3.91780062334464));
#44894=CARTESIAN_POINT('Ctrl Pts',(-0.773232154506305,-1.,3.91127138115238));
#44895=CARTESIAN_POINT('Ctrl Pts',(-0.773232154506305,1.,3.91127138115238));
#44896=CARTESIAN_POINT('Ctrl Pts',(-0.769377629847877,-1.,3.90473237182634));
#44897=CARTESIAN_POINT('Ctrl Pts',(-0.769377629847877,1.,3.90473237182634));
#44898=CARTESIAN_POINT('Ctrl Pts',(-0.765566256401306,-1.,3.89818233104381));
#44899=CARTESIAN_POINT('Ctrl Pts',(-0.765566256401306,1.,3.89818233104381));
#44900=CARTESIAN_POINT('Ctrl Pts',(-0.761798028793978,-1.,3.89161738162245));
#44901=CARTESIAN_POINT('Ctrl Pts',(-0.761798028793978,1.,3.89161738162245));
#44902=CARTESIAN_POINT('Ctrl Pts',(-0.758072800564799,-1.,3.88503262662684));
#44903=CARTESIAN_POINT('Ctrl Pts',(-0.758072800564799,1.,3.88503262662684));
#44904=CARTESIAN_POINT('Ctrl Pts',(-0.754390577396847,-1.,3.87842382520058));
#44905=CARTESIAN_POINT('Ctrl Pts',(-0.754390577396847,1.,3.87842382520058));
#44906=CARTESIAN_POINT('Ctrl Pts',(-0.750751822383024,-1.,3.87178914078372));
#44907=CARTESIAN_POINT('Ctrl Pts',(-0.750751822383024,1.,3.87178914078372));
#44908=CARTESIAN_POINT('Ctrl Pts',(-0.747157716488884,-1.,3.86513062969896));
#44909=CARTESIAN_POINT('Ctrl Pts',(-0.747157716488884,1.,3.86513062969896));
#44910=CARTESIAN_POINT('Ctrl Pts',(-0.743610542737042,-1.,3.85845645217611));
#44911=CARTESIAN_POINT('Ctrl Pts',(-0.743610542737042,1.,3.85845645217611));
#44912=CARTESIAN_POINT('Ctrl Pts',(-0.740113146827176,-1.,3.85177770351237));
#44913=CARTESIAN_POINT('Ctrl Pts',(-0.740113146827176,1.,3.85177770351237));
#44914=CARTESIAN_POINT('Ctrl Pts',(-0.736668240497151,-1.,3.84510432881231));
#44915=CARTESIAN_POINT('Ctrl Pts',(-0.736668240497151,1.,3.84510432881231));
#44916=CARTESIAN_POINT('Ctrl Pts',(-0.73327770375609,-1.,3.83844103658016));
#44917=CARTESIAN_POINT('Ctrl Pts',(-0.73327770375609,1.,3.83844103658016));
#44918=CARTESIAN_POINT('Ctrl Pts',(-0.729942010490146,-1.,3.8317839240337));
#44919=CARTESIAN_POINT('Ctrl Pts',(-0.729942010490146,1.,3.8317839240337));
#44920=CARTESIAN_POINT('Ctrl Pts',(-0.726659281876608,-1.,3.82511495756682));
#44921=CARTESIAN_POINT('Ctrl Pts',(-0.726659281876608,1.,3.82511495756682));
#44922=CARTESIAN_POINT('Ctrl Pts',(-0.723426346019349,-1.,3.81840802610795));
#44923=CARTESIAN_POINT('Ctrl Pts',(-0.723426346019349,1.,3.81840802610795));
#44924=CARTESIAN_POINT('Ctrl Pts',(-0.720240466589172,-1.,3.81163885127309));
#44925=CARTESIAN_POINT('Ctrl Pts',(-0.720240466589172,1.,3.81163885127309));
#44926=CARTESIAN_POINT('Ctrl Pts',(-0.717100993669091,-1.,3.80479445759296));
#44927=CARTESIAN_POINT('Ctrl Pts',(-0.717100993669091,1.,3.80479445759296));
#44928=CARTESIAN_POINT('Ctrl Pts',(-0.714010733006677,-1.,3.79788100314994));
#44929=CARTESIAN_POINT('Ctrl Pts',(-0.714010733006677,1.,3.79788100314994));
#44930=CARTESIAN_POINT('Ctrl Pts',(-0.710978231689117,-1.,3.79093694007146));
#44931=CARTESIAN_POINT('Ctrl Pts',(-0.710978231689117,1.,3.79093694007146));
#44932=CARTESIAN_POINT('Ctrl Pts',(-0.7080158793756,-1.,3.78402183336678));
#44933=CARTESIAN_POINT('Ctrl Pts',(-0.7080158793756,1.,3.78402183336678));
#44934=CARTESIAN_POINT('Ctrl Pts',(-0.70513584799995,-1.,3.77719254217197));
#44935=CARTESIAN_POINT('Ctrl Pts',(-0.70513584799995,1.,3.77719254217197));
#44936=CARTESIAN_POINT('Ctrl Pts',(-0.702346356621613,-1.,3.77048141872904));
#44937=CARTESIAN_POINT('Ctrl Pts',(-0.702346356621613,1.,3.77048141872904));
#44938=CARTESIAN_POINT('Ctrl Pts',(-0.699648552230851,-1.,3.76387780603725));
#44939=CARTESIAN_POINT('Ctrl Pts',(-0.699648552230851,1.,3.76387780603725));
#44940=CARTESIAN_POINT('Ctrl Pts',(-0.69703124565953,-1.,3.75729775766913));
#44941=CARTESIAN_POINT('Ctrl Pts',(-0.69703124565953,1.,3.75729775766913));
#44942=CARTESIAN_POINT('Ctrl Pts',(-0.694474562581173,-1.,3.7506028824329));
#44943=CARTESIAN_POINT('Ctrl Pts',(-0.694474562581173,1.,3.7506028824329));
#44944=CARTESIAN_POINT('Ctrl Pts',(-0.691960080400503,-1.,3.74365508986548));
#44945=CARTESIAN_POINT('Ctrl Pts',(-0.691960080400503,1.,3.74365508986548));
#44946=CARTESIAN_POINT('Ctrl Pts',(-0.689479637354651,-1.,3.73636374474993));
#44947=CARTESIAN_POINT('Ctrl Pts',(-0.689479637354651,1.,3.73636374474993));
#44948=CARTESIAN_POINT('Ctrl Pts',(-0.687043475232499,-1.,3.72872973554125));
#44949=CARTESIAN_POINT('Ctrl Pts',(-0.687043475232499,1.,3.72872973554125));
#44950=CARTESIAN_POINT('Ctrl Pts',(-0.684691698168355,-1.,3.7209063713952));
#44951=CARTESIAN_POINT('Ctrl Pts',(-0.684691698168355,1.,3.7209063713952));
#44952=CARTESIAN_POINT('Ctrl Pts',(-0.682492345109689,-1.,3.71319182790334));
#44953=CARTESIAN_POINT('Ctrl Pts',(-0.682492345109689,1.,3.71319182790334));
#44954=CARTESIAN_POINT('Ctrl Pts',(-0.680526909711618,-1.,3.70595722032165));
#44955=CARTESIAN_POINT('Ctrl Pts',(-0.680526909711618,1.,3.70595722032165));
#44956=CARTESIAN_POINT('Ctrl Pts',(-0.67887882222639,-1.,3.69959004073192));
#44957=CARTESIAN_POINT('Ctrl Pts',(-0.67887882222639,1.,3.69959004073192));
#44958=CARTESIAN_POINT('Ctrl Pts',(-0.677621861865196,-1.,3.69443683573443));
#44959=CARTESIAN_POINT('Ctrl Pts',(-0.677621861865196,1.,3.69443683573443));
#44960=CARTESIAN_POINT('Ctrl Pts',(-0.676805811074141,-1.,3.69073278191505));
#44961=CARTESIAN_POINT('Ctrl Pts',(-0.676805811074141,1.,3.69073278191505));
#44962=CARTESIAN_POINT('Ctrl Pts',(-0.676524321060167,-1.,3.68901718135636));
#44963=CARTESIAN_POINT('Ctrl Pts',(-0.676524321060167,1.,3.68901718135636));
#44964=CARTESIAN_POINT('Ctrl Pts',(-0.676525601650139,-1.,3.68844918120934));
#44965=CARTESIAN_POINT('Ctrl Pts',(-0.676525601650139,1.,3.68844918120934));
#44966=CARTESIAN_POINT('Ctrl Pts',(-0.676620796001716,-1.,3.68838970675356));
#44967=CARTESIAN_POINT('Ctrl Pts',(-0.676620796001716,1.,3.68838970675356));
#44968=CARTESIAN_POINT('Ctrl Pts',(-0.676691979611562,-1.,3.68843977377012));
#44969=CARTESIAN_POINT('Ctrl Pts',(-0.676691979611562,1.,3.68843977377012));
#44970=CARTESIAN_POINT('',(-0.906349047628866,1.,4.10104028313088));
#44971=CARTESIAN_POINT('Ctrl Pts',(-0.906349047628866,1.,4.10104028313088));
#44972=CARTESIAN_POINT('Ctrl Pts',(-0.905360112216302,1.,4.09981755067956));
#44973=CARTESIAN_POINT('Ctrl Pts',(-0.903385402444213,1.,4.09737067247114));
#44974=CARTESIAN_POINT('Ctrl Pts',(-0.900432820945975,1.,4.09369611524319));
#44975=CARTESIAN_POINT('Ctrl Pts',(-0.896515019236368,1.,4.08878822249095));
#44976=CARTESIAN_POINT('Ctrl Pts',(-0.891649447920401,1.,4.08263920306651));
#44977=CARTESIAN_POINT('Ctrl Pts',(-0.886815658360739,1.,4.07647601774639));
#44978=CARTESIAN_POINT('Ctrl Pts',(-0.882013797525916,1.,4.07029866694292));
#44979=CARTESIAN_POINT('Ctrl Pts',(-0.877244060484595,1.,4.06410717232347));
#44980=CARTESIAN_POINT('Ctrl Pts',(-0.872506694780563,1.,4.05790159030495));
#44981=CARTESIAN_POINT('Ctrl Pts',(-0.867801988858176,1.,4.05168199437128));
#44982=CARTESIAN_POINT('Ctrl Pts',(-0.863130256642173,1.,4.04544845048097));
#44983=CARTESIAN_POINT('Ctrl Pts',(-0.858491822322571,1.,4.03920099284658));
#44984=CARTESIAN_POINT('Ctrl Pts',(-0.853887006632178,1.,4.03293960436945));
#44985=CARTESIAN_POINT('Ctrl Pts',(-0.849316107475012,1.,4.02666418343508));
#44986=CARTESIAN_POINT('Ctrl Pts',(-0.844779403288517,1.,4.02037456798787));
#44987=CARTESIAN_POINT('Ctrl Pts',(-0.84027717197638,1.,4.01407059766338));
#44988=CARTESIAN_POINT('Ctrl Pts',(-0.835809705809822,1.,4.00775216907934));
#44989=CARTESIAN_POINT('Ctrl Pts',(-0.831377325741487,1.,4.00141928477447));
#44990=CARTESIAN_POINT('Ctrl Pts',(-0.826980400320473,1.,3.99507212784289));
#44991=CARTESIAN_POINT('Ctrl Pts',(-0.822619346021769,1.,3.98871104646328));
#44992=CARTESIAN_POINT('Ctrl Pts',(-0.818294599022033,1.,3.98233640155287));
#44993=CARTESIAN_POINT('Ctrl Pts',(-0.814006592328737,1.,3.97594844078763));
#44994=CARTESIAN_POINT('Ctrl Pts',(-0.809755732818134,1.,3.96954717513251));
#44995=CARTESIAN_POINT('Ctrl Pts',(-0.805542372178496,1.,3.96313222295874));
#44996=CARTESIAN_POINT('Ctrl Pts',(-0.801366797727206,1.,3.95670276375176));
#44997=CARTESIAN_POINT('Ctrl Pts',(-0.797229296085438,1.,3.95025788827189));
#44998=CARTESIAN_POINT('Ctrl Pts',(-0.793130205641017,1.,3.94379688971307));
#44999=CARTESIAN_POINT('Ctrl Pts',(-0.789069971469323,1.,3.93731956885671));
#45000=CARTESIAN_POINT('Ctrl Pts',(-0.785049202786458,1.,3.93082655631768));
#45001=CARTESIAN_POINT('Ctrl Pts',(-0.781068718228395,1.,3.92431956510418));
#45002=CARTESIAN_POINT('Ctrl Pts',(-0.777129415664915,1.,3.91780062334464));
#45003=CARTESIAN_POINT('Ctrl Pts',(-0.773232154506305,1.,3.91127138115238));
#45004=CARTESIAN_POINT('Ctrl Pts',(-0.769377629847877,1.,3.90473237182634));
#45005=CARTESIAN_POINT('Ctrl Pts',(-0.765566256401306,1.,3.89818233104381));
#45006=CARTESIAN_POINT('Ctrl Pts',(-0.761798028793978,1.,3.89161738162245));
#45007=CARTESIAN_POINT('Ctrl Pts',(-0.758072800564799,1.,3.88503262662684));
#45008=CARTESIAN_POINT('Ctrl Pts',(-0.754390577396847,1.,3.87842382520058));
#45009=CARTESIAN_POINT('Ctrl Pts',(-0.750751822383024,1.,3.87178914078372));
#45010=CARTESIAN_POINT('Ctrl Pts',(-0.747157716488884,1.,3.86513062969896));
#45011=CARTESIAN_POINT('Ctrl Pts',(-0.743610542737042,1.,3.85845645217611));
#45012=CARTESIAN_POINT('Ctrl Pts',(-0.740113146827176,1.,3.85177770351237));
#45013=CARTESIAN_POINT('Ctrl Pts',(-0.736668240497151,1.,3.84510432881231));
#45014=CARTESIAN_POINT('Ctrl Pts',(-0.73327770375609,1.,3.83844103658016));
#45015=CARTESIAN_POINT('Ctrl Pts',(-0.729942010490146,1.,3.8317839240337));
#45016=CARTESIAN_POINT('Ctrl Pts',(-0.726659281876608,1.,3.82511495756682));
#45017=CARTESIAN_POINT('Ctrl Pts',(-0.723426346019349,1.,3.81840802610795));
#45018=CARTESIAN_POINT('Ctrl Pts',(-0.720240466589172,1.,3.81163885127309));
#45019=CARTESIAN_POINT('Ctrl Pts',(-0.717100993669091,1.,3.80479445759296));
#45020=CARTESIAN_POINT('Ctrl Pts',(-0.714010733006677,1.,3.79788100314994));
#45021=CARTESIAN_POINT('Ctrl Pts',(-0.710978231689117,1.,3.79093694007146));
#45022=CARTESIAN_POINT('Ctrl Pts',(-0.7080158793756,1.,3.78402183336678));
#45023=CARTESIAN_POINT('Ctrl Pts',(-0.70513584799995,1.,3.77719254217197));
#45024=CARTESIAN_POINT('Ctrl Pts',(-0.702346356621613,1.,3.77048141872904));
#45025=CARTESIAN_POINT('Ctrl Pts',(-0.699648552230851,1.,3.76387780603725));
#45026=CARTESIAN_POINT('Ctrl Pts',(-0.69703124565953,1.,3.75729775766913));
#45027=CARTESIAN_POINT('Ctrl Pts',(-0.694474562581173,1.,3.7506028824329));
#45028=CARTESIAN_POINT('Ctrl Pts',(-0.691960080400503,1.,3.74365508986548));
#45029=CARTESIAN_POINT('Ctrl Pts',(-0.689479637354651,1.,3.73636374474993));
#45030=CARTESIAN_POINT('Ctrl Pts',(-0.687043475232499,1.,3.72872973554125));
#45031=CARTESIAN_POINT('Ctrl Pts',(-0.684691698168355,1.,3.7209063713952));
#45032=CARTESIAN_POINT('Ctrl Pts',(-0.682492345109689,1.,3.71319182790334));
#45033=CARTESIAN_POINT('Ctrl Pts',(-0.680526909711618,1.,3.70595722032165));
#45034=CARTESIAN_POINT('Ctrl Pts',(-0.67887882222639,1.,3.69959004073192));
#45035=CARTESIAN_POINT('Ctrl Pts',(-0.677621861865196,1.,3.69443683573443));
#45036=CARTESIAN_POINT('Ctrl Pts',(-0.676867042599711,1.,3.6910107117555));
#45037=CARTESIAN_POINT('Ctrl Pts',(-0.676580391119535,1.,3.68934997767391));
#45038=CARTESIAN_POINT('Ctrl Pts',(-0.676535079520366,1.,3.68869596426099));
#45039=CARTESIAN_POINT('Ctrl Pts',(-0.67656928609342,1.,3.68850172300543));
#45040=CARTESIAN_POINT('Ctrl Pts',(-0.676591647973661,1.,3.68845817949618));
#45041=CARTESIAN_POINT('',(-0.906349047628866,0.,4.10104028313088));
#45042=CARTESIAN_POINT('Ctrl Pts',(-1.07157964745328,-1.,3.59363563249864));
#45043=CARTESIAN_POINT('Ctrl Pts',(-1.07157964745328,1.,3.59363563249864));
#45044=CARTESIAN_POINT('Ctrl Pts',(-1.07162034256459,-1.,3.59355870577901));
#45045=CARTESIAN_POINT('Ctrl Pts',(-1.07162034256459,1.,3.59355870577901));
#45046=CARTESIAN_POINT('Ctrl Pts',(-1.07173216219145,-1.,3.59356848057812));
#45047=CARTESIAN_POINT('Ctrl Pts',(-1.07173216219145,1.,3.59356848057812));
#45048=CARTESIAN_POINT('Ctrl Pts',(-1.07199116987656,-1.,3.5940739910409));
#45049=CARTESIAN_POINT('Ctrl Pts',(-1.07199116987656,1.,3.5940739910409));
#45050=CARTESIAN_POINT('Ctrl Pts',(-1.07251922679245,-1.,3.59573039612316));
#45051=CARTESIAN_POINT('Ctrl Pts',(-1.07251922679245,1.,3.59573039612316));
#45052=CARTESIAN_POINT('Ctrl Pts',(-1.07347372545714,-1.,3.59940121154535));
#45053=CARTESIAN_POINT('Ctrl Pts',(-1.07347372545714,1.,3.59940121154535));
#45054=CARTESIAN_POINT('Ctrl Pts',(-1.07469327168578,-1.,3.60456339887778));
#45055=CARTESIAN_POINT('Ctrl Pts',(-1.07469327168578,1.,3.60456339887778));
#45056=CARTESIAN_POINT('Ctrl Pts',(-1.07611545402734,-1.,3.61098481349204));
#45057=CARTESIAN_POINT('Ctrl Pts',(-1.07611545402734,1.,3.61098481349204));
#45058=CARTESIAN_POINT('Ctrl Pts',(-1.07764868137619,-1.,3.61832318504574));
#45059=CARTESIAN_POINT('Ctrl Pts',(-1.07764868137619,1.,3.61832318504574));
#45060=CARTESIAN_POINT('Ctrl Pts',(-1.07919137290742,-1.,3.62619537902361));
#45061=CARTESIAN_POINT('Ctrl Pts',(-1.07919137290742,1.,3.62619537902361));
#45062=CARTESIAN_POINT('Ctrl Pts',(-1.08064765719867,-1.,3.63423373196529));
#45063=CARTESIAN_POINT('Ctrl Pts',(-1.08064765719867,1.,3.63423373196529));
#45064=CARTESIAN_POINT('Ctrl Pts',(-1.08194278850996,-1.,3.64214167843677));
#45065=CARTESIAN_POINT('Ctrl Pts',(-1.08194278850996,1.,3.64214167843677));
#45066=CARTESIAN_POINT('Ctrl Pts',(-1.08304289898623,-1.,3.64976441208358));
#45067=CARTESIAN_POINT('Ctrl Pts',(-1.08304289898623,1.,3.64976441208358));
#45068=CARTESIAN_POINT('Ctrl Pts',(-1.08395671077807,-1.,3.65709649161166));
#45069=CARTESIAN_POINT('Ctrl Pts',(-1.08395671077807,1.,3.65709649161166));
#45070=CARTESIAN_POINT('Ctrl Pts',(-1.08471809922901,-1.,3.66422237895365));
#45071=CARTESIAN_POINT('Ctrl Pts',(-1.08471809922901,1.,3.66422237895365));
#45072=CARTESIAN_POINT('Ctrl Pts',(-1.0853733414449,-1.,3.67127347729666));
#45073=CARTESIAN_POINT('Ctrl Pts',(-1.0853733414449,1.,3.67127347729666));
#45074=CARTESIAN_POINT('Ctrl Pts',(-1.0859675575576,-1.,3.67838211685117));
#45075=CARTESIAN_POINT('Ctrl Pts',(-1.0859675575576,1.,3.67838211685117));
#45076=CARTESIAN_POINT('Ctrl Pts',(-1.0865288888259,-1.,3.68562817420797));
#45077=CARTESIAN_POINT('Ctrl Pts',(-1.0865288888259,1.,3.68562817420797));
#45078=CARTESIAN_POINT('Ctrl Pts',(-1.08706319540271,-1.,3.69302062410157));
#45079=CARTESIAN_POINT('Ctrl Pts',(-1.08706319540271,1.,3.69302062410157));
#45080=CARTESIAN_POINT('Ctrl Pts',(-1.08756311291309,-1.,3.70052690909833));
#45081=CARTESIAN_POINT('Ctrl Pts',(-1.08756311291309,1.,3.70052690909833));
#45082=CARTESIAN_POINT('Ctrl Pts',(-1.08801367312185,-1.,3.70809084139457));
#45083=CARTESIAN_POINT('Ctrl Pts',(-1.08801367312185,1.,3.70809084139457));
#45084=CARTESIAN_POINT('Ctrl Pts',(-1.0883988733478,-1.,3.71565372339075));
#45085=CARTESIAN_POINT('Ctrl Pts',(-1.0883988733478,1.,3.71565372339075));
#45086=CARTESIAN_POINT('Ctrl Pts',(-1.08870887220082,-1.,3.72317741369398));
#45087=CARTESIAN_POINT('Ctrl Pts',(-1.08870887220082,1.,3.72317741369398));
#45088=CARTESIAN_POINT('Ctrl Pts',(-1.08894337390937,-1.,3.73065515162988));
#45089=CARTESIAN_POINT('Ctrl Pts',(-1.08894337390937,1.,3.73065515162988));
#45090=CARTESIAN_POINT('Ctrl Pts',(-1.08910769013297,-1.,3.73809879348239));
#45091=CARTESIAN_POINT('Ctrl Pts',(-1.08910769013297,1.,3.73809879348239));
#45092=CARTESIAN_POINT('Ctrl Pts',(-1.08921040494017,-1.,3.74553121371757));
#45093=CARTESIAN_POINT('Ctrl Pts',(-1.08921040494017,1.,3.74553121371757));
#45094=CARTESIAN_POINT('Ctrl Pts',(-1.08926054632925,-1.,3.75297711748132));
#45095=CARTESIAN_POINT('Ctrl Pts',(-1.08926054632925,1.,3.75297711748132));
#45096=CARTESIAN_POINT('Ctrl Pts',(-1.08926462734282,-1.,3.76045342580208));
#45097=CARTESIAN_POINT('Ctrl Pts',(-1.08926462734282,1.,3.76045342580208));
#45098=CARTESIAN_POINT('Ctrl Pts',(-1.08922484204256,-1.,3.76796340094448));
#45099=CARTESIAN_POINT('Ctrl Pts',(-1.08922484204256,1.,3.76796340094448));
#45100=CARTESIAN_POINT('Ctrl Pts',(-1.0891407279127,-1.,3.77550199409424));
#45101=CARTESIAN_POINT('Ctrl Pts',(-1.0891407279127,1.,3.77550199409424));
#45102=CARTESIAN_POINT('Ctrl Pts',(-1.08901018614636,-1.,3.78305911299504));
#45103=CARTESIAN_POINT('Ctrl Pts',(-1.08901018614636,1.,3.78305911299504));
#45104=CARTESIAN_POINT('Ctrl Pts',(-1.08883071512098,-1.,3.79062357974404));
#45105=CARTESIAN_POINT('Ctrl Pts',(-1.08883071512098,1.,3.79062357974404));
#45106=CARTESIAN_POINT('Ctrl Pts',(-1.08860064435778,-1.,3.79818708705259));
#45107=CARTESIAN_POINT('Ctrl Pts',(-1.08860064435778,1.,3.79818708705259));
#45108=CARTESIAN_POINT('Ctrl Pts',(-1.0883200925538,-1.,3.8057472665766));
#45109=CARTESIAN_POINT('Ctrl Pts',(-1.0883200925538,1.,3.8057472665766));
#45110=CARTESIAN_POINT('Ctrl Pts',(-1.08799030610862,-1.,3.81330554446323));
#45111=CARTESIAN_POINT('Ctrl Pts',(-1.08799030610862,1.,3.81330554446323));
#45112=CARTESIAN_POINT('Ctrl Pts',(-1.08761321539442,-1.,3.82086569676319));
#45113=CARTESIAN_POINT('Ctrl Pts',(-1.08761321539442,1.,3.82086569676319));
#45114=CARTESIAN_POINT('Ctrl Pts',(-1.08719091307558,-1.,3.82843215316984));
#45115=CARTESIAN_POINT('Ctrl Pts',(-1.08719091307558,1.,3.82843215316984));
#45116=CARTESIAN_POINT('Ctrl Pts',(-1.08672515456902,-1.,3.83600837071708));
#45117=CARTESIAN_POINT('Ctrl Pts',(-1.08672515456902,1.,3.83600837071708));
#45118=CARTESIAN_POINT('Ctrl Pts',(-1.08621688337604,-1.,3.8435952876495));
#45119=CARTESIAN_POINT('Ctrl Pts',(-1.08621688337604,1.,3.8435952876495));
#45120=CARTESIAN_POINT('Ctrl Pts',(-1.08566647671844,-1.,3.85119211322755));
#45121=CARTESIAN_POINT('Ctrl Pts',(-1.08566647671844,1.,3.85119211322755));
#45122=CARTESIAN_POINT('Ctrl Pts',(-1.08507395120059,-1.,3.85879698702532));
#45123=CARTESIAN_POINT('Ctrl Pts',(-1.08507395120059,1.,3.85879698702532));
#45124=CARTESIAN_POINT('Ctrl Pts',(-1.08443918607927,-1.,3.86640769434274));
#45125=CARTESIAN_POINT('Ctrl Pts',(-1.08443918607927,1.,3.86640769434274));
#45126=CARTESIAN_POINT('Ctrl Pts',(-1.08376213307504,-1.,3.8740223372254));
#45127=CARTESIAN_POINT('Ctrl Pts',(-1.08376213307504,1.,3.8740223372254));
#45128=CARTESIAN_POINT('Ctrl Pts',(-1.08304304871028,-1.,3.88164007721312));
#45129=CARTESIAN_POINT('Ctrl Pts',(-1.08304304871028,1.,3.88164007721312));
#45130=CARTESIAN_POINT('Ctrl Pts',(-1.08228241999346,-1.,3.88926088975114));
#45131=CARTESIAN_POINT('Ctrl Pts',(-1.08228241999346,1.,3.88926088975114));
#45132=CARTESIAN_POINT('Ctrl Pts',(-1.08148086931358,-1.,3.8968852509835));
#45133=CARTESIAN_POINT('Ctrl Pts',(-1.08148086931358,1.,3.8968852509835));
#45134=CARTESIAN_POINT('Ctrl Pts',(-1.08063906483818,-1.,3.90451384092545));
#45135=CARTESIAN_POINT('Ctrl Pts',(-1.08063906483818,1.,3.90451384092545));
#45136=CARTESIAN_POINT('Ctrl Pts',(-1.07975763507473,-1.,3.91214726022143));
#45137=CARTESIAN_POINT('Ctrl Pts',(-1.07975763507473,1.,3.91214726022143));
#45138=CARTESIAN_POINT('Ctrl Pts',(-1.07883706663554,-1.,3.91978568924178));
#45139=CARTESIAN_POINT('Ctrl Pts',(-1.07883706663554,1.,3.91978568924178));
#45140=CARTESIAN_POINT('Ctrl Pts',(-1.07787771707195,-1.,3.9274289334984));
#45141=CARTESIAN_POINT('Ctrl Pts',(-1.07787771707195,1.,3.9274289334984));
#45142=CARTESIAN_POINT('Ctrl Pts',(-1.07687985975384,-1.,3.93507657572883));
#45143=CARTESIAN_POINT('Ctrl Pts',(-1.07687985975384,1.,3.93507657572883));
#45144=CARTESIAN_POINT('Ctrl Pts',(-1.07584371946443,-1.,3.94272809633331));
#45145=CARTESIAN_POINT('Ctrl Pts',(-1.07584371946443,1.,3.94272809633331));
#45146=CARTESIAN_POINT('Ctrl Pts',(-1.07476950921587,-1.,3.95038299600676));
#45147=CARTESIAN_POINT('Ctrl Pts',(-1.07476950921587,1.,3.95038299600676));
#45148=CARTESIAN_POINT('Ctrl Pts',(-1.07365747426491,-1.,3.95804094429373));
#45149=CARTESIAN_POINT('Ctrl Pts',(-1.07365747426491,1.,3.95804094429373));
#45150=CARTESIAN_POINT('Ctrl Pts',(-1.07250789943007,-1.,3.96570179322338));
#45151=CARTESIAN_POINT('Ctrl Pts',(-1.07250789943007,1.,3.96570179322338));
#45152=CARTESIAN_POINT('Ctrl Pts',(-1.07132109206164,-1.,3.9733655022223));
#45153=CARTESIAN_POINT('Ctrl Pts',(-1.07132109206164,1.,3.9733655022223));
#45154=CARTESIAN_POINT('Ctrl Pts',(-1.07009737257767,-1.,3.98103208801101));
#45155=CARTESIAN_POINT('Ctrl Pts',(-1.07009737257767,1.,3.98103208801101));
#45156=CARTESIAN_POINT('Ctrl Pts',(-1.06883706263942,-1.,3.98870156857412));
#45157=CARTESIAN_POINT('Ctrl Pts',(-1.06883706263942,1.,3.98870156857412));
#45158=CARTESIAN_POINT('Ctrl Pts',(-1.06754047381312,-1.,3.99637389920441));
#45159=CARTESIAN_POINT('Ctrl Pts',(-1.06754047381312,1.,3.99637389920441));
#45160=CARTESIAN_POINT('Ctrl Pts',(-1.06620789963606,-1.,4.00404894952579));
#45161=CARTESIAN_POINT('Ctrl Pts',(-1.06620789963606,1.,4.00404894952579));
#45162=CARTESIAN_POINT('Ctrl Pts',(-1.06483961343109,-1.,4.01172654187398));
#45163=CARTESIAN_POINT('Ctrl Pts',(-1.06483961343109,1.,4.01172654187398));
#45164=CARTESIAN_POINT('Ctrl Pts',(-1.06343586496236,-1.,4.01940647495943));
#45165=CARTESIAN_POINT('Ctrl Pts',(-1.06343586496236,1.,4.01940647495943));
#45166=CARTESIAN_POINT('Ctrl Pts',(-1.06199687787462,-1.,4.02708855235633));
#45167=CARTESIAN_POINT('Ctrl Pts',(-1.06199687787462,1.,4.02708855235633));
#45168=CARTESIAN_POINT('Ctrl Pts',(-1.06052284711857,-1.,4.03477261141553));
#45169=CARTESIAN_POINT('Ctrl Pts',(-1.06052284711857,1.,4.03477261141553));
#45170=CARTESIAN_POINT('Ctrl Pts',(-1.05901393666566,-1.,4.04245854427496));
#45171=CARTESIAN_POINT('Ctrl Pts',(-1.05901393666566,1.,4.04245854427496));
#45172=CARTESIAN_POINT('Ctrl Pts',(-1.05747027727959,-1.,4.05014628384869));
#45173=CARTESIAN_POINT('Ctrl Pts',(-1.05747027727959,1.,4.05014628384869));
#45174=CARTESIAN_POINT('Ctrl Pts',(-1.05620762707996,-1.,4.05629789307025));
#45175=CARTESIAN_POINT('Ctrl Pts',(-1.05620762707996,1.,4.05629789307025));
#45176=CARTESIAN_POINT('Ctrl Pts',(-1.055245071776,-1.,4.06091239149123));
#45177=CARTESIAN_POINT('Ctrl Pts',(-1.055245071776,1.,4.06091239149123));
#45178=CARTESIAN_POINT('Ctrl Pts',(-1.05459645194823,-1.,4.06398907542249));
#45179=CARTESIAN_POINT('Ctrl Pts',(-1.05459645194823,1.,4.06398907542249));
#45180=CARTESIAN_POINT('Ctrl Pts',(-1.05427041296137,-1.,4.06552750530042));
#45181=CARTESIAN_POINT('Ctrl Pts',(-1.05427041296137,1.,4.06552750530042));
#45182=CARTESIAN_POINT('',(-1.07167739962028,1.,3.59360648251073));
#45183=CARTESIAN_POINT('Ctrl Pts',(-1.07167739962028,-1.,3.59360648251073));
#45184=CARTESIAN_POINT('Ctrl Pts',(-1.07167739962028,-0.666666666666667,
3.59360648251073));
#45185=CARTESIAN_POINT('Ctrl Pts',(-1.07167739962028,-0.333333333333333,
3.59360648251073));
#45186=CARTESIAN_POINT('Ctrl Pts',(-1.07167739962028,0.333333333333333,
3.59360648251073));
#45187=CARTESIAN_POINT('Ctrl Pts',(-1.07167739962028,0.666666666666667,
3.59360648251073));
#45188=CARTESIAN_POINT('Ctrl Pts',(-1.07167739962028,1.,3.59360648251073));
#45189=CARTESIAN_POINT('',(-1.05427041296137,1.,4.06552750530042));
#45190=CARTESIAN_POINT('',(-1.05427041296137,0.,4.06552750530042));
#45191=CARTESIAN_POINT('Ctrl Pts',(-1.07167739962028,1.,3.59360648251073));
#45192=CARTESIAN_POINT('Ctrl Pts',(-1.07171709254135,1.,3.5936351279798));
#45193=CARTESIAN_POINT('Ctrl Pts',(-1.07183575450617,1.,3.59379266874567));
#45194=CARTESIAN_POINT('Ctrl Pts',(-1.07209229745229,1.,3.59439596999862));
#45195=CARTESIAN_POINT('Ctrl Pts',(-1.07259084660936,1.,3.59600583194946));
#45196=CARTESIAN_POINT('Ctrl Pts',(-1.07347372545714,1.,3.59940121154535));
#45197=CARTESIAN_POINT('Ctrl Pts',(-1.07469327168578,1.,3.60456339887778));
#45198=CARTESIAN_POINT('Ctrl Pts',(-1.07611545402734,1.,3.61098481349204));
#45199=CARTESIAN_POINT('Ctrl Pts',(-1.07764868137619,1.,3.61832318504574));
#45200=CARTESIAN_POINT('Ctrl Pts',(-1.07919137290742,1.,3.62619537902361));
#45201=CARTESIAN_POINT('Ctrl Pts',(-1.08064765719867,1.,3.63423373196529));
#45202=CARTESIAN_POINT('Ctrl Pts',(-1.08194278850996,1.,3.64214167843677));
#45203=CARTESIAN_POINT('Ctrl Pts',(-1.08304289898623,1.,3.64976441208358));
#45204=CARTESIAN_POINT('Ctrl Pts',(-1.08395671077807,1.,3.65709649161166));
#45205=CARTESIAN_POINT('Ctrl Pts',(-1.08471809922901,1.,3.66422237895365));
#45206=CARTESIAN_POINT('Ctrl Pts',(-1.0853733414449,1.,3.67127347729666));
#45207=CARTESIAN_POINT('Ctrl Pts',(-1.0859675575576,1.,3.67838211685117));
#45208=CARTESIAN_POINT('Ctrl Pts',(-1.0865288888259,1.,3.68562817420797));
#45209=CARTESIAN_POINT('Ctrl Pts',(-1.08706319540271,1.,3.69302062410157));
#45210=CARTESIAN_POINT('Ctrl Pts',(-1.08756311291309,1.,3.70052690909833));
#45211=CARTESIAN_POINT('Ctrl Pts',(-1.08801367312185,1.,3.70809084139457));
#45212=CARTESIAN_POINT('Ctrl Pts',(-1.0883988733478,1.,3.71565372339075));
#45213=CARTESIAN_POINT('Ctrl Pts',(-1.08870887220082,1.,3.72317741369398));
#45214=CARTESIAN_POINT('Ctrl Pts',(-1.08894337390937,1.,3.73065515162988));
#45215=CARTESIAN_POINT('Ctrl Pts',(-1.08910769013297,1.,3.73809879348239));
#45216=CARTESIAN_POINT('Ctrl Pts',(-1.08921040494017,1.,3.74553121371757));
#45217=CARTESIAN_POINT('Ctrl Pts',(-1.08926054632925,1.,3.75297711748132));
#45218=CARTESIAN_POINT('Ctrl Pts',(-1.08926462734282,1.,3.76045342580208));
#45219=CARTESIAN_POINT('Ctrl Pts',(-1.08922484204256,1.,3.76796340094448));
#45220=CARTESIAN_POINT('Ctrl Pts',(-1.0891407279127,1.,3.77550199409424));
#45221=CARTESIAN_POINT('Ctrl Pts',(-1.08901018614636,1.,3.78305911299504));
#45222=CARTESIAN_POINT('Ctrl Pts',(-1.08883071512098,1.,3.79062357974404));
#45223=CARTESIAN_POINT('Ctrl Pts',(-1.08860064435778,1.,3.79818708705259));
#45224=CARTESIAN_POINT('Ctrl Pts',(-1.0883200925538,1.,3.8057472665766));
#45225=CARTESIAN_POINT('Ctrl Pts',(-1.08799030610862,1.,3.81330554446323));
#45226=CARTESIAN_POINT('Ctrl Pts',(-1.08761321539442,1.,3.82086569676319));
#45227=CARTESIAN_POINT('Ctrl Pts',(-1.08719091307558,1.,3.82843215316984));
#45228=CARTESIAN_POINT('Ctrl Pts',(-1.08672515456902,1.,3.83600837071708));
#45229=CARTESIAN_POINT('Ctrl Pts',(-1.08621688337604,1.,3.8435952876495));
#45230=CARTESIAN_POINT('Ctrl Pts',(-1.08566647671844,1.,3.85119211322755));
#45231=CARTESIAN_POINT('Ctrl Pts',(-1.08507395120059,1.,3.85879698702532));
#45232=CARTESIAN_POINT('Ctrl Pts',(-1.08443918607927,1.,3.86640769434274));
#45233=CARTESIAN_POINT('Ctrl Pts',(-1.08376213307504,1.,3.8740223372254));
#45234=CARTESIAN_POINT('Ctrl Pts',(-1.08304304871028,1.,3.88164007721312));
#45235=CARTESIAN_POINT('Ctrl Pts',(-1.08228241999346,1.,3.88926088975114));
#45236=CARTESIAN_POINT('Ctrl Pts',(-1.08148086931358,1.,3.8968852509835));
#45237=CARTESIAN_POINT('Ctrl Pts',(-1.08063906483818,1.,3.90451384092545));
#45238=CARTESIAN_POINT('Ctrl Pts',(-1.07975763507473,1.,3.91214726022143));
#45239=CARTESIAN_POINT('Ctrl Pts',(-1.07883706663554,1.,3.91978568924178));
#45240=CARTESIAN_POINT('Ctrl Pts',(-1.07787771707195,1.,3.9274289334984));
#45241=CARTESIAN_POINT('Ctrl Pts',(-1.07687985975384,1.,3.93507657572883));
#45242=CARTESIAN_POINT('Ctrl Pts',(-1.07584371946443,1.,3.94272809633331));
#45243=CARTESIAN_POINT('Ctrl Pts',(-1.07476950921587,1.,3.95038299600676));
#45244=CARTESIAN_POINT('Ctrl Pts',(-1.07365747426491,1.,3.95804094429373));
#45245=CARTESIAN_POINT('Ctrl Pts',(-1.07250789943007,1.,3.96570179322338));
#45246=CARTESIAN_POINT('Ctrl Pts',(-1.07132109206164,1.,3.9733655022223));
#45247=CARTESIAN_POINT('Ctrl Pts',(-1.07009737257767,1.,3.98103208801101));
#45248=CARTESIAN_POINT('Ctrl Pts',(-1.06883706263942,1.,3.98870156857412));
#45249=CARTESIAN_POINT('Ctrl Pts',(-1.06754047381312,1.,3.99637389920441));
#45250=CARTESIAN_POINT('Ctrl Pts',(-1.06620789963606,1.,4.00404894952579));
#45251=CARTESIAN_POINT('Ctrl Pts',(-1.06483961343109,1.,4.01172654187398));
#45252=CARTESIAN_POINT('Ctrl Pts',(-1.06343586496236,1.,4.01940647495943));
#45253=CARTESIAN_POINT('Ctrl Pts',(-1.06199687787462,1.,4.02708855235633));
#45254=CARTESIAN_POINT('Ctrl Pts',(-1.06052284711857,1.,4.03477261141553));
#45255=CARTESIAN_POINT('Ctrl Pts',(-1.05901393666566,1.,4.04245854427496));
#45256=CARTESIAN_POINT('Ctrl Pts',(-1.05747027727959,1.,4.05014628384869));
#45257=CARTESIAN_POINT('Ctrl Pts',(-1.05620762707996,1.,4.05629789307025));
#45258=CARTESIAN_POINT('Ctrl Pts',(-1.055245071776,1.,4.06091239149123));
#45259=CARTESIAN_POINT('Ctrl Pts',(-1.05459645194823,1.,4.06398907542249));
#45260=CARTESIAN_POINT('Ctrl Pts',(-1.05427041296137,1.,4.06552750530042));
#45261=CARTESIAN_POINT('Origin',(-1.05427041296137,0.,4.06552750530042));
#45262=CARTESIAN_POINT('',(-0.906349047628866,1.,4.10104028313088));
#45263=CARTESIAN_POINT('Origin',(0.,0.,0.));
#45264=CARTESIAN_POINT('',(-1.24526366418038,1.,3.5372048861597));
#45265=CARTESIAN_POINT('Origin',(0.,1.,0.));
#45266=CARTESIAN_POINT('Ctrl Pts',(-1.24526366418038,1.,3.5372048861597));
#45267=CARTESIAN_POINT('Ctrl Pts',(-1.24526366418038,0.666666666666667,
3.5372048861597));
#45268=CARTESIAN_POINT('Ctrl Pts',(-1.24526366418038,0.333333333333333,
3.5372048861597));
#45269=CARTESIAN_POINT('Ctrl Pts',(-1.24526366418038,-0.333333333333333,
3.5372048861597));
#45270=CARTESIAN_POINT('Ctrl Pts',(-1.24526366418038,-0.666666666666667,
3.5372048861597));
#45271=CARTESIAN_POINT('Ctrl Pts',(-1.24526366418038,-1.,3.5372048861597));
#45272=CARTESIAN_POINT('Ctrl Pts',(-1.53673442965256,-1.,3.90876544355381));
#45273=CARTESIAN_POINT('Ctrl Pts',(-1.53673442965256,1.,3.90876544355381));
#45274=CARTESIAN_POINT('Ctrl Pts',(-1.53556639217905,-1.,3.90771246855019));
#45275=CARTESIAN_POINT('Ctrl Pts',(-1.53556639217905,1.,3.90771246855019));
#45276=CARTESIAN_POINT('Ctrl Pts',(-1.53323321827755,-1.,3.90560462813969));
#45277=CARTESIAN_POINT('Ctrl Pts',(-1.53323321827755,1.,3.90560462813969));
#45278=CARTESIAN_POINT('Ctrl Pts',(-1.52974216056287,-1.,3.90243719631596));
#45279=CARTESIAN_POINT('Ctrl Pts',(-1.52974216056287,1.,3.90243719631596));
#45280=CARTESIAN_POINT('Ctrl Pts',(-1.52510482991635,-1.,3.89820260708225));
#45281=CARTESIAN_POINT('Ctrl Pts',(-1.52510482991635,1.,3.89820260708225));
#45282=CARTESIAN_POINT('Ctrl Pts',(-1.51933724329306,-1.,3.89289043533657));
#45283=CARTESIAN_POINT('Ctrl Pts',(-1.51933724329306,1.,3.89289043533657));
#45284=CARTESIAN_POINT('Ctrl Pts',(-1.51359883110559,-1.,3.88755930033884));
#45285=CARTESIAN_POINT('Ctrl Pts',(-1.51359883110559,1.,3.88755930033884));
#45286=CARTESIAN_POINT('Ctrl Pts',(-1.50788973857757,-1.,3.88220917950538));
#45287=CARTESIAN_POINT('Ctrl Pts',(-1.50788973857757,1.,3.88220917950538));
#45288=CARTESIAN_POINT('Ctrl Pts',(-1.50221016176556,-1.,3.87684006372134));
#45289=CARTESIAN_POINT('Ctrl Pts',(-1.50221016176556,1.,3.87684006372134));
#45290=CARTESIAN_POINT('Ctrl Pts',(-1.49656035399122,-1.,3.87145196998465));
#45291=CARTESIAN_POINT('Ctrl Pts',(-1.49656035399122,1.,3.87145196998465));
#45292=CARTESIAN_POINT('Ctrl Pts',(-1.4909406116431,-1.,3.86604492575189));
#45293=CARTESIAN_POINT('Ctrl Pts',(-1.4909406116431,1.,3.86604492575189));
#45294=CARTESIAN_POINT('Ctrl Pts',(-1.48535125509919,-1.,3.86061894706087));
#45295=CARTESIAN_POINT('Ctrl Pts',(-1.48535125509919,1.,3.86061894706087));
#45296=CARTESIAN_POINT('Ctrl Pts',(-1.4797926099102,-1.,3.85517401698843));
#45297=CARTESIAN_POINT('Ctrl Pts',(-1.4797926099102,1.,3.85517401698843));
#45298=CARTESIAN_POINT('Ctrl Pts',(-1.47426499018538,-1.,3.84971006847277));
#45299=CARTESIAN_POINT('Ctrl Pts',(-1.47426499018538,1.,3.84971006847277));
#45300=CARTESIAN_POINT('Ctrl Pts',(-1.46876867426504,-1.,3.84422695454796));
#45301=CARTESIAN_POINT('Ctrl Pts',(-1.46876867426504,1.,3.84422695454796));
#45302=CARTESIAN_POINT('Ctrl Pts',(-1.46330391180752,-1.,3.83872447159639));
#45303=CARTESIAN_POINT('Ctrl Pts',(-1.46330391180752,1.,3.83872447159639));
#45304=CARTESIAN_POINT('Ctrl Pts',(-1.45787095220852,-1.,3.83320241775423));
#45305=CARTESIAN_POINT('Ctrl Pts',(-1.45787095220852,1.,3.83320241775423));
#45306=CARTESIAN_POINT('Ctrl Pts',(-1.45247006796836,-1.,3.82766064519074));
#45307=CARTESIAN_POINT('Ctrl Pts',(-1.45247006796836,1.,3.82766064519074));
#45308=CARTESIAN_POINT('Ctrl Pts',(-1.44710157648539,-1.,3.82209910620533));
#45309=CARTESIAN_POINT('Ctrl Pts',(-1.44710157648539,1.,3.82209910620533));
#45310=CARTESIAN_POINT('Ctrl Pts',(-1.44176587041347,-1.,3.81651792398414));
#45311=CARTESIAN_POINT('Ctrl Pts',(-1.44176587041347,1.,3.81651792398414));
#45312=CARTESIAN_POINT('Ctrl Pts',(-1.43646341556724,-1.,3.81091737726815));
#45313=CARTESIAN_POINT('Ctrl Pts',(-1.43646341556724,1.,3.81091737726815));
#45314=CARTESIAN_POINT('Ctrl Pts',(-1.4311946992132,-1.,3.80529775429805));
#45315=CARTESIAN_POINT('Ctrl Pts',(-1.4311946992132,1.,3.80529775429805));
#45316=CARTESIAN_POINT('Ctrl Pts',(-1.42596018777283,-1.,3.7996592319632));
#45317=CARTESIAN_POINT('Ctrl Pts',(-1.42596018777283,1.,3.7996592319632));
#45318=CARTESIAN_POINT('Ctrl Pts',(-1.42076028482836,-1.,3.79400175744408));
#45319=CARTESIAN_POINT('Ctrl Pts',(-1.42076028482836,1.,3.79400175744408));
#45320=CARTESIAN_POINT('Ctrl Pts',(-1.4155952780383,-1.,3.78832489879426));
#45321=CARTESIAN_POINT('Ctrl Pts',(-1.4155952780383,1.,3.78832489879426));
#45322=CARTESIAN_POINT('Ctrl Pts',(-1.41046532282593,-1.,3.78262780065471));
#45323=CARTESIAN_POINT('Ctrl Pts',(-1.41046532282593,1.,3.78262780065471));
#45324=CARTESIAN_POINT('Ctrl Pts',(-1.40537056004722,-1.,3.77690952014259));
#45325=CARTESIAN_POINT('Ctrl Pts',(-1.40537056004722,1.,3.77690952014259));
#45326=CARTESIAN_POINT('Ctrl Pts',(-1.40031121335505,-1.,3.77116930621827));
#45327=CARTESIAN_POINT('Ctrl Pts',(-1.40031121335505,1.,3.77116930621827));
#45328=CARTESIAN_POINT('Ctrl Pts',(-1.39528769118052,-1.,3.76540689249074));
#45329=CARTESIAN_POINT('Ctrl Pts',(-1.39528769118052,1.,3.76540689249074));
#45330=CARTESIAN_POINT('Ctrl Pts',(-1.39030069388918,-1.,3.75962280650855));
#45331=CARTESIAN_POINT('Ctrl Pts',(-1.39030069388918,1.,3.75962280650855));
#45332=CARTESIAN_POINT('Ctrl Pts',(-1.38535129801176,-1.,3.75381861212707));
#45333=CARTESIAN_POINT('Ctrl Pts',(-1.38535129801176,1.,3.75381861212707));
#45334=CARTESIAN_POINT('Ctrl Pts',(-1.38044070763295,-1.,3.74799617204729));
#45335=CARTESIAN_POINT('Ctrl Pts',(-1.38044070763295,1.,3.74799617204729));
#45336=CARTESIAN_POINT('Ctrl Pts',(-1.37557002971687,-1.,3.74215698162555));
#45337=CARTESIAN_POINT('Ctrl Pts',(-1.37557002971687,1.,3.74215698162555));
#45338=CARTESIAN_POINT('Ctrl Pts',(-1.37074003422739,-1.,3.7363014588581));
#45339=CARTESIAN_POINT('Ctrl Pts',(-1.37074003422739,1.,3.7363014588581));
#45340=CARTESIAN_POINT('Ctrl Pts',(-1.36595093298676,-1.,3.73042829011295));
#45341=CARTESIAN_POINT('Ctrl Pts',(-1.36595093298676,1.,3.73042829011295));
#45342=CARTESIAN_POINT('Ctrl Pts',(-1.36120211416354,-1.,3.72453364678279));
#45343=CARTESIAN_POINT('Ctrl Pts',(-1.36120211416354,1.,3.72453364678279));
#45344=CARTESIAN_POINT('Ctrl Pts',(-1.35649266705037,-1.,3.71861271513313));
#45345=CARTESIAN_POINT('Ctrl Pts',(-1.35649266705037,1.,3.71861271513313));
#45346=CARTESIAN_POINT('Ctrl Pts',(-1.35182193384424,-1.,3.71266130563054));
#45347=CARTESIAN_POINT('Ctrl Pts',(-1.35182193384424,1.,3.71266130563054));
#45348=CARTESIAN_POINT('Ctrl Pts',(-1.34719008463534,-1.,3.70667753188248));
#45349=CARTESIAN_POINT('Ctrl Pts',(-1.34719008463534,1.,3.70667753188248));
#45350=CARTESIAN_POINT('Ctrl Pts',(-1.34259860752933,-1.,3.70066324015119));
#45351=CARTESIAN_POINT('Ctrl Pts',(-1.34259860752933,1.,3.70066324015119));
#45352=CARTESIAN_POINT('Ctrl Pts',(-1.3380510339822,-1.,3.69462613305708));
#45353=CARTESIAN_POINT('Ctrl Pts',(-1.3380510339822,1.,3.69462613305708));
#45354=CARTESIAN_POINT('Ctrl Pts',(-1.33355191034523,-1.,3.68857672413033));
#45355=CARTESIAN_POINT('Ctrl Pts',(-1.33355191034523,1.,3.68857672413033));
#45356=CARTESIAN_POINT('Ctrl Pts',(-1.3291054707274,-1.,3.68252441182551));
#45357=CARTESIAN_POINT('Ctrl Pts',(-1.3291054707274,1.,3.68252441182551));
#45358=CARTESIAN_POINT('Ctrl Pts',(-1.32471430856415,-1.,3.67647355257912));
#45359=CARTESIAN_POINT('Ctrl Pts',(-1.32471430856415,1.,3.67647355257912));
#45360=CARTESIAN_POINT('Ctrl Pts',(-1.32037828137766,-1.,3.67042021752656));
#45361=CARTESIAN_POINT('Ctrl Pts',(-1.32037828137766,1.,3.67042021752656));
#45362=CARTESIAN_POINT('Ctrl Pts',(-1.31609271239911,-1.,3.66434688899793));
#45363=CARTESIAN_POINT('Ctrl Pts',(-1.31609271239911,1.,3.66434688899793));
#45364=CARTESIAN_POINT('Ctrl Pts',(-1.31185038411218,-1.,3.65822827358617));
#45365=CARTESIAN_POINT('Ctrl Pts',(-1.31185038411218,1.,3.65822827358617));
#45366=CARTESIAN_POINT('Ctrl Pts',(-1.30764479590039,-1.,3.65204081987068));
#45367=CARTESIAN_POINT('Ctrl Pts',(-1.30764479590039,1.,3.65204081987068));
#45368=CARTESIAN_POINT('Ctrl Pts',(-1.30347327603774,-1.,3.64577181380113));
#45369=CARTESIAN_POINT('Ctrl Pts',(-1.30347327603774,1.,3.64577181380113));
#45370=CARTESIAN_POINT('Ctrl Pts',(-1.2993395590647,-1.,3.63942689872808));
#45371=CARTESIAN_POINT('Ctrl Pts',(-1.2993395590647,1.,3.63942689872808));
#45372=CARTESIAN_POINT('Ctrl Pts',(-1.29525810207762,-1.,3.63304271631046));
#45373=CARTESIAN_POINT('Ctrl Pts',(-1.29525810207762,1.,3.63304271631046));
#45374=CARTESIAN_POINT('Ctrl Pts',(-1.29125046021878,-1.,3.62667616004369));
#45375=CARTESIAN_POINT('Ctrl Pts',(-1.29125046021878,1.,3.62667616004369));
#45376=CARTESIAN_POINT('Ctrl Pts',(-1.28733755029384,-1.,3.6203814849236));
#45377=CARTESIAN_POINT('Ctrl Pts',(-1.28733755029384,1.,3.6203814849236));
#45378=CARTESIAN_POINT('Ctrl Pts',(-1.28353255117765,-1.,3.61418935913823));
#45379=CARTESIAN_POINT('Ctrl Pts',(-1.28353255117765,1.,3.61418935913823));
#45380=CARTESIAN_POINT('Ctrl Pts',(-1.27983492861691,-1.,3.60808907746339));
#45381=CARTESIAN_POINT('Ctrl Pts',(-1.27983492861691,1.,3.60808907746339));
#45382=CARTESIAN_POINT('Ctrl Pts',(-1.27622049908625,-1.,3.60199947736298));
#45383=CARTESIAN_POINT('Ctrl Pts',(-1.27622049908625,1.,3.60199947736298));
#45384=CARTESIAN_POINT('Ctrl Pts',(-1.27264798379307,-1.,3.59578698050006));
#45385=CARTESIAN_POINT('Ctrl Pts',(-1.27264798379307,1.,3.59578698050006));
#45386=CARTESIAN_POINT('Ctrl Pts',(-1.26907758484709,-1.,3.58931807846313));
#45387=CARTESIAN_POINT('Ctrl Pts',(-1.26907758484709,1.,3.58931807846313));
#45388=CARTESIAN_POINT('Ctrl Pts',(-1.26548706249862,-1.,3.58250452868618));
#45389=CARTESIAN_POINT('Ctrl Pts',(-1.26548706249862,1.,3.58250452868618));
#45390=CARTESIAN_POINT('Ctrl Pts',(-1.2618866714281,-1.,3.5753456065171));
#45391=CARTESIAN_POINT('Ctrl Pts',(-1.2618866714281,1.,3.5753456065171));
#45392=CARTESIAN_POINT('Ctrl Pts',(-1.25834000485716,-1.,3.56798645995275));
#45393=CARTESIAN_POINT('Ctrl Pts',(-1.25834000485716,1.,3.56798645995275));
#45394=CARTESIAN_POINT('Ctrl Pts',(-1.25496090900009,-1.,3.56071094991199));
#45395=CARTESIAN_POINT('Ctrl Pts',(-1.25496090900009,1.,3.56071094991199));
#45396=CARTESIAN_POINT('Ctrl Pts',(-1.2518879294064,-1.,3.55387287418985));
#45397=CARTESIAN_POINT('Ctrl Pts',(-1.2518879294064,1.,3.55387287418985));
#45398=CARTESIAN_POINT('Ctrl Pts',(-1.24926408628003,-1.,3.54784190283068));
#45399=CARTESIAN_POINT('Ctrl Pts',(-1.24926408628003,1.,3.54784190283068));
#45400=CARTESIAN_POINT('Ctrl Pts',(-1.24721646231966,-1.,3.54294877425964));
#45401=CARTESIAN_POINT('Ctrl Pts',(-1.24721646231966,1.,3.54294877425964));
#45402=CARTESIAN_POINT('Ctrl Pts',(-1.24583101679029,-1.,3.53941798195825));
#45403=CARTESIAN_POINT('Ctrl Pts',(-1.24583101679029,1.,3.53941798195825));
#45404=CARTESIAN_POINT('Ctrl Pts',(-1.24528461332987,-1.,3.53776753802906));
#45405=CARTESIAN_POINT('Ctrl Pts',(-1.24528461332987,1.,3.53776753802906));
#45406=CARTESIAN_POINT('Ctrl Pts',(-1.24519702335451,-1.,3.53720633057798));
#45407=CARTESIAN_POINT('Ctrl Pts',(-1.24519702335451,1.,3.53720633057798));
#45408=CARTESIAN_POINT('Ctrl Pts',(-1.24528174185098,-1.,3.53713269667399));
#45409=CARTESIAN_POINT('Ctrl Pts',(-1.24528174185098,1.,3.53713269667399));
#45410=CARTESIAN_POINT('Ctrl Pts',(-1.24535988127942,-1.,3.53717101171257));
#45411=CARTESIAN_POINT('Ctrl Pts',(-1.24535988127942,1.,3.53717101171257));
#45412=CARTESIAN_POINT('',(-1.53673442965256,1.,3.90876544355381));
#45413=CARTESIAN_POINT('Ctrl Pts',(-1.53673442965256,1.,3.90876544355381));
#45414=CARTESIAN_POINT('Ctrl Pts',(-1.53556639217905,1.,3.90771246855019));
#45415=CARTESIAN_POINT('Ctrl Pts',(-1.53323321827755,1.,3.90560462813969));
#45416=CARTESIAN_POINT('Ctrl Pts',(-1.52974216056287,1.,3.90243719631596));
#45417=CARTESIAN_POINT('Ctrl Pts',(-1.52510482991635,1.,3.89820260708225));
#45418=CARTESIAN_POINT('Ctrl Pts',(-1.51933724329306,1.,3.89289043533657));
#45419=CARTESIAN_POINT('Ctrl Pts',(-1.51359883110559,1.,3.88755930033884));
#45420=CARTESIAN_POINT('Ctrl Pts',(-1.50788973857757,1.,3.88220917950538));
#45421=CARTESIAN_POINT('Ctrl Pts',(-1.50221016176556,1.,3.87684006372134));
#45422=CARTESIAN_POINT('Ctrl Pts',(-1.49656035399122,1.,3.87145196998465));
#45423=CARTESIAN_POINT('Ctrl Pts',(-1.4909406116431,1.,3.86604492575189));
#45424=CARTESIAN_POINT('Ctrl Pts',(-1.48535125509919,1.,3.86061894706087));
#45425=CARTESIAN_POINT('Ctrl Pts',(-1.4797926099102,1.,3.85517401698843));
#45426=CARTESIAN_POINT('Ctrl Pts',(-1.47426499018538,1.,3.84971006847277));
#45427=CARTESIAN_POINT('Ctrl Pts',(-1.46876867426504,1.,3.84422695454796));
#45428=CARTESIAN_POINT('Ctrl Pts',(-1.46330391180752,1.,3.83872447159639));
#45429=CARTESIAN_POINT('Ctrl Pts',(-1.45787095220852,1.,3.83320241775423));
#45430=CARTESIAN_POINT('Ctrl Pts',(-1.45247006796836,1.,3.82766064519074));
#45431=CARTESIAN_POINT('Ctrl Pts',(-1.44710157648539,1.,3.82209910620533));
#45432=CARTESIAN_POINT('Ctrl Pts',(-1.44176587041347,1.,3.81651792398414));
#45433=CARTESIAN_POINT('Ctrl Pts',(-1.43646341556724,1.,3.81091737726815));
#45434=CARTESIAN_POINT('Ctrl Pts',(-1.4311946992132,1.,3.80529775429805));
#45435=CARTESIAN_POINT('Ctrl Pts',(-1.42596018777283,1.,3.7996592319632));
#45436=CARTESIAN_POINT('Ctrl Pts',(-1.42076028482836,1.,3.79400175744408));
#45437=CARTESIAN_POINT('Ctrl Pts',(-1.4155952780383,1.,3.78832489879426));
#45438=CARTESIAN_POINT('Ctrl Pts',(-1.41046532282593,1.,3.78262780065471));
#45439=CARTESIAN_POINT('Ctrl Pts',(-1.40537056004722,1.,3.77690952014259));
#45440=CARTESIAN_POINT('Ctrl Pts',(-1.40031121335505,1.,3.77116930621827));
#45441=CARTESIAN_POINT('Ctrl Pts',(-1.39528769118052,1.,3.76540689249074));
#45442=CARTESIAN_POINT('Ctrl Pts',(-1.39030069388918,1.,3.75962280650855));
#45443=CARTESIAN_POINT('Ctrl Pts',(-1.38535129801176,1.,3.75381861212707));
#45444=CARTESIAN_POINT('Ctrl Pts',(-1.38044070763295,1.,3.74799617204729));
#45445=CARTESIAN_POINT('Ctrl Pts',(-1.37557002971687,1.,3.74215698162555));
#45446=CARTESIAN_POINT('Ctrl Pts',(-1.37074003422739,1.,3.7363014588581));
#45447=CARTESIAN_POINT('Ctrl Pts',(-1.36595093298676,1.,3.73042829011295));
#45448=CARTESIAN_POINT('Ctrl Pts',(-1.36120211416354,1.,3.72453364678279));
#45449=CARTESIAN_POINT('Ctrl Pts',(-1.35649266705037,1.,3.71861271513313));
#45450=CARTESIAN_POINT('Ctrl Pts',(-1.35182193384424,1.,3.71266130563054));
#45451=CARTESIAN_POINT('Ctrl Pts',(-1.34719008463534,1.,3.70667753188248));
#45452=CARTESIAN_POINT('Ctrl Pts',(-1.34259860752933,1.,3.70066324015119));
#45453=CARTESIAN_POINT('Ctrl Pts',(-1.3380510339822,1.,3.69462613305708));
#45454=CARTESIAN_POINT('Ctrl Pts',(-1.33355191034523,1.,3.68857672413033));
#45455=CARTESIAN_POINT('Ctrl Pts',(-1.3291054707274,1.,3.68252441182551));
#45456=CARTESIAN_POINT('Ctrl Pts',(-1.32471430856415,1.,3.67647355257912));
#45457=CARTESIAN_POINT('Ctrl Pts',(-1.32037828137766,1.,3.67042021752656));
#45458=CARTESIAN_POINT('Ctrl Pts',(-1.31609271239911,1.,3.66434688899793));
#45459=CARTESIAN_POINT('Ctrl Pts',(-1.31185038411218,1.,3.65822827358617));
#45460=CARTESIAN_POINT('Ctrl Pts',(-1.30764479590039,1.,3.65204081987068));
#45461=CARTESIAN_POINT('Ctrl Pts',(-1.30347327603774,1.,3.64577181380113));
#45462=CARTESIAN_POINT('Ctrl Pts',(-1.2993395590647,1.,3.63942689872808));
#45463=CARTESIAN_POINT('Ctrl Pts',(-1.29525810207762,1.,3.63304271631046));
#45464=CARTESIAN_POINT('Ctrl Pts',(-1.29125046021878,1.,3.62667616004369));
#45465=CARTESIAN_POINT('Ctrl Pts',(-1.28733755029384,1.,3.6203814849236));
#45466=CARTESIAN_POINT('Ctrl Pts',(-1.28353255117765,1.,3.61418935913823));
#45467=CARTESIAN_POINT('Ctrl Pts',(-1.27983492861691,1.,3.60808907746339));
#45468=CARTESIAN_POINT('Ctrl Pts',(-1.27622049908625,1.,3.60199947736298));
#45469=CARTESIAN_POINT('Ctrl Pts',(-1.27264798379307,1.,3.59578698050006));
#45470=CARTESIAN_POINT('Ctrl Pts',(-1.26907758484709,1.,3.58931807846313));
#45471=CARTESIAN_POINT('Ctrl Pts',(-1.26548706249862,1.,3.58250452868618));
#45472=CARTESIAN_POINT('Ctrl Pts',(-1.2618866714281,1.,3.5753456065171));
#45473=CARTESIAN_POINT('Ctrl Pts',(-1.25834000485716,1.,3.56798645995275));
#45474=CARTESIAN_POINT('Ctrl Pts',(-1.25496090900009,1.,3.56071094991199));
#45475=CARTESIAN_POINT('Ctrl Pts',(-1.2518879294064,1.,3.55387287418985));
#45476=CARTESIAN_POINT('Ctrl Pts',(-1.24926408628003,1.,3.54784190283068));
#45477=CARTESIAN_POINT('Ctrl Pts',(-1.24721646231966,1.,3.54294877425964));
#45478=CARTESIAN_POINT('Ctrl Pts',(-1.24593497226008,1.,3.53968291130022));
#45479=CARTESIAN_POINT('Ctrl Pts',(-1.24539205388767,1.,3.53808746578196));
#45480=CARTESIAN_POINT('Ctrl Pts',(-1.2452449899111,1.,3.5374485926552));
#45481=CARTESIAN_POINT('Ctrl Pts',(-1.24524838931757,1.,3.53725139174486));
#45482=CARTESIAN_POINT('Ctrl Pts',(-1.24526366418038,1.,3.5372048861597));
#45483=CARTESIAN_POINT('',(-1.53673442965256,0.,3.90876544355381));
#45484=CARTESIAN_POINT('Ctrl Pts',(-1.62055519152809,-1.,3.38176002566879));
#45485=CARTESIAN_POINT('Ctrl Pts',(-1.62055519152809,1.,3.38176002566879));
#45486=CARTESIAN_POINT('Ctrl Pts',(-1.62058335162482,-1.,3.38167767992676));
#45487=CARTESIAN_POINT('Ctrl Pts',(-1.62058335162482,1.,3.38167767992676));
#45488=CARTESIAN_POINT('Ctrl Pts',(-1.62069532368199,-1.,3.38166984193836));
#45489=CARTESIAN_POINT('Ctrl Pts',(-1.62069532368199,1.,3.38166984193836));
#45490=CARTESIAN_POINT('Ctrl Pts',(-1.62103022181151,-1.,3.38212861099983));
#45491=CARTESIAN_POINT('Ctrl Pts',(-1.62103022181151,1.,3.38212861099983));
#45492=CARTESIAN_POINT('Ctrl Pts',(-1.62181089631344,-1.,3.38368201668574));
#45493=CARTESIAN_POINT('Ctrl Pts',(-1.62181089631344,1.,3.38368201668574));
#45494=CARTESIAN_POINT('Ctrl Pts',(-1.6233278855625,-1.,3.38715832179072));
#45495=CARTESIAN_POINT('Ctrl Pts',(-1.6233278855625,1.,3.38715832179072));
#45496=CARTESIAN_POINT('Ctrl Pts',(-1.62533996116713,-1.,3.39206617496906));
#45497=CARTESIAN_POINT('Ctrl Pts',(-1.62533996116713,1.,3.39206617496906));
#45498=CARTESIAN_POINT('Ctrl Pts',(-1.62774916464408,-1.,3.39818605297991));
#45499=CARTESIAN_POINT('Ctrl Pts',(-1.62774916464408,1.,3.39818605297991));
#45500=CARTESIAN_POINT('Ctrl Pts',(-1.63041148964828,-1.,3.40519422740235));
#45501=CARTESIAN_POINT('Ctrl Pts',(-1.63041148964828,1.,3.40519422740235));
#45502=CARTESIAN_POINT('Ctrl Pts',(-1.63316667054044,-1.,3.41272817148478));
#45503=CARTESIAN_POINT('Ctrl Pts',(-1.63316667054044,1.,3.41272817148478));
#45504=CARTESIAN_POINT('Ctrl Pts',(-1.63586250099773,-1.,3.42043974590882));
#45505=CARTESIAN_POINT('Ctrl Pts',(-1.63586250099773,1.,3.42043974590882));
#45506=CARTESIAN_POINT('Ctrl Pts',(-1.63837876246926,-1.,3.42804772926291));
#45507=CARTESIAN_POINT('Ctrl Pts',(-1.63837876246926,1.,3.42804772926291));
#45508=CARTESIAN_POINT('Ctrl Pts',(-1.64065778702023,-1.,3.43540451921548));
#45509=CARTESIAN_POINT('Ctrl Pts',(-1.64065778702023,1.,3.43540451921548));
#45510=CARTESIAN_POINT('Ctrl Pts',(-1.64270733821113,-1.,3.44250337701888));
#45511=CARTESIAN_POINT('Ctrl Pts',(-1.64270733821113,1.,3.44250337701888));
#45512=CARTESIAN_POINT('Ctrl Pts',(-1.64457408708107,-1.,3.44942242546795));
#45513=CARTESIAN_POINT('Ctrl Pts',(-1.64457408708107,1.,3.44942242546795));
#45514=CARTESIAN_POINT('Ctrl Pts',(-1.64632429697521,-1.,3.45628421062422));
#45515=CARTESIAN_POINT('Ctrl Pts',(-1.64632429697521,1.,3.45628421062422));
#45516=CARTESIAN_POINT('Ctrl Pts',(-1.64802323352738,-1.,3.46321237515));
#45517=CARTESIAN_POINT('Ctrl Pts',(-1.64802323352738,1.,3.46321237515));
#45518=CARTESIAN_POINT('Ctrl Pts',(-1.64971118698256,-1.,3.47028140995992));
#45519=CARTESIAN_POINT('Ctrl Pts',(-1.64971118698256,1.,3.47028140995992));
#45520=CARTESIAN_POINT('Ctrl Pts',(-1.65139534930322,-1.,3.47749926256476));
#45521=CARTESIAN_POINT('Ctrl Pts',(-1.65139534930322,1.,3.47749926256476));
#45522=CARTESIAN_POINT('Ctrl Pts',(-1.65306335367739,-1.,3.48483492840894));
#45523=CARTESIAN_POINT('Ctrl Pts',(-1.65306335367739,1.,3.48483492840894));
#45524=CARTESIAN_POINT('Ctrl Pts',(-1.65469162644468,-1.,3.49223525300176));
#45525=CARTESIAN_POINT('Ctrl Pts',(-1.65469162644468,1.,3.49223525300176));
#45526=CARTESIAN_POINT('Ctrl Pts',(-1.65625517961588,-1.,3.4996447647794));
#45527=CARTESIAN_POINT('Ctrl Pts',(-1.65625517961588,1.,3.4996447647794));
#45528=CARTESIAN_POINT('Ctrl Pts',(-1.65773832633632,-1.,3.50702733146542));
#45529=CARTESIAN_POINT('Ctrl Pts',(-1.65773832633632,1.,3.50702733146542));
#45530=CARTESIAN_POINT('Ctrl Pts',(-1.65913971687342,-1.,3.5143763218894));
#45531=CARTESIAN_POINT('Ctrl Pts',(-1.65913971687342,1.,3.5143763218894));
#45532=CARTESIAN_POINT('Ctrl Pts',(-1.66046645222279,-1.,3.52170261543815));
#45533=CARTESIAN_POINT('Ctrl Pts',(-1.66046645222279,1.,3.52170261543815));
#45534=CARTESIAN_POINT('Ctrl Pts',(-1.66173058912371,-1.,3.52902746211093));
#45535=CARTESIAN_POINT('Ctrl Pts',(-1.66173058912371,1.,3.52902746211093));
#45536=CARTESIAN_POINT('Ctrl Pts',(-1.66294490916111,-1.,3.5363738506022));
#45537=CARTESIAN_POINT('Ctrl Pts',(-1.66294490916111,1.,3.5363738506022));
#45538=CARTESIAN_POINT('Ctrl Pts',(-1.66411849222326,-1.,3.54375747475014));
#45539=CARTESIAN_POINT('Ctrl Pts',(-1.66411849222326,1.,3.54375747475014));
#45540=CARTESIAN_POINT('Ctrl Pts',(-1.66525401568994,-1.,3.55118121342861));
#45541=CARTESIAN_POINT('Ctrl Pts',(-1.66525401568994,1.,3.55118121342861));
#45542=CARTESIAN_POINT('Ctrl Pts',(-1.66635023293114,-1.,3.55864015233602));
#45543=CARTESIAN_POINT('Ctrl Pts',(-1.66635023293114,1.,3.55864015233602));
#45544=CARTESIAN_POINT('Ctrl Pts',(-1.66740349220305,-1.,3.56612465179422));
#45545=CARTESIAN_POINT('Ctrl Pts',(-1.66740349220305,1.,3.56612465179422));
#45546=CARTESIAN_POINT('Ctrl Pts',(-1.668409574073,-1.,3.57362406285887));
#45547=CARTESIAN_POINT('Ctrl Pts',(-1.668409574073,1.,3.57362406285887));
#45548=CARTESIAN_POINT('Ctrl Pts',(-1.66936552908232,-1.,3.58113044183829));
#45549=CARTESIAN_POINT('Ctrl Pts',(-1.66936552908232,1.,3.58113044183829));
#45550=CARTESIAN_POINT('Ctrl Pts',(-1.67027110397604,-1.,3.58864143097834));
#45551=CARTESIAN_POINT('Ctrl Pts',(-1.67027110397604,1.,3.58864143097834));
#45552=CARTESIAN_POINT('Ctrl Pts',(-1.67112775290707,-1.,3.59615824388807));
#45553=CARTESIAN_POINT('Ctrl Pts',(-1.67112775290707,1.,3.59615824388807));
#45554=CARTESIAN_POINT('Ctrl Pts',(-1.67193797318597,-1.,3.603684308152));
#45555=CARTESIAN_POINT('Ctrl Pts',(-1.67193797318597,1.,3.603684308152));
#45556=CARTESIAN_POINT('Ctrl Pts',(-1.67270452466968,-1.,3.61122367156181));
#45557=CARTESIAN_POINT('Ctrl Pts',(-1.67270452466968,1.,3.61122367156181));
#45558=CARTESIAN_POINT('Ctrl Pts',(-1.67342968196224,-1.,3.61877947398184));
#45559=CARTESIAN_POINT('Ctrl Pts',(-1.67342968196224,1.,3.61877947398184));
#45560=CARTESIAN_POINT('Ctrl Pts',(-1.67411452372271,-1.,3.62635249450923));
#45561=CARTESIAN_POINT('Ctrl Pts',(-1.67411452372271,1.,3.62635249450923));
#45562=CARTESIAN_POINT('Ctrl Pts',(-1.67475929882971,-1.,3.63394189312924));
#45563=CARTESIAN_POINT('Ctrl Pts',(-1.67475929882971,1.,3.63394189312924));
#45564=CARTESIAN_POINT('Ctrl Pts',(-1.67536373264848,-1.,3.6415458297234));
#45565=CARTESIAN_POINT('Ctrl Pts',(-1.67536373264848,1.,3.6415458297234));
#45566=CARTESIAN_POINT('Ctrl Pts',(-1.67592735946692,-1.,3.64916213574667));
#45567=CARTESIAN_POINT('Ctrl Pts',(-1.67592735946692,1.,3.64916213574667));
#45568=CARTESIAN_POINT('Ctrl Pts',(-1.6764498346945,-1.,3.6567889441642));
#45569=CARTESIAN_POINT('Ctrl Pts',(-1.6764498346945,1.,3.6567889441642));
#45570=CARTESIAN_POINT('Ctrl Pts',(-1.67693128053132,-1.,3.66442538670968));
#45571=CARTESIAN_POINT('Ctrl Pts',(-1.67693128053132,1.,3.66442538670968));
#45572=CARTESIAN_POINT('Ctrl Pts',(-1.67737217414874,-1.,3.67207136294575));
#45573=CARTESIAN_POINT('Ctrl Pts',(-1.67737217414874,1.,3.67207136294575));
#45574=CARTESIAN_POINT('Ctrl Pts',(-1.67777320475848,-1.,3.67972724579124));
#45575=CARTESIAN_POINT('Ctrl Pts',(-1.67777320475848,1.,3.67972724579124));
#45576=CARTESIAN_POINT('Ctrl Pts',(-1.67813513867965,-1.,3.68739360236487));
#45577=CARTESIAN_POINT('Ctrl Pts',(-1.67813513867965,1.,3.68739360236487));
#45578=CARTESIAN_POINT('Ctrl Pts',(-1.67845869064323,-1.,3.6950709275959));
#45579=CARTESIAN_POINT('Ctrl Pts',(-1.67845869064323,1.,3.6950709275959));
#45580=CARTESIAN_POINT('Ctrl Pts',(-1.67874436948667,-1.,3.70275932351108));
#45581=CARTESIAN_POINT('Ctrl Pts',(-1.67874436948667,1.,3.70275932351108));
#45582=CARTESIAN_POINT('Ctrl Pts',(-1.67899249793462,-1.,3.71045854208343));
#45583=CARTESIAN_POINT('Ctrl Pts',(-1.67899249793462,1.,3.71045854208343));
#45584=CARTESIAN_POINT('Ctrl Pts',(-1.67920328071708,-1.,3.71816812842322));
#45585=CARTESIAN_POINT('Ctrl Pts',(-1.67920328071708,1.,3.71816812842322));
#45586=CARTESIAN_POINT('Ctrl Pts',(-1.67937685856652,-1.,3.72588753416396));
#45587=CARTESIAN_POINT('Ctrl Pts',(-1.67937685856652,1.,3.72588753416396));
#45588=CARTESIAN_POINT('Ctrl Pts',(-1.67951336376402,-1.,3.73361623282543));
#45589=CARTESIAN_POINT('Ctrl Pts',(-1.67951336376402,1.,3.73361623282543));
#45590=CARTESIAN_POINT('Ctrl Pts',(-1.6796129868522,-1.,3.74135385965401));
#45591=CARTESIAN_POINT('Ctrl Pts',(-1.6796129868522,1.,3.74135385965401));
#45592=CARTESIAN_POINT('Ctrl Pts',(-1.67967598599525,-1.,3.7491002239452));
#45593=CARTESIAN_POINT('Ctrl Pts',(-1.67967598599525,1.,3.7491002239452));
#45594=CARTESIAN_POINT('Ctrl Pts',(-1.67970265841239,-1.,3.75685523754493));
#45595=CARTESIAN_POINT('Ctrl Pts',(-1.67970265841239,1.,3.75685523754493));
#45596=CARTESIAN_POINT('Ctrl Pts',(-1.67969332319245,-1.,3.76461886684344));
#45597=CARTESIAN_POINT('Ctrl Pts',(-1.67969332319245,1.,3.76461886684344));
#45598=CARTESIAN_POINT('Ctrl Pts',(-1.67964830084993,-1.,3.77239107928502));
#45599=CARTESIAN_POINT('Ctrl Pts',(-1.67964830084993,1.,3.77239107928502));
#45600=CARTESIAN_POINT('Ctrl Pts',(-1.67956789212141,-1.,3.78017178197317));
#45601=CARTESIAN_POINT('Ctrl Pts',(-1.67956789212141,1.,3.78017178197317));
#45602=CARTESIAN_POINT('Ctrl Pts',(-1.67945236653493,-1.,3.7879608002176));
#45603=CARTESIAN_POINT('Ctrl Pts',(-1.67945236653493,1.,3.7879608002176));
#45604=CARTESIAN_POINT('Ctrl Pts',(-1.67930196625548,-1.,3.79575791578424));
#45605=CARTESIAN_POINT('Ctrl Pts',(-1.67930196625548,1.,3.79575791578424));
#45606=CARTESIAN_POINT('Ctrl Pts',(-1.67911690648355,-1.,3.80356289079005));
#45607=CARTESIAN_POINT('Ctrl Pts',(-1.67911690648355,1.,3.80356289079005));
#45608=CARTESIAN_POINT('Ctrl Pts',(-1.6788973773827,-1.,3.81137549624178));
#45609=CARTESIAN_POINT('Ctrl Pts',(-1.6788973773827,1.,3.81137549624178));
#45610=CARTESIAN_POINT('Ctrl Pts',(-1.67864354605954,-1.,3.81919554099578));
#45611=CARTESIAN_POINT('Ctrl Pts',(-1.67864354605954,1.,3.81919554099578));
#45612=CARTESIAN_POINT('Ctrl Pts',(-1.6783555575934,-1.,3.82702289286713));
#45613=CARTESIAN_POINT('Ctrl Pts',(-1.6783555575934,1.,3.82702289286713));
#45614=CARTESIAN_POINT('Ctrl Pts',(-1.67803353064351,-1.,3.83485746513989));
#45615=CARTESIAN_POINT('Ctrl Pts',(-1.67803353064351,1.,3.83485746513989));
#45616=CARTESIAN_POINT('Ctrl Pts',(-1.67774874946079,-1.,3.84113085985244));
#45617=CARTESIAN_POINT('Ctrl Pts',(-1.67774874946079,1.,3.84113085985244));
#45618=CARTESIAN_POINT('Ctrl Pts',(-1.6775199114018,-1.,3.84583912296459));
#45619=CARTESIAN_POINT('Ctrl Pts',(-1.6775199114018,1.,3.84583912296459));
#45620=CARTESIAN_POINT('Ctrl Pts',(-1.67736057656533,-1.,3.84897939430696));
#45621=CARTESIAN_POINT('Ctrl Pts',(-1.67736057656533,1.,3.84897939430696));
#45622=CARTESIAN_POINT('Ctrl Pts',(-1.67727921511438,-1.,3.85054988729471));
#45623=CARTESIAN_POINT('Ctrl Pts',(-1.67727921511438,1.,3.85054988729471));
#45624=CARTESIAN_POINT('',(-1.62064718014094,1.,3.38171594275765));
#45625=CARTESIAN_POINT('Ctrl Pts',(-1.62064718014094,-1.,3.38171594275765));
#45626=CARTESIAN_POINT('Ctrl Pts',(-1.62064718014094,-0.666666666666667,
3.38171594275765));
#45627=CARTESIAN_POINT('Ctrl Pts',(-1.62064718014094,-0.333333333333333,
3.38171594275765));
#45628=CARTESIAN_POINT('Ctrl Pts',(-1.62064718014094,0.333333333333333,
3.38171594275765));
#45629=CARTESIAN_POINT('Ctrl Pts',(-1.62064718014094,0.666666666666667,
3.38171594275765));
#45630=CARTESIAN_POINT('Ctrl Pts',(-1.62064718014094,1.,3.38171594275765));
#45631=CARTESIAN_POINT('',(-1.67727921511438,1.,3.85054988729471));
#45632=CARTESIAN_POINT('',(-1.67727921511438,0.,3.85054988729471));
#45633=CARTESIAN_POINT('Ctrl Pts',(-1.62064718014094,1.,3.38171594275765));
#45634=CARTESIAN_POINT('Ctrl Pts',(-1.62069086551492,1.,3.38173802621259));
#45635=CARTESIAN_POINT('Ctrl Pts',(-1.62083271135947,1.,3.38187506456922));
#45636=CARTESIAN_POINT('Ctrl Pts',(-1.62118047294498,1.,3.38243080602408));
#45637=CARTESIAN_POINT('Ctrl Pts',(-1.62192472202769,1.,3.38394285763222));
#45638=CARTESIAN_POINT('Ctrl Pts',(-1.6233278855625,1.,3.38715832179072));
#45639=CARTESIAN_POINT('Ctrl Pts',(-1.62533996116713,1.,3.39206617496906));
#45640=CARTESIAN_POINT('Ctrl Pts',(-1.62774916464408,1.,3.39818605297991));
#45641=CARTESIAN_POINT('Ctrl Pts',(-1.63041148964828,1.,3.40519422740235));
#45642=CARTESIAN_POINT('Ctrl Pts',(-1.63316667054044,1.,3.41272817148478));
#45643=CARTESIAN_POINT('Ctrl Pts',(-1.63586250099773,1.,3.42043974590882));
#45644=CARTESIAN_POINT('Ctrl Pts',(-1.63837876246926,1.,3.42804772926291));
#45645=CARTESIAN_POINT('Ctrl Pts',(-1.64065778702023,1.,3.43540451921548));
#45646=CARTESIAN_POINT('Ctrl Pts',(-1.64270733821113,1.,3.44250337701888));
#45647=CARTESIAN_POINT('Ctrl Pts',(-1.64457408708107,1.,3.44942242546795));
#45648=CARTESIAN_POINT('Ctrl Pts',(-1.64632429697521,1.,3.45628421062422));
#45649=CARTESIAN_POINT('Ctrl Pts',(-1.64802323352738,1.,3.46321237515));
#45650=CARTESIAN_POINT('Ctrl Pts',(-1.64971118698256,1.,3.47028140995992));
#45651=CARTESIAN_POINT('Ctrl Pts',(-1.65139534930322,1.,3.47749926256476));
#45652=CARTESIAN_POINT('Ctrl Pts',(-1.65306335367739,1.,3.48483492840894));
#45653=CARTESIAN_POINT('Ctrl Pts',(-1.65469162644468,1.,3.49223525300176));
#45654=CARTESIAN_POINT('Ctrl Pts',(-1.65625517961588,1.,3.4996447647794));
#45655=CARTESIAN_POINT('Ctrl Pts',(-1.65773832633632,1.,3.50702733146542));
#45656=CARTESIAN_POINT('Ctrl Pts',(-1.65913971687342,1.,3.5143763218894));
#45657=CARTESIAN_POINT('Ctrl Pts',(-1.66046645222279,1.,3.52170261543815));
#45658=CARTESIAN_POINT('Ctrl Pts',(-1.66173058912371,1.,3.52902746211093));
#45659=CARTESIAN_POINT('Ctrl Pts',(-1.66294490916111,1.,3.5363738506022));
#45660=CARTESIAN_POINT('Ctrl Pts',(-1.66411849222326,1.,3.54375747475014));
#45661=CARTESIAN_POINT('Ctrl Pts',(-1.66525401568994,1.,3.55118121342861));
#45662=CARTESIAN_POINT('Ctrl Pts',(-1.66635023293114,1.,3.55864015233602));
#45663=CARTESIAN_POINT('Ctrl Pts',(-1.66740349220305,1.,3.56612465179422));
#45664=CARTESIAN_POINT('Ctrl Pts',(-1.668409574073,1.,3.57362406285887));
#45665=CARTESIAN_POINT('Ctrl Pts',(-1.66936552908232,1.,3.58113044183829));
#45666=CARTESIAN_POINT('Ctrl Pts',(-1.67027110397604,1.,3.58864143097834));
#45667=CARTESIAN_POINT('Ctrl Pts',(-1.67112775290707,1.,3.59615824388807));
#45668=CARTESIAN_POINT('Ctrl Pts',(-1.67193797318597,1.,3.603684308152));
#45669=CARTESIAN_POINT('Ctrl Pts',(-1.67270452466968,1.,3.61122367156181));
#45670=CARTESIAN_POINT('Ctrl Pts',(-1.67342968196224,1.,3.61877947398184));
#45671=CARTESIAN_POINT('Ctrl Pts',(-1.67411452372271,1.,3.62635249450923));
#45672=CARTESIAN_POINT('Ctrl Pts',(-1.67475929882971,1.,3.63394189312924));
#45673=CARTESIAN_POINT('Ctrl Pts',(-1.67536373264848,1.,3.6415458297234));
#45674=CARTESIAN_POINT('Ctrl Pts',(-1.67592735946692,1.,3.64916213574667));
#45675=CARTESIAN_POINT('Ctrl Pts',(-1.6764498346945,1.,3.6567889441642));
#45676=CARTESIAN_POINT('Ctrl Pts',(-1.67693128053132,1.,3.66442538670968));
#45677=CARTESIAN_POINT('Ctrl Pts',(-1.67737217414874,1.,3.67207136294575));
#45678=CARTESIAN_POINT('Ctrl Pts',(-1.67777320475848,1.,3.67972724579124));
#45679=CARTESIAN_POINT('Ctrl Pts',(-1.67813513867965,1.,3.68739360236487));
#45680=CARTESIAN_POINT('Ctrl Pts',(-1.67845869064323,1.,3.6950709275959));
#45681=CARTESIAN_POINT('Ctrl Pts',(-1.67874436948667,1.,3.70275932351108));
#45682=CARTESIAN_POINT('Ctrl Pts',(-1.67899249793462,1.,3.71045854208343));
#45683=CARTESIAN_POINT('Ctrl Pts',(-1.67920328071708,1.,3.71816812842322));
#45684=CARTESIAN_POINT('Ctrl Pts',(-1.67937685856652,1.,3.72588753416396));
#45685=CARTESIAN_POINT('Ctrl Pts',(-1.67951336376402,1.,3.73361623282543));
#45686=CARTESIAN_POINT('Ctrl Pts',(-1.6796129868522,1.,3.74135385965401));
#45687=CARTESIAN_POINT('Ctrl Pts',(-1.67967598599525,1.,3.7491002239452));
#45688=CARTESIAN_POINT('Ctrl Pts',(-1.67970265841239,1.,3.75685523754493));
#45689=CARTESIAN_POINT('Ctrl Pts',(-1.67969332319245,1.,3.76461886684344));
#45690=CARTESIAN_POINT('Ctrl Pts',(-1.67964830084993,1.,3.77239107928502));
#45691=CARTESIAN_POINT('Ctrl Pts',(-1.67956789212141,1.,3.78017178197317));
#45692=CARTESIAN_POINT('Ctrl Pts',(-1.67945236653493,1.,3.7879608002176));
#45693=CARTESIAN_POINT('Ctrl Pts',(-1.67930196625548,1.,3.79575791578424));
#45694=CARTESIAN_POINT('Ctrl Pts',(-1.67911690648355,1.,3.80356289079005));
#45695=CARTESIAN_POINT('Ctrl Pts',(-1.6788973773827,1.,3.81137549624178));
#45696=CARTESIAN_POINT('Ctrl Pts',(-1.67864354605954,1.,3.81919554099578));
#45697=CARTESIAN_POINT('Ctrl Pts',(-1.6783555575934,1.,3.82702289286713));
#45698=CARTESIAN_POINT('Ctrl Pts',(-1.67803353064351,1.,3.83485746513989));
#45699=CARTESIAN_POINT('Ctrl Pts',(-1.67774874946079,1.,3.84113085985244));
#45700=CARTESIAN_POINT('Ctrl Pts',(-1.6775199114018,1.,3.84583912296459));
#45701=CARTESIAN_POINT('Ctrl Pts',(-1.67736057656533,1.,3.84897939430696));
#45702=CARTESIAN_POINT('Ctrl Pts',(-1.67727921511438,1.,3.85054988729471));
#45703=CARTESIAN_POINT('Origin',(-1.67727921511438,0.,3.85054988729471));
#45704=CARTESIAN_POINT('',(-1.53673442965256,1.,3.90876544355381));
#45705=CARTESIAN_POINT('Origin',(0.,0.,0.));
#45706=CARTESIAN_POINT('',(-1.78327315618183,1.,3.29885386921599));
#45707=CARTESIAN_POINT('Origin',(0.,1.,0.));
#45708=CARTESIAN_POINT('Ctrl Pts',(-1.78327315618183,1.,3.29885386921599));
#45709=CARTESIAN_POINT('Ctrl Pts',(-1.78327315618183,0.666666666666667,
3.29885386921599));
#45710=CARTESIAN_POINT('Ctrl Pts',(-1.78327315618183,0.333333333333333,
3.29885386921599));
#45711=CARTESIAN_POINT('Ctrl Pts',(-1.78327315618183,-0.333333333333333,
3.29885386921599));
#45712=CARTESIAN_POINT('Ctrl Pts',(-1.78327315618183,-0.666666666666667,
3.29885386921599));
#45713=CARTESIAN_POINT('Ctrl Pts',(-1.78327315618183,-1.,3.29885386921599));
#45714=CARTESIAN_POINT('Ctrl Pts',(-2.12928030988903,-1.,3.62024382630768));
#45715=CARTESIAN_POINT('Ctrl Pts',(-2.12928030988903,1.,3.62024382630768));
#45716=CARTESIAN_POINT('Ctrl Pts',(-2.12796193131368,-1.,3.61938653649098));
#45717=CARTESIAN_POINT('Ctrl Pts',(-2.12796193131368,1.,3.61938653649098));
#45718=CARTESIAN_POINT('Ctrl Pts',(-2.12532774376758,-1.,3.61766963590482));
#45719=CARTESIAN_POINT('Ctrl Pts',(-2.12532774376758,1.,3.61766963590482));
#45720=CARTESIAN_POINT('Ctrl Pts',(-2.12138417126355,-1.,3.61508732216891));
#45721=CARTESIAN_POINT('Ctrl Pts',(-2.12138417126355,1.,3.61508732216891));
#45722=CARTESIAN_POINT('Ctrl Pts',(-2.11614149815106,-1.,3.61163030609447));
#45723=CARTESIAN_POINT('Ctrl Pts',(-2.11614149815106,1.,3.61163030609447));
#45724=CARTESIAN_POINT('Ctrl Pts',(-2.10961391334462,-1.,3.60728578532601));
#45725=CARTESIAN_POINT('Ctrl Pts',(-2.10961391334462,1.,3.60728578532601));
#45726=CARTESIAN_POINT('Ctrl Pts',(-2.1031121772821,-1.,3.60291797088734));
#45727=CARTESIAN_POINT('Ctrl Pts',(-2.1031121772821,1.,3.60291797088734));
#45728=CARTESIAN_POINT('Ctrl Pts',(-2.09663642986631,-1.,3.59852681775485));
#45729=CARTESIAN_POINT('Ctrl Pts',(-2.09663642986631,1.,3.59852681775485));
#45730=CARTESIAN_POINT('Ctrl Pts',(-2.09018686331416,-1.,3.59411228625588));
#45731=CARTESIAN_POINT('Ctrl Pts',(-2.09018686331416,1.,3.59411228625588));
#45732=CARTESIAN_POINT('Ctrl Pts',(-2.08376373048756,-1.,3.58967435355088));
#45733=CARTESIAN_POINT('Ctrl Pts',(-2.08376373048756,1.,3.58967435355088));
#45734=CARTESIAN_POINT('Ctrl Pts',(-2.07736732842117,-1.,3.58521300039299));
#45735=CARTESIAN_POINT('Ctrl Pts',(-2.07736732842117,1.,3.58521300039299));
#45736=CARTESIAN_POINT('Ctrl Pts',(-2.07099797605747,-1.,3.58072819250442));
#45737=CARTESIAN_POINT('Ctrl Pts',(-2.07099797605747,1.,3.58072819250442));
#45738=CARTESIAN_POINT('Ctrl Pts',(-2.06465599229174,-1.,3.576219862243));
#45739=CARTESIAN_POINT('Ctrl Pts',(-2.06465599229174,1.,3.576219862243));
#45740=CARTESIAN_POINT('Ctrl Pts',(-2.05834167687523,-1.,3.57168789423507));
#45741=CARTESIAN_POINT('Ctrl Pts',(-2.05834167687523,1.,3.57168789423507));
#45742=CARTESIAN_POINT('Ctrl Pts',(-2.0520552817309,-1.,3.56713209978207));
#45743=CARTESIAN_POINT('Ctrl Pts',(-2.0520552817309,1.,3.56713209978207));
#45744=CARTESIAN_POINT('Ctrl Pts',(-2.04579702159056,-1.,3.5625522387181));
#45745=CARTESIAN_POINT('Ctrl Pts',(-2.04579702159056,1.,3.5625522387181));
#45746=CARTESIAN_POINT('Ctrl Pts',(-2.03956711120099,-1.,3.55794807265052));
#45747=CARTESIAN_POINT('Ctrl Pts',(-2.03956711120099,1.,3.55794807265052));
#45748=CARTESIAN_POINT('Ctrl Pts',(-2.03336579658174,-1.,3.55331941294018));
#45749=CARTESIAN_POINT('Ctrl Pts',(-2.03336579658174,1.,3.55331941294018));
#45750=CARTESIAN_POINT('Ctrl Pts',(-2.02719338376144,-1.,3.54866616282173));
#45751=CARTESIAN_POINT('Ctrl Pts',(-2.02719338376144,1.,3.54866616282173));
#45752=CARTESIAN_POINT('Ctrl Pts',(-2.0210502798303,-1.,3.54398838254011));
#45753=CARTESIAN_POINT('Ctrl Pts',(-2.0210502798303,1.,3.54398838254011));
#45754=CARTESIAN_POINT('Ctrl Pts',(-2.0149369884727,-1.,3.53928627453503));
#45755=CARTESIAN_POINT('Ctrl Pts',(-2.0149369884727,1.,3.53928627453503));
#45756=CARTESIAN_POINT('Ctrl Pts',(-2.00885403604685,-1.,3.53456004727321));
#45757=CARTESIAN_POINT('Ctrl Pts',(-2.00885403604685,1.,3.53456004727321));
#45758=CARTESIAN_POINT('Ctrl Pts',(-2.00280191090341,-1.,3.52980980250181));
#45759=CARTESIAN_POINT('Ctrl Pts',(-2.00280191090341,1.,3.52980980250181));
#45760=CARTESIAN_POINT('Ctrl Pts',(-1.99678100339305,-1.,3.52503542491745));
#45761=CARTESIAN_POINT('Ctrl Pts',(-1.99678100339305,1.,3.52503542491745));
#45762=CARTESIAN_POINT('Ctrl Pts',(-1.99079153006143,-1.,3.52023644289195));
#45763=CARTESIAN_POINT('Ctrl Pts',(-1.99079153006143,1.,3.52023644289195));
#45764=CARTESIAN_POINT('Ctrl Pts',(-1.98483351061066,-1.,3.51541198728362));
#45765=CARTESIAN_POINT('Ctrl Pts',(-1.98483351061066,1.,3.51541198728362));
#45766=CARTESIAN_POINT('Ctrl Pts',(-1.97890693666316,-1.,3.51056110478334));
#45767=CARTESIAN_POINT('Ctrl Pts',(-1.97890693666316,1.,3.51056110478334));
#45768=CARTESIAN_POINT('Ctrl Pts',(-1.9730119116298,-1.,3.505683018611));
#45769=CARTESIAN_POINT('Ctrl Pts',(-1.9730119116298,1.,3.505683018611));
#45770=CARTESIAN_POINT('Ctrl Pts',(-1.9671487972405,-1.,3.50077740176262));
#45771=CARTESIAN_POINT('Ctrl Pts',(-1.9671487972405,1.,3.50077740176262));
#45772=CARTESIAN_POINT('Ctrl Pts',(-1.96131836776489,-1.,3.49584466573045));
#45773=CARTESIAN_POINT('Ctrl Pts',(-1.96131836776489,1.,3.49584466573045));
#45774=CARTESIAN_POINT('Ctrl Pts',(-1.95552193112071,-1.,3.49088618670967));
#45775=CARTESIAN_POINT('Ctrl Pts',(-1.95552193112071,1.,3.49088618670967));
#45776=CARTESIAN_POINT('Ctrl Pts',(-1.94976096795902,-1.,3.485903616108));
#45777=CARTESIAN_POINT('Ctrl Pts',(-1.94976096795902,1.,3.485903616108));
#45778=CARTESIAN_POINT('Ctrl Pts',(-1.94403680554062,-1.,3.48089825770411));
#45779=CARTESIAN_POINT('Ctrl Pts',(-1.94403680554062,1.,3.48089825770411));
#45780=CARTESIAN_POINT('Ctrl Pts',(-1.93835026973888,-1.,3.47587040389916));
#45781=CARTESIAN_POINT('Ctrl Pts',(-1.93835026973888,1.,3.47587040389916));
#45782=CARTESIAN_POINT('Ctrl Pts',(-1.93270136427083,-1.,3.47081872409783));
#45783=CARTESIAN_POINT('Ctrl Pts',(-1.93270136427083,1.,3.47081872409783));
#45784=CARTESIAN_POINT('Ctrl Pts',(-1.92708888591159,-1.,3.46573953254084));
#45785=CARTESIAN_POINT('Ctrl Pts',(-1.92708888591159,1.,3.46573953254084));
#45786=CARTESIAN_POINT('Ctrl Pts',(-1.9215111821321,-1.,3.4606282172248));
#45787=CARTESIAN_POINT('Ctrl Pts',(-1.9215111821321,1.,3.4606282172248));
#45788=CARTESIAN_POINT('Ctrl Pts',(-1.9159669478406,-1.,3.45548074309943));
#45789=CARTESIAN_POINT('Ctrl Pts',(-1.9159669478406,1.,3.45548074309943));
#45790=CARTESIAN_POINT('Ctrl Pts',(-1.91045605593638,-1.,3.45029522038885));
#45791=CARTESIAN_POINT('Ctrl Pts',(-1.91045605593638,1.,3.45029522038885));
#45792=CARTESIAN_POINT('Ctrl Pts',(-1.90498026502308,-1.,3.44507323983374));
#45793=CARTESIAN_POINT('Ctrl Pts',(-1.90498026502308,1.,3.44507323983374));
#45794=CARTESIAN_POINT('Ctrl Pts',(-1.89954426803392,-1.,3.43982185678105));
#45795=CARTESIAN_POINT('Ctrl Pts',(-1.89954426803392,1.,3.43982185678105));
#45796=CARTESIAN_POINT('Ctrl Pts',(-1.89415420002553,-1.,3.43455074411591));
#45797=CARTESIAN_POINT('Ctrl Pts',(-1.89415420002553,1.,3.43455074411591));
#45798=CARTESIAN_POINT('Ctrl Pts',(-1.88881571322018,-1.,3.42926852222174));
#45799=CARTESIAN_POINT('Ctrl Pts',(-1.88881571322018,1.,3.42926852222174));
#45800=CARTESIAN_POINT('Ctrl Pts',(-1.88353205062063,-1.,3.42397908819741));
#45801=CARTESIAN_POINT('Ctrl Pts',(-1.88353205062063,1.,3.42397908819741));
#45802=CARTESIAN_POINT('Ctrl Pts',(-1.87830245689338,-1.,3.4186785838376));
#45803=CARTESIAN_POINT('Ctrl Pts',(-1.87830245689338,1.,3.4186785838376));
#45804=CARTESIAN_POINT('Ctrl Pts',(-1.87311957248106,-1.,3.41335043875182));
#45805=CARTESIAN_POINT('Ctrl Pts',(-1.87311957248106,1.,3.41335043875182));
#45806=CARTESIAN_POINT('Ctrl Pts',(-1.86797231196635,-1.,3.40797080000513));
#45807=CARTESIAN_POINT('Ctrl Pts',(-1.86797231196635,1.,3.40797080000513));
#45808=CARTESIAN_POINT('Ctrl Pts',(-1.86285057051228,-1.,3.40251742305445));
#45809=CARTESIAN_POINT('Ctrl Pts',(-1.86285057051228,1.,3.40251742305445));
#45810=CARTESIAN_POINT('Ctrl Pts',(-1.85774972037055,-1.,3.39697816833056));
#45811=CARTESIAN_POINT('Ctrl Pts',(-1.85774972037055,1.,3.39697816833056));
#45812=CARTESIAN_POINT('Ctrl Pts',(-1.85267433291778,-1.,3.39135802549415));
#45813=CARTESIAN_POINT('Ctrl Pts',(-1.85267433291778,1.,3.39135802549415));
#45814=CARTESIAN_POINT('Ctrl Pts',(-1.84764441927778,-1.,3.38569092349639));
#45815=CARTESIAN_POINT('Ctrl Pts',(-1.84764441927778,1.,3.38569092349639));
#45816=CARTESIAN_POINT('Ctrl Pts',(-1.84269016931679,-1.,3.38002968341222));
#45817=CARTESIAN_POINT('Ctrl Pts',(-1.84269016931679,1.,3.38002968341222));
#45818=CARTESIAN_POINT('Ctrl Pts',(-1.83784072967111,-1.,3.37442462015914));
#45819=CARTESIAN_POINT('Ctrl Pts',(-1.83784072967111,1.,3.37442462015914));
#45820=CARTESIAN_POINT('Ctrl Pts',(-1.83311391452338,-1.,3.36890396271864));
#45821=CARTESIAN_POINT('Ctrl Pts',(-1.83311391452338,1.,3.36890396271864));
#45822=CARTESIAN_POINT('Ctrl Pts',(-1.82850752153182,-1.,3.36345722124127));
#45823=CARTESIAN_POINT('Ctrl Pts',(-1.82850752153182,1.,3.36345722124127));
#45824=CARTESIAN_POINT('Ctrl Pts',(-1.82398496829247,-1.,3.35800801557326));
#45825=CARTESIAN_POINT('Ctrl Pts',(-1.82398496829247,1.,3.35800801557326));
#45826=CARTESIAN_POINT('Ctrl Pts',(-1.81948458796748,-1.,3.35243086937451));
#45827=CARTESIAN_POINT('Ctrl Pts',(-1.81948458796748,1.,3.35243086937451));
#45828=CARTESIAN_POINT('Ctrl Pts',(-1.81494618732772,-1.,3.34660014370527));
#45829=CARTESIAN_POINT('Ctrl Pts',(-1.81494618732772,1.,3.34660014370527));
#45830=CARTESIAN_POINT('Ctrl Pts',(-1.81033399625311,-1.,3.34043216147532));
#45831=CARTESIAN_POINT('Ctrl Pts',(-1.81033399625311,1.,3.34043216147532));
#45832=CARTESIAN_POINT('Ctrl Pts',(-1.80565802981138,-1.,3.33392460276874));
#45833=CARTESIAN_POINT('Ctrl Pts',(-1.80565802981138,1.,3.33392460276874));
#45834=CARTESIAN_POINT('Ctrl Pts',(-1.80100380443535,-1.,3.3272108803981));
#45835=CARTESIAN_POINT('Ctrl Pts',(-1.80100380443535,1.,3.3272108803981));
#45836=CARTESIAN_POINT('Ctrl Pts',(-1.79652817033444,-1.,3.32055355101168));
#45837=CARTESIAN_POINT('Ctrl Pts',(-1.79652817033444,1.,3.32055355101168));
#45838=CARTESIAN_POINT('Ctrl Pts',(-1.79242331350137,-1.,3.31428038326763));
#45839=CARTESIAN_POINT('Ctrl Pts',(-1.79242331350137,1.,3.31428038326763));
#45840=CARTESIAN_POINT('Ctrl Pts',(-1.78888832245965,-1.,3.30873412266954));
#45841=CARTESIAN_POINT('Ctrl Pts',(-1.78888832245965,1.,3.30873412266954));
#45842=CARTESIAN_POINT('Ctrl Pts',(-1.78610045419769,-1.,3.30422155558973));
#45843=CARTESIAN_POINT('Ctrl Pts',(-1.78610045419769,1.,3.30422155558973));
#45844=CARTESIAN_POINT('Ctrl Pts',(-1.78417972819696,-1.,3.30095096463082));
#45845=CARTESIAN_POINT('Ctrl Pts',(-1.78417972819696,1.,3.30095096463082));
#45846=CARTESIAN_POINT('Ctrl Pts',(-1.78338186555671,-1.,3.29940631673818));
#45847=CARTESIAN_POINT('Ctrl Pts',(-1.78338186555671,1.,3.29940631673818));
#45848=CARTESIAN_POINT('Ctrl Pts',(-1.78320756177191,-1.,3.29886572077303));
#45849=CARTESIAN_POINT('Ctrl Pts',(-1.78320756177191,1.,3.29886572077303));
#45850=CARTESIAN_POINT('Ctrl Pts',(-1.78327971836272,-1.,3.29877974053191));
#45851=CARTESIAN_POINT('Ctrl Pts',(-1.78327971836272,1.,3.29877974053191));
#45852=CARTESIAN_POINT('Ctrl Pts',(-1.7833628895577,-1.,3.2988053601491));
#45853=CARTESIAN_POINT('Ctrl Pts',(-1.7833628895577,1.,3.2988053601491));
#45854=CARTESIAN_POINT('',(-2.12928030988903,1.,3.62024382630768));
#45855=CARTESIAN_POINT('Ctrl Pts',(-2.12928030988903,1.,3.62024382630768));
#45856=CARTESIAN_POINT('Ctrl Pts',(-2.12796193131368,1.,3.61938653649098));
#45857=CARTESIAN_POINT('Ctrl Pts',(-2.12532774376758,1.,3.61766963590482));
#45858=CARTESIAN_POINT('Ctrl Pts',(-2.12138417126355,1.,3.61508732216891));
#45859=CARTESIAN_POINT('Ctrl Pts',(-2.11614149815106,1.,3.61163030609447));
#45860=CARTESIAN_POINT('Ctrl Pts',(-2.10961391334462,1.,3.60728578532601));
#45861=CARTESIAN_POINT('Ctrl Pts',(-2.1031121772821,1.,3.60291797088734));
#45862=CARTESIAN_POINT('Ctrl Pts',(-2.09663642986631,1.,3.59852681775485));
#45863=CARTESIAN_POINT('Ctrl Pts',(-2.09018686331416,1.,3.59411228625588));
#45864=CARTESIAN_POINT('Ctrl Pts',(-2.08376373048756,1.,3.58967435355088));
#45865=CARTESIAN_POINT('Ctrl Pts',(-2.07736732842117,1.,3.58521300039299));
#45866=CARTESIAN_POINT('Ctrl Pts',(-2.07099797605747,1.,3.58072819250442));
#45867=CARTESIAN_POINT('Ctrl Pts',(-2.06465599229174,1.,3.576219862243));
#45868=CARTESIAN_POINT('Ctrl Pts',(-2.05834167687523,1.,3.57168789423507));
#45869=CARTESIAN_POINT('Ctrl Pts',(-2.0520552817309,1.,3.56713209978207));
#45870=CARTESIAN_POINT('Ctrl Pts',(-2.04579702159056,1.,3.5625522387181));
#45871=CARTESIAN_POINT('Ctrl Pts',(-2.03956711120099,1.,3.55794807265052));
#45872=CARTESIAN_POINT('Ctrl Pts',(-2.03336579658174,1.,3.55331941294018));
#45873=CARTESIAN_POINT('Ctrl Pts',(-2.02719338376144,1.,3.54866616282173));
#45874=CARTESIAN_POINT('Ctrl Pts',(-2.0210502798303,1.,3.54398838254011));
#45875=CARTESIAN_POINT('Ctrl Pts',(-2.0149369884727,1.,3.53928627453503));
#45876=CARTESIAN_POINT('Ctrl Pts',(-2.00885403604685,1.,3.53456004727321));
#45877=CARTESIAN_POINT('Ctrl Pts',(-2.00280191090341,1.,3.52980980250181));
#45878=CARTESIAN_POINT('Ctrl Pts',(-1.99678100339305,1.,3.52503542491745));
#45879=CARTESIAN_POINT('Ctrl Pts',(-1.99079153006143,1.,3.52023644289195));
#45880=CARTESIAN_POINT('Ctrl Pts',(-1.98483351061066,1.,3.51541198728362));
#45881=CARTESIAN_POINT('Ctrl Pts',(-1.97890693666316,1.,3.51056110478334));
#45882=CARTESIAN_POINT('Ctrl Pts',(-1.9730119116298,1.,3.505683018611));
#45883=CARTESIAN_POINT('Ctrl Pts',(-1.9671487972405,1.,3.50077740176262));
#45884=CARTESIAN_POINT('Ctrl Pts',(-1.96131836776489,1.,3.49584466573045));
#45885=CARTESIAN_POINT('Ctrl Pts',(-1.95552193112071,1.,3.49088618670967));
#45886=CARTESIAN_POINT('Ctrl Pts',(-1.94976096795902,1.,3.485903616108));
#45887=CARTESIAN_POINT('Ctrl Pts',(-1.94403680554062,1.,3.48089825770411));
#45888=CARTESIAN_POINT('Ctrl Pts',(-1.93835026973888,1.,3.47587040389916));
#45889=CARTESIAN_POINT('Ctrl Pts',(-1.93270136427083,1.,3.47081872409783));
#45890=CARTESIAN_POINT('Ctrl Pts',(-1.92708888591159,1.,3.46573953254084));
#45891=CARTESIAN_POINT('Ctrl Pts',(-1.9215111821321,1.,3.4606282172248));
#45892=CARTESIAN_POINT('Ctrl Pts',(-1.9159669478406,1.,3.45548074309943));
#45893=CARTESIAN_POINT('Ctrl Pts',(-1.91045605593638,1.,3.45029522038885));
#45894=CARTESIAN_POINT('Ctrl Pts',(-1.90498026502308,1.,3.44507323983374));
#45895=CARTESIAN_POINT('Ctrl Pts',(-1.89954426803392,1.,3.43982185678105));
#45896=CARTESIAN_POINT('Ctrl Pts',(-1.89415420002553,1.,3.43455074411591));
#45897=CARTESIAN_POINT('Ctrl Pts',(-1.88881571322018,1.,3.42926852222174));
#45898=CARTESIAN_POINT('Ctrl Pts',(-1.88353205062063,1.,3.42397908819741));
#45899=CARTESIAN_POINT('Ctrl Pts',(-1.87830245689338,1.,3.4186785838376));
#45900=CARTESIAN_POINT('Ctrl Pts',(-1.87311957248106,1.,3.41335043875182));
#45901=CARTESIAN_POINT('Ctrl Pts',(-1.86797231196635,1.,3.40797080000513));
#45902=CARTESIAN_POINT('Ctrl Pts',(-1.86285057051228,1.,3.40251742305445));
#45903=CARTESIAN_POINT('Ctrl Pts',(-1.85774972037055,1.,3.39697816833056));
#45904=CARTESIAN_POINT('Ctrl Pts',(-1.85267433291778,1.,3.39135802549415));
#45905=CARTESIAN_POINT('Ctrl Pts',(-1.84764441927778,1.,3.38569092349639));
#45906=CARTESIAN_POINT('Ctrl Pts',(-1.84269016931679,1.,3.38002968341222));
#45907=CARTESIAN_POINT('Ctrl Pts',(-1.83784072967111,1.,3.37442462015914));
#45908=CARTESIAN_POINT('Ctrl Pts',(-1.83311391452338,1.,3.36890396271864));
#45909=CARTESIAN_POINT('Ctrl Pts',(-1.82850752153182,1.,3.36345722124127));
#45910=CARTESIAN_POINT('Ctrl Pts',(-1.82398496829247,1.,3.35800801557326));
#45911=CARTESIAN_POINT('Ctrl Pts',(-1.81948458796748,1.,3.35243086937451));
#45912=CARTESIAN_POINT('Ctrl Pts',(-1.81494618732772,1.,3.34660014370527));
#45913=CARTESIAN_POINT('Ctrl Pts',(-1.81033399625311,1.,3.34043216147532));
#45914=CARTESIAN_POINT('Ctrl Pts',(-1.80565802981138,1.,3.33392460276874));
#45915=CARTESIAN_POINT('Ctrl Pts',(-1.80100380443535,1.,3.3272108803981));
#45916=CARTESIAN_POINT('Ctrl Pts',(-1.79652817033444,1.,3.32055355101168));
#45917=CARTESIAN_POINT('Ctrl Pts',(-1.79242331350137,1.,3.31428038326763));
#45918=CARTESIAN_POINT('Ctrl Pts',(-1.78888832245965,1.,3.30873412266954));
#45919=CARTESIAN_POINT('Ctrl Pts',(-1.78610045419769,1.,3.30422155558973));
#45920=CARTESIAN_POINT('Ctrl Pts',(-1.7843238478823,1.,3.30119637003466));
#45921=CARTESIAN_POINT('Ctrl Pts',(-1.78353803106983,1.,3.29970549824337));
#45922=CARTESIAN_POINT('Ctrl Pts',(-1.78329283591903,1.,3.29909749657945));
#45923=CARTESIAN_POINT('Ctrl Pts',(-1.78326534445426,1.,3.29890219175522));
#45924=CARTESIAN_POINT('Ctrl Pts',(-1.78327315618183,1.,3.29885386921599));
#45925=CARTESIAN_POINT('',(-2.12928030988903,0.,3.62024382630768));
#45926=CARTESIAN_POINT('Ctrl Pts',(-2.12962728847315,-1.,3.08661426358891));
#45927=CARTESIAN_POINT('Ctrl Pts',(-2.12962728847315,1.,3.08661426358891));
#45928=CARTESIAN_POINT('Ctrl Pts',(-2.12964222016025,-1.,3.08652852644995));
#45929=CARTESIAN_POINT('Ctrl Pts',(-2.12964222016025,1.,3.08652852644995));
#45930=CARTESIAN_POINT('Ctrl Pts',(-2.12975158752407,-1.,3.08650326867133));
#45931=CARTESIAN_POINT('Ctrl Pts',(-2.12975158752407,1.,3.08650326867133));
#45932=CARTESIAN_POINT('Ctrl Pts',(-2.1301541297946,-1.,3.08690399991463));
#45933=CARTESIAN_POINT('Ctrl Pts',(-2.1301541297946,1.,3.08690399991463));
#45934=CARTESIAN_POINT('Ctrl Pts',(-2.13116819908542,-1.,3.08831615620074));
#45935=CARTESIAN_POINT('Ctrl Pts',(-2.13116819908542,1.,3.08831615620074));
#45936=CARTESIAN_POINT('Ctrl Pts',(-2.13321032560893,-1.,3.09151235281963));
#45937=CARTESIAN_POINT('Ctrl Pts',(-2.13321032560893,1.,3.09151235281963));
#45938=CARTESIAN_POINT('Ctrl Pts',(-2.13596538661048,-1.,3.0960450242104));
#45939=CARTESIAN_POINT('Ctrl Pts',(-2.13596538661048,1.,3.0960450242104));
#45940=CARTESIAN_POINT('Ctrl Pts',(-2.13930228863751,-1.,3.10171267391049));
#45941=CARTESIAN_POINT('Ctrl Pts',(-2.13930228863751,1.,3.10171267391049));
#45942=CARTESIAN_POINT('Ctrl Pts',(-2.14302815601973,-1.,3.10821808668859));
#45943=CARTESIAN_POINT('Ctrl Pts',(-2.14302815601973,1.,3.10821808668859));
#45944=CARTESIAN_POINT('Ctrl Pts',(-2.14692798457532,-1.,3.11522827016855));
#45945=CARTESIAN_POINT('Ctrl Pts',(-2.14692798457532,1.,3.11522827016855));
#45946=CARTESIAN_POINT('Ctrl Pts',(-2.15079698090585,-1.,3.12242318151938));
#45947=CARTESIAN_POINT('Ctrl Pts',(-2.15079698090585,1.,3.12242318151938));
#45948=CARTESIAN_POINT('Ctrl Pts',(-2.1544724138292,-1.,3.12954386795646));
#45949=CARTESIAN_POINT('Ctrl Pts',(-2.1544724138292,1.,3.12954386795646));
#45950=CARTESIAN_POINT('Ctrl Pts',(-2.15787423530676,-1.,3.13645356563038));
#45951=CARTESIAN_POINT('Ctrl Pts',(-2.15787423530676,1.,3.13645356563038));
#45952=CARTESIAN_POINT('Ctrl Pts',(-2.16100905914435,-1.,3.14314440427022));
#45953=CARTESIAN_POINT('Ctrl Pts',(-2.16100905914435,1.,3.14314440427022));
#45954=CARTESIAN_POINT('Ctrl Pts',(-2.16393520288072,-1.,3.14968624389054));
#45955=CARTESIAN_POINT('Ctrl Pts',(-2.16393520288072,1.,3.14968624389054));
#45956=CARTESIAN_POINT('Ctrl Pts',(-2.1667372844769,-1.,3.15618975593656));
#45957=CARTESIAN_POINT('Ctrl Pts',(-2.1667372844769,1.,3.15618975593656));
#45958=CARTESIAN_POINT('Ctrl Pts',(-2.16949910801219,-1.,3.16276685102972));
#45959=CARTESIAN_POINT('Ctrl Pts',(-2.16949910801219,1.,3.16276685102972));
#45960=CARTESIAN_POINT('Ctrl Pts',(-2.17227212063817,-1.,3.16948480019497));
#45961=CARTESIAN_POINT('Ctrl Pts',(-2.17227212063817,1.,3.16948480019497));
#45962=CARTESIAN_POINT('Ctrl Pts',(-2.17506466903694,-1.,3.17635032802523));
#45963=CARTESIAN_POINT('Ctrl Pts',(-2.17506466903694,1.,3.17635032802523));
#45964=CARTESIAN_POINT('Ctrl Pts',(-2.17785968847142,-1.,3.18333474627807));
#45965=CARTESIAN_POINT('Ctrl Pts',(-2.17785968847142,1.,3.18333474627807));
#45966=CARTESIAN_POINT('Ctrl Pts',(-2.18062558031778,-1.,3.19038924261573));
#45967=CARTESIAN_POINT('Ctrl Pts',(-2.18062558031778,1.,3.19038924261573));
#45968=CARTESIAN_POINT('Ctrl Pts',(-2.18332898656602,-1.,3.19746293740411));
#45969=CARTESIAN_POINT('Ctrl Pts',(-2.18332898656602,1.,3.19746293740411));
#45970=CARTESIAN_POINT('Ctrl Pts',(-2.18594876115934,-1.,3.20452259717976));
#45971=CARTESIAN_POINT('Ctrl Pts',(-2.18594876115934,1.,3.20452259717976));
#45972=CARTESIAN_POINT('Ctrl Pts',(-2.18848253363901,-1.,3.21156188355769));
#45973=CARTESIAN_POINT('Ctrl Pts',(-2.18848253363901,1.,3.21156188355769));
#45974=CARTESIAN_POINT('Ctrl Pts',(-2.19093901948667,-1.,3.21859043114095));
#45975=CARTESIAN_POINT('Ctrl Pts',(-2.19093901948667,1.,3.21859043114095));
#45976=CARTESIAN_POINT('Ctrl Pts',(-2.19333345123538,-1.,3.22562734221646));
#45977=CARTESIAN_POINT('Ctrl Pts',(-2.19333345123538,1.,3.22562734221646));
#45978=CARTESIAN_POINT('Ctrl Pts',(-2.19568204933168,-1.,3.23269332296933));
#45979=CARTESIAN_POINT('Ctrl Pts',(-2.19568204933168,1.,3.23269332296933));
#45980=CARTESIAN_POINT('Ctrl Pts',(-2.19799623693253,-1.,3.23980245361308));
#45981=CARTESIAN_POINT('Ctrl Pts',(-2.19799623693253,1.,3.23980245361308));
#45982=CARTESIAN_POINT('Ctrl Pts',(-2.20027910880981,-1.,3.24695715874338));
#45983=CARTESIAN_POINT('Ctrl Pts',(-2.20027910880981,1.,3.24695715874338));
#45984=CARTESIAN_POINT('Ctrl Pts',(-2.20252866491545,-1.,3.25415277957775));
#45985=CARTESIAN_POINT('Ctrl Pts',(-2.20252866491545,1.,3.25415277957775));
#45986=CARTESIAN_POINT('Ctrl Pts',(-2.20473979048678,-1.,3.26138036637705));
#45987=CARTESIAN_POINT('Ctrl Pts',(-2.20473979048678,1.,3.26138036637705));
#45988=CARTESIAN_POINT('Ctrl Pts',(-2.20690665217743,-1.,3.26863006136782));
#45989=CARTESIAN_POINT('Ctrl Pts',(-2.20690665217743,1.,3.26863006136782));
#45990=CARTESIAN_POINT('Ctrl Pts',(-2.2090250941743,-1.,3.2758944800554));
#45991=CARTESIAN_POINT('Ctrl Pts',(-2.2090250941743,1.,3.2758944800554));
#45992=CARTESIAN_POINT('Ctrl Pts',(-2.21109449750641,-1.,3.28317133333131));
#45993=CARTESIAN_POINT('Ctrl Pts',(-2.21109449750641,1.,3.28317133333131));
#45994=CARTESIAN_POINT('Ctrl Pts',(-2.21311648827391,-1.,3.29046159238343));
#45995=CARTESIAN_POINT('Ctrl Pts',(-2.21311648827391,1.,3.29046159238343));
#45996=CARTESIAN_POINT('Ctrl Pts',(-2.21509406923368,-1.,3.29776825193159));
#45997=CARTESIAN_POINT('Ctrl Pts',(-2.21509406923368,1.,3.29776825193159));
#45998=CARTESIAN_POINT('Ctrl Pts',(-2.21703059947836,-1.,3.30509487819569));
#45999=CARTESIAN_POINT('Ctrl Pts',(-2.21703059947836,1.,3.30509487819569));
#46000=CARTESIAN_POINT('Ctrl Pts',(-2.21892881679086,-1.,3.31244421655666));
#46001=CARTESIAN_POINT('Ctrl Pts',(-2.21892881679086,1.,3.31244421655666));
#46002=CARTESIAN_POINT('Ctrl Pts',(-2.22078990842776,-1.,3.31981686778022));
#46003=CARTESIAN_POINT('Ctrl Pts',(-2.22078990842776,1.,3.31981686778022));
#46004=CARTESIAN_POINT('Ctrl Pts',(-2.22261398879635,-1.,3.3272119632604));
#46005=CARTESIAN_POINT('Ctrl Pts',(-2.22261398879635,1.,3.3272119632604));
#46006=CARTESIAN_POINT('Ctrl Pts',(-2.22440049878511,-1.,3.33462772849598));
#46007=CARTESIAN_POINT('Ctrl Pts',(-2.22440049878511,1.,3.33462772849598));
#46008=CARTESIAN_POINT('Ctrl Pts',(-2.22614863918047,-1.,3.34206209449375));
#46009=CARTESIAN_POINT('Ctrl Pts',(-2.22614863918047,1.,3.34206209449375));
#46010=CARTESIAN_POINT('Ctrl Pts',(-2.22785777756576,-1.,3.34951327111096));
#46011=CARTESIAN_POINT('Ctrl Pts',(-2.22785777756576,1.,3.34951327111096));
#46012=CARTESIAN_POINT('Ctrl Pts',(-2.22952789880982,-1.,3.35698038165483));
#46013=CARTESIAN_POINT('Ctrl Pts',(-2.22952789880982,1.,3.35698038165483));
#46014=CARTESIAN_POINT('Ctrl Pts',(-2.23115945849739,-1.,3.36446325227848));
#46015=CARTESIAN_POINT('Ctrl Pts',(-2.23115945849739,1.,3.36446325227848));
#46016=CARTESIAN_POINT('Ctrl Pts',(-2.23275319569221,-1.,3.37196214349304));
#46017=CARTESIAN_POINT('Ctrl Pts',(-2.23275319569221,1.,3.37196214349304));
#46018=CARTESIAN_POINT('Ctrl Pts',(-2.23430995599561,-1.,3.37947749555632));
#46019=CARTESIAN_POINT('Ctrl Pts',(-2.23430995599561,1.,3.37947749555632));
#46020=CARTESIAN_POINT('Ctrl Pts',(-2.23583052276308,-1.,3.38700968549563));
#46021=CARTESIAN_POINT('Ctrl Pts',(-2.23583052276308,1.,3.38700968549563));
#46022=CARTESIAN_POINT('Ctrl Pts',(-2.23731541452791,-1.,3.39455873448189));
#46023=CARTESIAN_POINT('Ctrl Pts',(-2.23731541452791,1.,3.39455873448189));
#46024=CARTESIAN_POINT('Ctrl Pts',(-2.2387649112415,-1.,3.40212434705647));
#46025=CARTESIAN_POINT('Ctrl Pts',(-2.2387649112415,1.,3.40212434705647));
#46026=CARTESIAN_POINT('Ctrl Pts',(-2.24017914395289,-1.,3.40970604190328));
#46027=CARTESIAN_POINT('Ctrl Pts',(-2.24017914395289,1.,3.40970604190328));
#46028=CARTESIAN_POINT('Ctrl Pts',(-2.24155816587844,-1.,3.41730325539172));
#46029=CARTESIAN_POINT('Ctrl Pts',(-2.24155816587844,1.,3.41730325539172));
#46030=CARTESIAN_POINT('Ctrl Pts',(-2.24290202531101,-1.,3.42491544683008));
#46031=CARTESIAN_POINT('Ctrl Pts',(-2.24290202531101,1.,3.42491544683008));
#46032=CARTESIAN_POINT('Ctrl Pts',(-2.24421085338727,-1.,3.43254222614803));
#46033=CARTESIAN_POINT('Ctrl Pts',(-2.24421085338727,1.,3.43254222614803));
#46034=CARTESIAN_POINT('Ctrl Pts',(-2.24548487526022,-1.,3.4401833646032));
#46035=CARTESIAN_POINT('Ctrl Pts',(-2.24548487526022,1.,3.4401833646032));
#46036=CARTESIAN_POINT('Ctrl Pts',(-2.2467243706995,-1.,3.44783872863151));
#46037=CARTESIAN_POINT('Ctrl Pts',(-2.2467243706995,1.,3.44783872863151));
#46038=CARTESIAN_POINT('Ctrl Pts',(-2.2479296496077,-1.,3.45550823512049));
#46039=CARTESIAN_POINT('Ctrl Pts',(-2.2479296496077,1.,3.45550823512049));
#46040=CARTESIAN_POINT('Ctrl Pts',(-2.2491010234604,-1.,3.46319180177573));
#46041=CARTESIAN_POINT('Ctrl Pts',(-2.2491010234604,1.,3.46319180177573));
#46042=CARTESIAN_POINT('Ctrl Pts',(-2.25023877475942,-1.,3.47088928979888));
#46043=CARTESIAN_POINT('Ctrl Pts',(-2.25023877475942,1.,3.47088928979888));
#46044=CARTESIAN_POINT('Ctrl Pts',(-2.25134314238687,-1.,3.47860048448691));
#46045=CARTESIAN_POINT('Ctrl Pts',(-2.25134314238687,1.,3.47860048448691));
#46046=CARTESIAN_POINT('Ctrl Pts',(-2.25241433138695,-1.,3.48632513240961));
#46047=CARTESIAN_POINT('Ctrl Pts',(-2.25241433138695,1.,3.48632513240961));
#46048=CARTESIAN_POINT('Ctrl Pts',(-2.2534525170976,-1.,3.49406296494791));
#46049=CARTESIAN_POINT('Ctrl Pts',(-2.2534525170976,1.,3.49406296494791));
#46050=CARTESIAN_POINT('Ctrl Pts',(-2.25445785151868,-1.,3.50181372617971));
#46051=CARTESIAN_POINT('Ctrl Pts',(-2.25445785151868,1.,3.50181372617971));
#46052=CARTESIAN_POINT('Ctrl Pts',(-2.25543046979799,-1.,3.50957720117341));
#46053=CARTESIAN_POINT('Ctrl Pts',(-2.25543046979799,1.,3.50957720117341));
#46054=CARTESIAN_POINT('Ctrl Pts',(-2.25637049455044,-1.,3.51735323667612));
#46055=CARTESIAN_POINT('Ctrl Pts',(-2.25637049455044,1.,3.51735323667612));
#46056=CARTESIAN_POINT('Ctrl Pts',(-2.25727802940898,-1.,3.52514172847711));
#46057=CARTESIAN_POINT('Ctrl Pts',(-2.25727802940898,1.,3.52514172847711));
#46058=CARTESIAN_POINT('Ctrl Pts',(-2.25797812950104,-1.,3.53138243688262));
#46059=CARTESIAN_POINT('Ctrl Pts',(-2.25797812950104,1.,3.53138243688262));
#46060=CARTESIAN_POINT('Ctrl Pts',(-2.25848864343951,-1.,3.53606853162228));
#46061=CARTESIAN_POINT('Ctrl Pts',(-2.25848864343951,1.,3.53606853162228));
#46062=CARTESIAN_POINT('Ctrl Pts',(-2.2588225169468,-1.,3.53919506647335));
#46063=CARTESIAN_POINT('Ctrl Pts',(-2.2588225169468,1.,3.53919506647335));
#46064=CARTESIAN_POINT('Ctrl Pts',(-2.25898783642071,-1.,3.54075895182139));
#46065=CARTESIAN_POINT('Ctrl Pts',(-2.25898783642071,1.,3.54075895182139));
#46066=CARTESIAN_POINT('',(-2.1297112484669,1.,3.08655633322212));
#46067=CARTESIAN_POINT('Ctrl Pts',(-2.1297112484669,-1.,3.08655633322212));
#46068=CARTESIAN_POINT('Ctrl Pts',(-2.1297112484669,-0.666666666666667,
3.08655633322212));
#46069=CARTESIAN_POINT('Ctrl Pts',(-2.1297112484669,-0.333333333333333,
3.08655633322212));
#46070=CARTESIAN_POINT('Ctrl Pts',(-2.1297112484669,0.333333333333333,3.08655633322212));
#46071=CARTESIAN_POINT('Ctrl Pts',(-2.1297112484669,0.666666666666667,3.08655633322212));
#46072=CARTESIAN_POINT('Ctrl Pts',(-2.1297112484669,1.,3.08655633322212));
#46073=CARTESIAN_POINT('',(-2.25898783642071,1.,3.54075895182139));
#46074=CARTESIAN_POINT('',(-2.25898783642071,0.,3.54075895182139));
#46075=CARTESIAN_POINT('Ctrl Pts',(-2.1297112484669,1.,3.08655633322211));
#46076=CARTESIAN_POINT('Ctrl Pts',(-2.1297578506149,1.,3.08657131089497));
#46077=CARTESIAN_POINT('Ctrl Pts',(-2.12991938762374,1.,3.08668447250322));
#46078=CARTESIAN_POINT('Ctrl Pts',(-2.13034980480424,1.,3.08717896996098));
#46079=CARTESIAN_POINT('Ctrl Pts',(-2.13132142793017,1.,3.08855597949761));
#46080=CARTESIAN_POINT('Ctrl Pts',(-2.13321032560893,1.,3.09151235281963));
#46081=CARTESIAN_POINT('Ctrl Pts',(-2.13596538661048,1.,3.0960450242104));
#46082=CARTESIAN_POINT('Ctrl Pts',(-2.13930228863751,1.,3.10171267391049));
#46083=CARTESIAN_POINT('Ctrl Pts',(-2.14302815601973,1.,3.10821808668859));
#46084=CARTESIAN_POINT('Ctrl Pts',(-2.14692798457532,1.,3.11522827016855));
#46085=CARTESIAN_POINT('Ctrl Pts',(-2.15079698090585,1.,3.12242318151938));
#46086=CARTESIAN_POINT('Ctrl Pts',(-2.1544724138292,1.,3.12954386795646));
#46087=CARTESIAN_POINT('Ctrl Pts',(-2.15787423530676,1.,3.13645356563038));
#46088=CARTESIAN_POINT('Ctrl Pts',(-2.16100905914435,1.,3.14314440427022));
#46089=CARTESIAN_POINT('Ctrl Pts',(-2.16393520288072,1.,3.14968624389054));
#46090=CARTESIAN_POINT('Ctrl Pts',(-2.1667372844769,1.,3.15618975593656));
#46091=CARTESIAN_POINT('Ctrl Pts',(-2.16949910801219,1.,3.16276685102972));
#46092=CARTESIAN_POINT('Ctrl Pts',(-2.17227212063817,1.,3.16948480019497));
#46093=CARTESIAN_POINT('Ctrl Pts',(-2.17506466903694,1.,3.17635032802523));
#46094=CARTESIAN_POINT('Ctrl Pts',(-2.17785968847142,1.,3.18333474627807));
#46095=CARTESIAN_POINT('Ctrl Pts',(-2.18062558031778,1.,3.19038924261573));
#46096=CARTESIAN_POINT('Ctrl Pts',(-2.18332898656602,1.,3.19746293740411));
#46097=CARTESIAN_POINT('Ctrl Pts',(-2.18594876115934,1.,3.20452259717976));
#46098=CARTESIAN_POINT('Ctrl Pts',(-2.18848253363901,1.,3.21156188355769));
#46099=CARTESIAN_POINT('Ctrl Pts',(-2.19093901948667,1.,3.21859043114095));
#46100=CARTESIAN_POINT('Ctrl Pts',(-2.19333345123538,1.,3.22562734221646));
#46101=CARTESIAN_POINT('Ctrl Pts',(-2.19568204933168,1.,3.23269332296933));
#46102=CARTESIAN_POINT('Ctrl Pts',(-2.19799623693253,1.,3.23980245361308));
#46103=CARTESIAN_POINT('Ctrl Pts',(-2.20027910880981,1.,3.24695715874338));
#46104=CARTESIAN_POINT('Ctrl Pts',(-2.20252866491545,1.,3.25415277957775));
#46105=CARTESIAN_POINT('Ctrl Pts',(-2.20473979048678,1.,3.26138036637705));
#46106=CARTESIAN_POINT('Ctrl Pts',(-2.20690665217743,1.,3.26863006136782));
#46107=CARTESIAN_POINT('Ctrl Pts',(-2.2090250941743,1.,3.2758944800554));
#46108=CARTESIAN_POINT('Ctrl Pts',(-2.21109449750641,1.,3.28317133333131));
#46109=CARTESIAN_POINT('Ctrl Pts',(-2.21311648827391,1.,3.29046159238343));
#46110=CARTESIAN_POINT('Ctrl Pts',(-2.21509406923368,1.,3.29776825193159));
#46111=CARTESIAN_POINT('Ctrl Pts',(-2.21703059947836,1.,3.30509487819569));
#46112=CARTESIAN_POINT('Ctrl Pts',(-2.21892881679086,1.,3.31244421655666));
#46113=CARTESIAN_POINT('Ctrl Pts',(-2.22078990842776,1.,3.31981686778022));
#46114=CARTESIAN_POINT('Ctrl Pts',(-2.22261398879635,1.,3.3272119632604));
#46115=CARTESIAN_POINT('Ctrl Pts',(-2.22440049878511,1.,3.33462772849598));
#46116=CARTESIAN_POINT('Ctrl Pts',(-2.22614863918047,1.,3.34206209449375));
#46117=CARTESIAN_POINT('Ctrl Pts',(-2.22785777756576,1.,3.34951327111096));
#46118=CARTESIAN_POINT('Ctrl Pts',(-2.22952789880982,1.,3.35698038165483));
#46119=CARTESIAN_POINT('Ctrl Pts',(-2.23115945849739,1.,3.36446325227848));
#46120=CARTESIAN_POINT('Ctrl Pts',(-2.23275319569221,1.,3.37196214349304));
#46121=CARTESIAN_POINT('Ctrl Pts',(-2.23430995599561,1.,3.37947749555632));
#46122=CARTESIAN_POINT('Ctrl Pts',(-2.23583052276308,1.,3.38700968549563));
#46123=CARTESIAN_POINT('Ctrl Pts',(-2.23731541452791,1.,3.39455873448189));
#46124=CARTESIAN_POINT('Ctrl Pts',(-2.2387649112415,1.,3.40212434705647));
#46125=CARTESIAN_POINT('Ctrl Pts',(-2.24017914395289,1.,3.40970604190328));
#46126=CARTESIAN_POINT('Ctrl Pts',(-2.24155816587844,1.,3.41730325539172));
#46127=CARTESIAN_POINT('Ctrl Pts',(-2.24290202531101,1.,3.42491544683008));
#46128=CARTESIAN_POINT('Ctrl Pts',(-2.24421085338727,1.,3.43254222614803));
#46129=CARTESIAN_POINT('Ctrl Pts',(-2.24548487526022,1.,3.4401833646032));
#46130=CARTESIAN_POINT('Ctrl Pts',(-2.2467243706995,1.,3.44783872863151));
#46131=CARTESIAN_POINT('Ctrl Pts',(-2.2479296496077,1.,3.45550823512049));
#46132=CARTESIAN_POINT('Ctrl Pts',(-2.2491010234604,1.,3.46319180177573));
#46133=CARTESIAN_POINT('Ctrl Pts',(-2.25023877475942,1.,3.47088928979888));
#46134=CARTESIAN_POINT('Ctrl Pts',(-2.25134314238687,1.,3.47860048448691));
#46135=CARTESIAN_POINT('Ctrl Pts',(-2.25241433138695,1.,3.48632513240961));
#46136=CARTESIAN_POINT('Ctrl Pts',(-2.2534525170976,1.,3.49406296494791));
#46137=CARTESIAN_POINT('Ctrl Pts',(-2.25445785151868,1.,3.50181372617971));
#46138=CARTESIAN_POINT('Ctrl Pts',(-2.25543046979799,1.,3.50957720117341));
#46139=CARTESIAN_POINT('Ctrl Pts',(-2.25637049455044,1.,3.51735323667612));
#46140=CARTESIAN_POINT('Ctrl Pts',(-2.25727802940898,1.,3.52514172847711));
#46141=CARTESIAN_POINT('Ctrl Pts',(-2.25797812950104,1.,3.53138243688262));
#46142=CARTESIAN_POINT('Ctrl Pts',(-2.25848864343951,1.,3.53606853162228));
#46143=CARTESIAN_POINT('Ctrl Pts',(-2.2588225169468,1.,3.53919506647335));
#46144=CARTESIAN_POINT('Ctrl Pts',(-2.25898783642071,1.,3.54075895182139));
#46145=CARTESIAN_POINT('Origin',(-2.25898783642071,0.,3.54075895182139));
#46146=CARTESIAN_POINT('',(-2.12928030988903,1.,3.62024382630768));
#46147=CARTESIAN_POINT('Origin',(0.,0.,0.));
#46148=CARTESIAN_POINT('',(-2.27737254473378,1.,2.97927412174388));
#46149=CARTESIAN_POINT('Origin',(0.,1.,0.));
#46150=CARTESIAN_POINT('Ctrl Pts',(-2.27737254473378,1.,2.97927412174388));
#46151=CARTESIAN_POINT('Ctrl Pts',(-2.27737254473378,0.666666666666667,
2.97927412174388));
#46152=CARTESIAN_POINT('Ctrl Pts',(-2.27737254473378,0.333333333333333,
2.97927412174388));
#46153=CARTESIAN_POINT('Ctrl Pts',(-2.27737254473378,-0.333333333333333,
2.97927412174388));
#46154=CARTESIAN_POINT('Ctrl Pts',(-2.27737254473378,-0.666666666666667,
2.97927412174388));
#46155=CARTESIAN_POINT('Ctrl Pts',(-2.27737254473378,-1.,2.97927412174388));
#46156=CARTESIAN_POINT('Ctrl Pts',(-2.66939624221984,-1.,3.24257979115744));
#46157=CARTESIAN_POINT('Ctrl Pts',(-2.66939624221984,1.,3.24257979115744));
#46158=CARTESIAN_POINT('Ctrl Pts',(-2.66795998539861,-1.,3.24193929584813));
#46159=CARTESIAN_POINT('Ctrl Pts',(-2.66795998539861,1.,3.24193929584813));
#46160=CARTESIAN_POINT('Ctrl Pts',(-2.66508964664767,-1.,3.24065561087681));
#46161=CARTESIAN_POINT('Ctrl Pts',(-2.66508964664767,1.,3.24065561087681));
#46162=CARTESIAN_POINT('Ctrl Pts',(-2.6607906631973,-1.,3.23872200036311));
#46163=CARTESIAN_POINT('Ctrl Pts',(-2.6607906631973,1.,3.23872200036311));
#46164=CARTESIAN_POINT('Ctrl Pts',(-2.6550717396303,-1.,3.23612768065687));
#46165=CARTESIAN_POINT('Ctrl Pts',(-2.6550717396303,1.,3.23612768065687));
#46166=CARTESIAN_POINT('Ctrl Pts',(-2.64794488744246,-1.,3.23285778738558));
#46167=CARTESIAN_POINT('Ctrl Pts',(-2.64794488744246,1.,3.23285778738558));
#46168=CARTESIAN_POINT('Ctrl Pts',(-2.64083992182478,-1.,3.2295608435934));
#46169=CARTESIAN_POINT('Ctrl Pts',(-2.64083992182478,1.,3.2295608435934));
#46170=CARTESIAN_POINT('Ctrl Pts',(-2.63375697391438,-1.,3.22623678292539));
#46171=CARTESIAN_POINT('Ctrl Pts',(-2.63375697391438,1.,3.22623678292539));
#46172=CARTESIAN_POINT('Ctrl Pts',(-2.62669622735548,-1.,3.222885536128));
#46173=CARTESIAN_POINT('Ctrl Pts',(-2.62669622735548,1.,3.222885536128));
#46174=CARTESIAN_POINT('Ctrl Pts',(-2.61965792832396,-1.,3.21950704108654));
#46175=CARTESIAN_POINT('Ctrl Pts',(-2.61965792832396,1.,3.21950704108654));
#46176=CARTESIAN_POINT('Ctrl Pts',(-2.61264236718662,-1.,3.21610123232465));
#46177=CARTESIAN_POINT('Ctrl Pts',(-2.61264236718662,1.,3.21610123232465));
#46178=CARTESIAN_POINT('Ctrl Pts',(-2.60564985359699,-1.,3.21266802609297));
#46179=CARTESIAN_POINT('Ctrl Pts',(-2.60564985359699,1.,3.21266802609297));
#46180=CARTESIAN_POINT('Ctrl Pts',(-2.59868069194267,-1.,3.2092073056959));
#46181=CARTESIAN_POINT('Ctrl Pts',(-2.59868069194267,1.,3.2092073056959));
#46182=CARTESIAN_POINT('Ctrl Pts',(-2.59173516023605,-1.,3.20571891028879));
#46183=CARTESIAN_POINT('Ctrl Pts',(-2.59173516023605,1.,3.20571891028879));
#46184=CARTESIAN_POINT('Ctrl Pts',(-2.58481347777953,-1.,3.20220261408685));
#46185=CARTESIAN_POINT('Ctrl Pts',(-2.58481347777953,1.,3.20220261408685));
#46186=CARTESIAN_POINT('Ctrl Pts',(-2.577915819091,-1.,3.19865814628955));
#46187=CARTESIAN_POINT('Ctrl Pts',(-2.577915819091,1.,3.19865814628955));
#46188=CARTESIAN_POINT('Ctrl Pts',(-2.57104235898053,-1.,3.19508523784548));
#46189=CARTESIAN_POINT('Ctrl Pts',(-2.57104235898053,1.,3.19508523784548));
#46190=CARTESIAN_POINT('Ctrl Pts',(-2.56419331092909,-1.,3.19148366395201));
#46191=CARTESIAN_POINT('Ctrl Pts',(-2.56419331092909,1.,3.19148366395201));
#46192=CARTESIAN_POINT('Ctrl Pts',(-2.55736896206016,-1.,3.1878532811617));
#46193=CARTESIAN_POINT('Ctrl Pts',(-2.55736896206016,1.,3.1878532811617));
#46194=CARTESIAN_POINT('Ctrl Pts',(-2.55056972387638,-1.,3.18419408529482));
#46195=CARTESIAN_POINT('Ctrl Pts',(-2.55056972387638,1.,3.18419408529482));
#46196=CARTESIAN_POINT('Ctrl Pts',(-2.54379612552948,-1.,3.18050619750515));
#46197=CARTESIAN_POINT('Ctrl Pts',(-2.54379612552948,1.,3.18050619750515));
#46198=CARTESIAN_POINT('Ctrl Pts',(-2.53704871950871,-1.,3.17678974135225));
#46199=CARTESIAN_POINT('Ctrl Pts',(-2.53704871950871,1.,3.17678974135225));
#46200=CARTESIAN_POINT('Ctrl Pts',(-2.5303280040691,-1.,3.17304474093574));
#46201=CARTESIAN_POINT('Ctrl Pts',(-2.5303280040691,1.,3.17304474093574));
#46202=CARTESIAN_POINT('Ctrl Pts',(-2.523634346718,-1.,3.16927102130751));
#46203=CARTESIAN_POINT('Ctrl Pts',(-2.523634346718,1.,3.16927102130751));
#46204=CARTESIAN_POINT('Ctrl Pts',(-2.51696788755616,-1.,3.16546808277069));
#46205=CARTESIAN_POINT('Ctrl Pts',(-2.51696788755616,1.,3.16546808277069));
#46206=CARTESIAN_POINT('Ctrl Pts',(-2.51032851007939,-1.,3.16163506380211));
#46207=CARTESIAN_POINT('Ctrl Pts',(-2.51032851007939,1.,3.16163506380211));
#46208=CARTESIAN_POINT('Ctrl Pts',(-2.50371605688287,-1.,3.15777102413998));
#46209=CARTESIAN_POINT('Ctrl Pts',(-2.50371605688287,1.,3.15777102413998));
#46210=CARTESIAN_POINT('Ctrl Pts',(-2.49713050858911,-1.,3.15387518039064));
#46211=CARTESIAN_POINT('Ctrl Pts',(-2.49713050858911,1.,3.15387518039064));
#46212=CARTESIAN_POINT('Ctrl Pts',(-2.49057217131985,-1.,3.14994715298903));
#46213=CARTESIAN_POINT('Ctrl Pts',(-2.49057217131985,1.,3.14994715298903));
#46214=CARTESIAN_POINT('Ctrl Pts',(-2.48404187418376,-1.,3.1459872272388));
#46215=CARTESIAN_POINT('Ctrl Pts',(-2.48404187418376,1.,3.1459872272388));
#46216=CARTESIAN_POINT('Ctrl Pts',(-2.47754112428028,-1.,3.14199655778845));
#46217=CARTESIAN_POINT('Ctrl Pts',(-2.47754112428028,1.,3.14199655778845));
#46218=CARTESIAN_POINT('Ctrl Pts',(-2.47107164236827,-1.,3.13797654408931));
#46219=CARTESIAN_POINT('Ctrl Pts',(-2.47107164236827,1.,3.13797654408931));
#46220=CARTESIAN_POINT('Ctrl Pts',(-2.4646349433237,-1.,3.13392826623902));
#46221=CARTESIAN_POINT('Ctrl Pts',(-2.4646349433237,1.,3.13392826623902));
#46222=CARTESIAN_POINT('Ctrl Pts',(-2.45823188859367,-1.,3.12985188384372));
#46223=CARTESIAN_POINT('Ctrl Pts',(-2.45823188859367,1.,3.12985188384372));
#46224=CARTESIAN_POINT('Ctrl Pts',(-2.45186227369848,-1.,3.12574608210849));
#46225=CARTESIAN_POINT('Ctrl Pts',(-2.45186227369848,1.,3.12574608210849));
#46226=CARTESIAN_POINT('Ctrl Pts',(-2.44552433364716,-1.,3.12160740887768));
#46227=CARTESIAN_POINT('Ctrl Pts',(-2.44552433364716,1.,3.12160740887768));
#46228=CARTESIAN_POINT('Ctrl Pts',(-2.43921571477975,-1.,3.11743156744182));
#46229=CARTESIAN_POINT('Ctrl Pts',(-2.43921571477975,1.,3.11743156744182));
#46230=CARTESIAN_POINT('Ctrl Pts',(-2.4329344968514,-1.,3.11321477659012));
#46231=CARTESIAN_POINT('Ctrl Pts',(-2.4329344968514,1.,3.11321477659012));
#46232=CARTESIAN_POINT('Ctrl Pts',(-2.42668025870013,-1.,3.10895518969592));
#46233=CARTESIAN_POINT('Ctrl Pts',(-2.42668025870013,1.,3.10895518969592));
#46234=CARTESIAN_POINT('Ctrl Pts',(-2.42045498612494,-1.,3.10465410280902));
#46235=CARTESIAN_POINT('Ctrl Pts',(-2.42045498612494,1.,3.10465410280902));
#46236=CARTESIAN_POINT('Ctrl Pts',(-2.41426441798067,-1.,3.10031775027683));
#46237=CARTESIAN_POINT('Ctrl Pts',(-2.41426441798067,1.,3.10031775027683));
#46238=CARTESIAN_POINT('Ctrl Pts',(-2.40811612696382,-1.,3.09595472616093));
#46239=CARTESIAN_POINT('Ctrl Pts',(-2.40811612696382,1.,3.09595472616093));
#46240=CARTESIAN_POINT('Ctrl Pts',(-2.40201704423352,-1.,3.09157266051115));
#46241=CARTESIAN_POINT('Ctrl Pts',(-2.40201704423352,1.,3.09157266051115));
#46242=CARTESIAN_POINT('Ctrl Pts',(-2.39597098250635,-1.,3.08717489512919));
#46243=CARTESIAN_POINT('Ctrl Pts',(-2.39597098250635,1.,3.08717489512919));
#46244=CARTESIAN_POINT('Ctrl Pts',(-2.38997659219192,-1.,3.08275773747083));
#46245=CARTESIAN_POINT('Ctrl Pts',(-2.38997659219192,1.,3.08275773747083));
#46246=CARTESIAN_POINT('Ctrl Pts',(-2.38402401216107,-1.,3.07830597244301));
#46247=CARTESIAN_POINT('Ctrl Pts',(-2.38402401216107,1.,3.07830597244301));
#46248=CARTESIAN_POINT('Ctrl Pts',(-2.37809856205524,-1.,3.07379777492133));
#46249=CARTESIAN_POINT('Ctrl Pts',(-2.37809856205524,1.,3.07379777492133));
#46250=CARTESIAN_POINT('Ctrl Pts',(-2.37218678163157,-1.,3.06921275497472));
#46251=CARTESIAN_POINT('Ctrl Pts',(-2.37218678163157,1.,3.06921275497472));
#46252=CARTESIAN_POINT('Ctrl Pts',(-2.36628220107001,-1.,3.06453964643152));
#46253=CARTESIAN_POINT('Ctrl Pts',(-2.36628220107001,1.,3.06453964643152));
#46254=CARTESIAN_POINT('Ctrl Pts',(-2.36039011602084,-1.,3.05978266240056));
#46255=CARTESIAN_POINT('Ctrl Pts',(-2.36039011602084,1.,3.05978266240056));
#46256=CARTESIAN_POINT('Ctrl Pts',(-2.35453559889506,-1.,3.05497218368188));
#46257=CARTESIAN_POINT('Ctrl Pts',(-2.35453559889506,1.,3.05497218368188));
#46258=CARTESIAN_POINT('Ctrl Pts',(-2.34875673090816,-1.,3.05015565829976));
#46259=CARTESIAN_POINT('Ctrl Pts',(-2.34875673090816,1.,3.05015565829976));
#46260=CARTESIAN_POINT('Ctrl Pts',(-2.3430901708402,-1.,3.04537822217311));
#46261=CARTESIAN_POINT('Ctrl Pts',(-2.3430901708402,1.,3.04537822217311));
#46262=CARTESIAN_POINT('Ctrl Pts',(-2.33755792953726,-1.,3.04066496998569));
#46263=CARTESIAN_POINT('Ctrl Pts',(-2.33755792953726,1.,3.04066496998569));
#46264=CARTESIAN_POINT('Ctrl Pts',(-2.33215619079807,-1.,3.03600588555765));
#46265=CARTESIAN_POINT('Ctrl Pts',(-2.33215619079807,1.,3.03600588555765));
#46266=CARTESIAN_POINT('Ctrl Pts',(-2.32683687412027,-1.,3.03133125185047));
#46267=CARTESIAN_POINT('Ctrl Pts',(-2.32683687412027,1.,3.03133125185047));
#46268=CARTESIAN_POINT('Ctrl Pts',(-2.32151944306299,-1.,3.02652678416478));
#46269=CARTESIAN_POINT('Ctrl Pts',(-2.32151944306299,1.,3.02652678416478));
#46270=CARTESIAN_POINT('Ctrl Pts',(-2.31612479121528,-1.,3.02147780668029));
#46271=CARTESIAN_POINT('Ctrl Pts',(-2.31612479121528,1.,3.02147780668029));
#46272=CARTESIAN_POINT('Ctrl Pts',(-2.31060449886577,-1.,3.01610726819019));
#46273=CARTESIAN_POINT('Ctrl Pts',(-2.31060449886577,1.,3.01610726819019));
#46274=CARTESIAN_POINT('Ctrl Pts',(-2.30496809486529,-1.,3.01041131063882));
#46275=CARTESIAN_POINT('Ctrl Pts',(-2.30496809486529,1.,3.01041131063882));
#46276=CARTESIAN_POINT('Ctrl Pts',(-2.29932091315939,-1.,3.00450832658822));
#46277=CARTESIAN_POINT('Ctrl Pts',(-2.29932091315939,1.,3.00450832658822));
#46278=CARTESIAN_POINT('Ctrl Pts',(-2.29385894577999,-1.,2.99863310340004));
#46279=CARTESIAN_POINT('Ctrl Pts',(-2.29385894577999,1.,2.99863310340004));
#46280=CARTESIAN_POINT('Ctrl Pts',(-2.28882328690601,-1.,2.9930793098434));
#46281=CARTESIAN_POINT('Ctrl Pts',(-2.28882328690601,1.,2.9930793098434));
#46282=CARTESIAN_POINT('Ctrl Pts',(-2.28446419116036,-1.,2.98815432734929));
#46283=CARTESIAN_POINT('Ctrl Pts',(-2.28446419116036,1.,2.98815432734929));
#46284=CARTESIAN_POINT('Ctrl Pts',(-2.28100472516582,-1.,2.98413343613858));
#46285=CARTESIAN_POINT('Ctrl Pts',(-2.28100472516582,1.,2.98413343613858));
#46286=CARTESIAN_POINT('Ctrl Pts',(-2.2785960133424,-1.,2.98120357932601));
#46287=CARTESIAN_POINT('Ctrl Pts',(-2.2785960133424,1.,2.98120357932601));
#46288=CARTESIAN_POINT('Ctrl Pts',(-2.27756633754846,-1.,2.97980276182744));
#46289=CARTESIAN_POINT('Ctrl Pts',(-2.27756633754846,1.,2.97980276182744));
#46290=CARTESIAN_POINT('Ctrl Pts',(-2.27730961189188,-1.,2.97929608861502));
#46291=CARTESIAN_POINT('Ctrl Pts',(-2.27730961189188,1.,2.97929608861502));
#46292=CARTESIAN_POINT('Ctrl Pts',(-2.2773674298423,-1.,2.97919987915565));
#46293=CARTESIAN_POINT('Ctrl Pts',(-2.2773674298423,1.,2.97919987915565));
#46294=CARTESIAN_POINT('Ctrl Pts',(-2.27745358485296,-1.,2.97921217251145));
#46295=CARTESIAN_POINT('Ctrl Pts',(-2.27745358485296,1.,2.97921217251145));
#46296=CARTESIAN_POINT('',(-2.66939624221984,1.,3.24257979115744));
#46297=CARTESIAN_POINT('Ctrl Pts',(-2.66939624221984,1.,3.24257979115744));
#46298=CARTESIAN_POINT('Ctrl Pts',(-2.66795998539861,1.,3.24193929584813));
#46299=CARTESIAN_POINT('Ctrl Pts',(-2.66508964664767,1.,3.24065561087681));
#46300=CARTESIAN_POINT('Ctrl Pts',(-2.6607906631973,1.,3.23872200036311));
#46301=CARTESIAN_POINT('Ctrl Pts',(-2.6550717396303,1.,3.23612768065687));
#46302=CARTESIAN_POINT('Ctrl Pts',(-2.64794488744246,1.,3.23285778738558));
#46303=CARTESIAN_POINT('Ctrl Pts',(-2.64083992182478,1.,3.2295608435934));
#46304=CARTESIAN_POINT('Ctrl Pts',(-2.63375697391438,1.,3.22623678292539));
#46305=CARTESIAN_POINT('Ctrl Pts',(-2.62669622735548,1.,3.222885536128));
#46306=CARTESIAN_POINT('Ctrl Pts',(-2.61965792832396,1.,3.21950704108654));
#46307=CARTESIAN_POINT('Ctrl Pts',(-2.61264236718662,1.,3.21610123232465));
#46308=CARTESIAN_POINT('Ctrl Pts',(-2.60564985359699,1.,3.21266802609297));
#46309=CARTESIAN_POINT('Ctrl Pts',(-2.59868069194267,1.,3.2092073056959));
#46310=CARTESIAN_POINT('Ctrl Pts',(-2.59173516023605,1.,3.20571891028879));
#46311=CARTESIAN_POINT('Ctrl Pts',(-2.58481347777953,1.,3.20220261408685));
#46312=CARTESIAN_POINT('Ctrl Pts',(-2.577915819091,1.,3.19865814628955));
#46313=CARTESIAN_POINT('Ctrl Pts',(-2.57104235898053,1.,3.19508523784548));
#46314=CARTESIAN_POINT('Ctrl Pts',(-2.56419331092909,1.,3.19148366395201));
#46315=CARTESIAN_POINT('Ctrl Pts',(-2.55736896206016,1.,3.1878532811617));
#46316=CARTESIAN_POINT('Ctrl Pts',(-2.55056972387638,1.,3.18419408529482));
#46317=CARTESIAN_POINT('Ctrl Pts',(-2.54379612552948,1.,3.18050619750515));
#46318=CARTESIAN_POINT('Ctrl Pts',(-2.53704871950871,1.,3.17678974135225));
#46319=CARTESIAN_POINT('Ctrl Pts',(-2.5303280040691,1.,3.17304474093574));
#46320=CARTESIAN_POINT('Ctrl Pts',(-2.523634346718,1.,3.16927102130751));
#46321=CARTESIAN_POINT('Ctrl Pts',(-2.51696788755616,1.,3.16546808277069));
#46322=CARTESIAN_POINT('Ctrl Pts',(-2.51032851007939,1.,3.16163506380211));
#46323=CARTESIAN_POINT('Ctrl Pts',(-2.50371605688287,1.,3.15777102413998));
#46324=CARTESIAN_POINT('Ctrl Pts',(-2.49713050858911,1.,3.15387518039064));
#46325=CARTESIAN_POINT('Ctrl Pts',(-2.49057217131985,1.,3.14994715298903));
#46326=CARTESIAN_POINT('Ctrl Pts',(-2.48404187418376,1.,3.1459872272388));
#46327=CARTESIAN_POINT('Ctrl Pts',(-2.47754112428028,1.,3.14199655778845));
#46328=CARTESIAN_POINT('Ctrl Pts',(-2.47107164236827,1.,3.13797654408931));
#46329=CARTESIAN_POINT('Ctrl Pts',(-2.4646349433237,1.,3.13392826623902));
#46330=CARTESIAN_POINT('Ctrl Pts',(-2.45823188859367,1.,3.12985188384372));
#46331=CARTESIAN_POINT('Ctrl Pts',(-2.45186227369848,1.,3.12574608210849));
#46332=CARTESIAN_POINT('Ctrl Pts',(-2.44552433364716,1.,3.12160740887768));
#46333=CARTESIAN_POINT('Ctrl Pts',(-2.43921571477975,1.,3.11743156744182));
#46334=CARTESIAN_POINT('Ctrl Pts',(-2.4329344968514,1.,3.11321477659012));
#46335=CARTESIAN_POINT('Ctrl Pts',(-2.42668025870013,1.,3.10895518969592));
#46336=CARTESIAN_POINT('Ctrl Pts',(-2.42045498612494,1.,3.10465410280902));
#46337=CARTESIAN_POINT('Ctrl Pts',(-2.41426441798067,1.,3.10031775027683));
#46338=CARTESIAN_POINT('Ctrl Pts',(-2.40811612696382,1.,3.09595472616093));
#46339=CARTESIAN_POINT('Ctrl Pts',(-2.40201704423352,1.,3.09157266051115));
#46340=CARTESIAN_POINT('Ctrl Pts',(-2.39597098250635,1.,3.08717489512919));
#46341=CARTESIAN_POINT('Ctrl Pts',(-2.38997659219192,1.,3.08275773747083));
#46342=CARTESIAN_POINT('Ctrl Pts',(-2.38402401216107,1.,3.07830597244301));
#46343=CARTESIAN_POINT('Ctrl Pts',(-2.37809856205524,1.,3.07379777492133));
#46344=CARTESIAN_POINT('Ctrl Pts',(-2.37218678163157,1.,3.06921275497472));
#46345=CARTESIAN_POINT('Ctrl Pts',(-2.36628220107001,1.,3.06453964643152));
#46346=CARTESIAN_POINT('Ctrl Pts',(-2.36039011602084,1.,3.05978266240056));
#46347=CARTESIAN_POINT('Ctrl Pts',(-2.35453559889506,1.,3.05497218368188));
#46348=CARTESIAN_POINT('Ctrl Pts',(-2.34875673090816,1.,3.05015565829976));
#46349=CARTESIAN_POINT('Ctrl Pts',(-2.3430901708402,1.,3.04537822217311));
#46350=CARTESIAN_POINT('Ctrl Pts',(-2.33755792953726,1.,3.04066496998569));
#46351=CARTESIAN_POINT('Ctrl Pts',(-2.33215619079807,1.,3.03600588555765));
#46352=CARTESIAN_POINT('Ctrl Pts',(-2.32683687412027,1.,3.03133125185047));
#46353=CARTESIAN_POINT('Ctrl Pts',(-2.32151944306299,1.,3.02652678416478));
#46354=CARTESIAN_POINT('Ctrl Pts',(-2.31612479121528,1.,3.02147780668029));
#46355=CARTESIAN_POINT('Ctrl Pts',(-2.31060449886577,1.,3.01610726819019));
#46356=CARTESIAN_POINT('Ctrl Pts',(-2.30496809486529,1.,3.01041131063882));
#46357=CARTESIAN_POINT('Ctrl Pts',(-2.29932091315939,1.,3.00450832658822));
#46358=CARTESIAN_POINT('Ctrl Pts',(-2.29385894577999,1.,2.99863310340004));
#46359=CARTESIAN_POINT('Ctrl Pts',(-2.28882328690601,1.,2.9930793098434));
#46360=CARTESIAN_POINT('Ctrl Pts',(-2.28446419116036,1.,2.98815432734929));
#46361=CARTESIAN_POINT('Ctrl Pts',(-2.28100472516582,1.,2.98413343613858));
#46362=CARTESIAN_POINT('Ctrl Pts',(-2.27877674853833,1.,2.98142341809623));
#46363=CARTESIAN_POINT('Ctrl Pts',(-2.27776738270369,1.,2.98007383024333));
#46364=CARTESIAN_POINT('Ctrl Pts',(-2.27743009389704,1.,2.97951167106106));
#46365=CARTESIAN_POINT('Ctrl Pts',(-2.27737238849212,1.,2.97932307137589));
#46366=CARTESIAN_POINT('Ctrl Pts',(-2.27737254473378,1.,2.97927412174388));
#46367=CARTESIAN_POINT('',(-2.66939624221984,0.,3.24257979115744));
#46368=CARTESIAN_POINT('Ctrl Pts',(-2.58626089374824,-1.,2.71546581445404));
#46369=CARTESIAN_POINT('Ctrl Pts',(-2.58626089374824,1.,2.71546581445404));
#46370=CARTESIAN_POINT('Ctrl Pts',(-2.58626222935804,-1.,2.71537879705104));
#46371=CARTESIAN_POINT('Ctrl Pts',(-2.58626222935804,1.,2.71537879705104));
#46372=CARTESIAN_POINT('Ctrl Pts',(-2.58636629904103,-1.,2.71533674141254));
#46373=CARTESIAN_POINT('Ctrl Pts',(-2.58636629904103,1.,2.71533674141254));
#46374=CARTESIAN_POINT('Ctrl Pts',(-2.5868265735259,-1.,2.71566956750452));
#46375=CARTESIAN_POINT('Ctrl Pts',(-2.5868265735259,1.,2.71566956750452));
#46376=CARTESIAN_POINT('Ctrl Pts',(-2.58804906785417,-1.,2.71690570241638));
#46377=CARTESIAN_POINT('Ctrl Pts',(-2.58804906785417,1.,2.71690570241638));
#46378=CARTESIAN_POINT('Ctrl Pts',(-2.59056604771971,-1.,2.71974308958086));
#46379=CARTESIAN_POINT('Ctrl Pts',(-2.59056604771971,1.,2.71974308958086));
#46380=CARTESIAN_POINT('Ctrl Pts',(-2.59399625537278,-1.,2.72378896977134));
#46381=CARTESIAN_POINT('Ctrl Pts',(-2.59399625537278,1.,2.72378896977134));
#46382=CARTESIAN_POINT('Ctrl Pts',(-2.59817869034746,-1.,2.7288648348152));
#46383=CARTESIAN_POINT('Ctrl Pts',(-2.59817869034746,1.,2.7288648348152));
#46384=CARTESIAN_POINT('Ctrl Pts',(-2.60287635688728,-1.,2.73470730109615));
#46385=CARTESIAN_POINT('Ctrl Pts',(-2.60287635688728,1.,2.73470730109615));
#46386=CARTESIAN_POINT('Ctrl Pts',(-2.60782480638448,-1.,2.7410211099909));
#46387=CARTESIAN_POINT('Ctrl Pts',(-2.60782480638448,1.,2.7410211099909));
#46388=CARTESIAN_POINT('Ctrl Pts',(-2.61277170105813,-1.,2.74752219567252));
#46389=CARTESIAN_POINT('Ctrl Pts',(-2.61277170105813,1.,2.74752219567252));
#46390=CARTESIAN_POINT('Ctrl Pts',(-2.61751580407667,-1.,2.7539802502603));
#46391=CARTESIAN_POINT('Ctrl Pts',(-2.61751580407667,1.,2.7539802502603));
#46392=CARTESIAN_POINT('Ctrl Pts',(-2.62195665834605,-1.,2.76027271596686));
#46393=CARTESIAN_POINT('Ctrl Pts',(-2.62195665834605,1.,2.76027271596686));
#46394=CARTESIAN_POINT('Ctrl Pts',(-2.62609956506355,-1.,2.76639078479021));
#46395=CARTESIAN_POINT('Ctrl Pts',(-2.62609956506355,1.,2.76639078479021));
#46396=CARTESIAN_POINT('Ctrl Pts',(-2.63001305229625,-1.,2.77239433377921));
#46397=CARTESIAN_POINT('Ctrl Pts',(-2.63001305229625,1.,2.77239433377921));
#46398=CARTESIAN_POINT('Ctrl Pts',(-2.63379800904599,-1.,2.77837943466449));
#46399=CARTESIAN_POINT('Ctrl Pts',(-2.63379800904599,1.,2.77837943466449));
#46400=CARTESIAN_POINT('Ctrl Pts',(-2.637554714303,-1.,2.78444351041571));
#46401=CARTESIAN_POINT('Ctrl Pts',(-2.637554714303,1.,2.78444351041571));
#46402=CARTESIAN_POINT('Ctrl Pts',(-2.64134450532584,-1.,2.79064495573224));
#46403=CARTESIAN_POINT('Ctrl Pts',(-2.64134450532584,1.,2.79064495573224));
#46404=CARTESIAN_POINT('Ctrl Pts',(-2.6451766779932,-1.,2.79698910670736));
#46405=CARTESIAN_POINT('Ctrl Pts',(-2.6451766779932,1.,2.79698910670736));
#46406=CARTESIAN_POINT('Ctrl Pts',(-2.64902988983337,-1.,2.80345029781152));
#46407=CARTESIAN_POINT('Ctrl Pts',(-2.64902988983337,1.,2.80345029781152));
#46408=CARTESIAN_POINT('Ctrl Pts',(-2.65286529532208,-1.,2.80998526078165));
#46409=CARTESIAN_POINT('Ctrl Pts',(-2.65286529532208,1.,2.80998526078165));
#46410=CARTESIAN_POINT('Ctrl Pts',(-2.65664198781344,-1.,2.81654896073883));
#46411=CARTESIAN_POINT('Ctrl Pts',(-2.65664198781344,1.,2.81654896073883));
#46412=CARTESIAN_POINT('Ctrl Pts',(-2.66033388273461,-1.,2.82311188135078));
#46413=CARTESIAN_POINT('Ctrl Pts',(-2.66033388273461,1.,2.82311188135078));
#46414=CARTESIAN_POINT('Ctrl Pts',(-2.6639376472693,-1.,2.82966813308998));
#46415=CARTESIAN_POINT('Ctrl Pts',(-2.6639376472693,1.,2.82966813308998));
#46416=CARTESIAN_POINT('Ctrl Pts',(-2.66746339678107,-1.,2.83622586853982));
#46417=CARTESIAN_POINT('Ctrl Pts',(-2.66746339678107,1.,2.83622586853982));
#46418=CARTESIAN_POINT('Ctrl Pts',(-2.67092916452125,-1.,2.84280157191323));
#46419=CARTESIAN_POINT('Ctrl Pts',(-2.67092916452125,1.,2.84280157191323));
#46420=CARTESIAN_POINT('Ctrl Pts',(-2.67435421039677,-1.,2.84941315703092));
#46421=CARTESIAN_POINT('Ctrl Pts',(-2.67435421039677,1.,2.84941315703092));
#46422=CARTESIAN_POINT('Ctrl Pts',(-2.67775201955724,-1.,2.85607274378018));
#46423=CARTESIAN_POINT('Ctrl Pts',(-2.67775201955724,1.,2.85607274378018));
#46424=CARTESIAN_POINT('Ctrl Pts',(-2.68112602796308,-1.,2.86278224277689));
#46425=CARTESIAN_POINT('Ctrl Pts',(-2.68112602796308,1.,2.86278224277689));
#46426=CARTESIAN_POINT('Ctrl Pts',(-2.68447353139599,-1.,2.86953736547238));
#46427=CARTESIAN_POINT('Ctrl Pts',(-2.68447353139599,1.,2.86953736547238));
#46428=CARTESIAN_POINT('Ctrl Pts',(-2.68778807801686,-1.,2.8763300724388));
#46429=CARTESIAN_POINT('Ctrl Pts',(-2.68778807801686,1.,2.8763300724388));
#46430=CARTESIAN_POINT('Ctrl Pts',(-2.69106236420198,-1.,2.88315153980466));
#46431=CARTESIAN_POINT('Ctrl Pts',(-2.69106236420198,1.,2.88315153980466));
#46432=CARTESIAN_POINT('Ctrl Pts',(-2.69429113011374,-1.,2.88999512410309));
#46433=CARTESIAN_POINT('Ctrl Pts',(-2.69429113011374,1.,2.88999512410309));
#46434=CARTESIAN_POINT('Ctrl Pts',(-2.69747340630625,-1.,2.89685866123671));
#46435=CARTESIAN_POINT('Ctrl Pts',(-2.69747340630625,1.,2.89685866123671));
#46436=CARTESIAN_POINT('Ctrl Pts',(-2.70061095078692,-1.,2.90374285605838));
#46437=CARTESIAN_POINT('Ctrl Pts',(-2.70061095078692,1.,2.90374285605838));
#46438=CARTESIAN_POINT('Ctrl Pts',(-2.70370719782113,-1.,2.91065019668329));
#46439=CARTESIAN_POINT('Ctrl Pts',(-2.70370719782113,1.,2.91065019668329));
#46440=CARTESIAN_POINT('Ctrl Pts',(-2.70676602302518,-1.,2.91758367994737));
#46441=CARTESIAN_POINT('Ctrl Pts',(-2.70676602302518,1.,2.91758367994737));
#46442=CARTESIAN_POINT('Ctrl Pts',(-2.70979055994754,-1.,2.92454558914778));
#46443=CARTESIAN_POINT('Ctrl Pts',(-2.70979055994754,1.,2.92454558914778));
#46444=CARTESIAN_POINT('Ctrl Pts',(-2.71278207520817,-1.,2.93153633192595));
#46445=CARTESIAN_POINT('Ctrl Pts',(-2.71278207520817,1.,2.93153633192595));
#46446=CARTESIAN_POINT('Ctrl Pts',(-2.71574054592591,-1.,2.93855503247266));
#46447=CARTESIAN_POINT('Ctrl Pts',(-2.71574054592591,1.,2.93855503247266));
#46448=CARTESIAN_POINT('Ctrl Pts',(-2.71866514227965,-1.,2.94560002559806));
#46449=CARTESIAN_POINT('Ctrl Pts',(-2.71866514227965,1.,2.94560002559806));
#46450=CARTESIAN_POINT('Ctrl Pts',(-2.72155475123364,-1.,2.95266939280621));
#46451=CARTESIAN_POINT('Ctrl Pts',(-2.72155475123364,1.,2.95266939280621));
#46452=CARTESIAN_POINT('Ctrl Pts',(-2.72440846811729,-1.,2.95976146492576));
#46453=CARTESIAN_POINT('Ctrl Pts',(-2.72440846811729,1.,2.95976146492576));
#46454=CARTESIAN_POINT('Ctrl Pts',(-2.72722614084076,-1.,2.96687537842451));
#46455=CARTESIAN_POINT('Ctrl Pts',(-2.72722614084076,1.,2.96687537842451));
#46456=CARTESIAN_POINT('Ctrl Pts',(-2.73000819218414,-1.,2.97401089032677));
#46457=CARTESIAN_POINT('Ctrl Pts',(-2.73000819218414,1.,2.97401089032677));
#46458=CARTESIAN_POINT('Ctrl Pts',(-2.73275539286497,-1.,2.98116814232129));
#46459=CARTESIAN_POINT('Ctrl Pts',(-2.73275539286497,1.,2.98116814232129));
#46460=CARTESIAN_POINT('Ctrl Pts',(-2.73546864694536,-1.,2.9883474369644));
#46461=CARTESIAN_POINT('Ctrl Pts',(-2.73546864694536,1.,2.9883474369644));
#46462=CARTESIAN_POINT('Ctrl Pts',(-2.73814878711641,-1.,2.99554902409778));
#46463=CARTESIAN_POINT('Ctrl Pts',(-2.73814878711641,1.,2.99554902409778));
#46464=CARTESIAN_POINT('Ctrl Pts',(-2.74079632883931,-1.,3.00277284351521));
#46465=CARTESIAN_POINT('Ctrl Pts',(-2.74079632883931,1.,3.00277284351521));
#46466=CARTESIAN_POINT('Ctrl Pts',(-2.74341150239887,-1.,3.01001855960162));
#46467=CARTESIAN_POINT('Ctrl Pts',(-2.74341150239887,1.,3.01001855960162));
#46468=CARTESIAN_POINT('Ctrl Pts',(-2.74599436193625,-1.,3.01728567646611));
#46469=CARTESIAN_POINT('Ctrl Pts',(-2.74599436193625,1.,3.01728567646611));
#46470=CARTESIAN_POINT('Ctrl Pts',(-2.7485448718414,-1.,3.02457362909245));
#46471=CARTESIAN_POINT('Ctrl Pts',(-2.7485448718414,1.,3.02457362909245));
#46472=CARTESIAN_POINT('Ctrl Pts',(-2.75106299522979,-1.,3.03188187589107));
#46473=CARTESIAN_POINT('Ctrl Pts',(-2.75106299522979,1.,3.03188187589107));
#46474=CARTESIAN_POINT('Ctrl Pts',(-2.75354880060314,-1.,3.03921001107977));
#46475=CARTESIAN_POINT('Ctrl Pts',(-2.75354880060314,1.,3.03921001107977));
#46476=CARTESIAN_POINT('Ctrl Pts',(-2.75600247455925,-1.,3.04655777351067));
#46477=CARTESIAN_POINT('Ctrl Pts',(-2.75600247455925,1.,3.04655777351067));
#46478=CARTESIAN_POINT('Ctrl Pts',(-2.75842427252931,-1.,3.05392498749847));
#46479=CARTESIAN_POINT('Ctrl Pts',(-2.75842427252931,1.,3.05392498749847));
#46480=CARTESIAN_POINT('Ctrl Pts',(-2.76081448759882,-1.,3.06131152247454));
#46481=CARTESIAN_POINT('Ctrl Pts',(-2.76081448759882,1.,3.06131152247454));
#46482=CARTESIAN_POINT('Ctrl Pts',(-2.76317341453493,-1.,3.0687172484321));
#46483=CARTESIAN_POINT('Ctrl Pts',(-2.76317341453493,1.,3.0687172484321));
#46484=CARTESIAN_POINT('Ctrl Pts',(-2.76550131064852,-1.,3.07614198408862));
#46485=CARTESIAN_POINT('Ctrl Pts',(-2.76550131064852,1.,3.07614198408862));
#46486=CARTESIAN_POINT('Ctrl Pts',(-2.76779837829373,-1.,3.08358548001504));
#46487=CARTESIAN_POINT('Ctrl Pts',(-2.76779837829373,1.,3.08358548001504));
#46488=CARTESIAN_POINT('Ctrl Pts',(-2.7700647803451,-1.,3.09104745382531));
#46489=CARTESIAN_POINT('Ctrl Pts',(-2.7700647803451,1.,3.09104745382531));
#46490=CARTESIAN_POINT('Ctrl Pts',(-2.77230064796057,-1.,3.0985276127786));
#46491=CARTESIAN_POINT('Ctrl Pts',(-2.77230064796057,1.,3.0985276127786));
#46492=CARTESIAN_POINT('Ctrl Pts',(-2.77450609123362,-1.,3.10602568032564));
#46493=CARTESIAN_POINT('Ctrl Pts',(-2.77450609123362,1.,3.10602568032564));
#46494=CARTESIAN_POINT('Ctrl Pts',(-2.77668121002545,-1.,3.11354142303921));
#46495=CARTESIAN_POINT('Ctrl Pts',(-2.77668121002545,1.,3.11354142303921));
#46496=CARTESIAN_POINT('Ctrl Pts',(-2.77882610146731,-1.,3.12107467037201));
#46497=CARTESIAN_POINT('Ctrl Pts',(-2.77882610146731,1.,3.12107467037201));
#46498=CARTESIAN_POINT('Ctrl Pts',(-2.78094085161413,-1.,3.12862530318457));
#46499=CARTESIAN_POINT('Ctrl Pts',(-2.78094085161413,1.,3.12862530318457));
#46500=CARTESIAN_POINT('Ctrl Pts',(-2.78260859419319,-1.,3.13467965833037));
#46501=CARTESIAN_POINT('Ctrl Pts',(-2.78260859419319,1.,3.13467965833037));
#46502=CARTESIAN_POINT('Ctrl Pts',(-2.78384588958166,-1.,3.13922819749279));
#46503=CARTESIAN_POINT('Ctrl Pts',(-2.78384588958166,1.,3.13922819749279));
#46504=CARTESIAN_POINT('Ctrl Pts',(-2.7846647503589,-1.,3.14226401018816));
#46505=CARTESIAN_POINT('Ctrl Pts',(-2.7846647503589,1.,3.14226401018816));
#46506=CARTESIAN_POINT('Ctrl Pts',(-2.78507268004356,-1.,3.14378277984898));
#46507=CARTESIAN_POINT('Ctrl Pts',(-2.78507268004356,1.,3.14378277984898));
#46508=CARTESIAN_POINT('',(-2.58633475774921,1.,2.71539546306948));
#46509=CARTESIAN_POINT('Ctrl Pts',(-2.58633475774921,-1.,2.71539546306948));
#46510=CARTESIAN_POINT('Ctrl Pts',(-2.58633475774921,-0.666666666666667,
2.71539546306948));
#46511=CARTESIAN_POINT('Ctrl Pts',(-2.58633475774921,-0.333333333333333,
2.71539546306948));
#46512=CARTESIAN_POINT('Ctrl Pts',(-2.58633475774921,0.333333333333333,
2.71539546306948));
#46513=CARTESIAN_POINT('Ctrl Pts',(-2.58633475774921,0.666666666666667,
2.71539546306948));
#46514=CARTESIAN_POINT('Ctrl Pts',(-2.58633475774921,1.,2.71539546306948));
#46515=CARTESIAN_POINT('',(-2.78507268004356,1.,3.14378277984898));
#46516=CARTESIAN_POINT('',(-2.78507268004356,0.,3.14378277984898));
#46517=CARTESIAN_POINT('Ctrl Pts',(-2.58633475774921,1.,2.71539546306948));
#46518=CARTESIAN_POINT('Ctrl Pts',(-2.58638312917167,1.,2.71540296616024));
#46519=CARTESIAN_POINT('Ctrl Pts',(-2.58656037976753,1.,2.71548946460575));
#46520=CARTESIAN_POINT('Ctrl Pts',(-2.58706285424358,1.,2.71591054189786));
#46521=CARTESIAN_POINT('Ctrl Pts',(-2.58823792682672,1.,2.71711860281815));
#46522=CARTESIAN_POINT('Ctrl Pts',(-2.59056604771971,1.,2.71974308958086));
#46523=CARTESIAN_POINT('Ctrl Pts',(-2.59399625537278,1.,2.72378896977134));
#46524=CARTESIAN_POINT('Ctrl Pts',(-2.59817869034746,1.,2.7288648348152));
#46525=CARTESIAN_POINT('Ctrl Pts',(-2.60287635688728,1.,2.73470730109615));
#46526=CARTESIAN_POINT('Ctrl Pts',(-2.60782480638448,1.,2.7410211099909));
#46527=CARTESIAN_POINT('Ctrl Pts',(-2.61277170105813,1.,2.74752219567252));
#46528=CARTESIAN_POINT('Ctrl Pts',(-2.61751580407667,1.,2.7539802502603));
#46529=CARTESIAN_POINT('Ctrl Pts',(-2.62195665834605,1.,2.76027271596686));
#46530=CARTESIAN_POINT('Ctrl Pts',(-2.62609956506355,1.,2.76639078479021));
#46531=CARTESIAN_POINT('Ctrl Pts',(-2.63001305229625,1.,2.77239433377921));
#46532=CARTESIAN_POINT('Ctrl Pts',(-2.63379800904599,1.,2.77837943466449));
#46533=CARTESIAN_POINT('Ctrl Pts',(-2.637554714303,1.,2.78444351041571));
#46534=CARTESIAN_POINT('Ctrl Pts',(-2.64134450532584,1.,2.79064495573224));
#46535=CARTESIAN_POINT('Ctrl Pts',(-2.6451766779932,1.,2.79698910670736));
#46536=CARTESIAN_POINT('Ctrl Pts',(-2.64902988983337,1.,2.80345029781152));
#46537=CARTESIAN_POINT('Ctrl Pts',(-2.65286529532208,1.,2.80998526078165));
#46538=CARTESIAN_POINT('Ctrl Pts',(-2.65664198781344,1.,2.81654896073883));
#46539=CARTESIAN_POINT('Ctrl Pts',(-2.66033388273461,1.,2.82311188135078));
#46540=CARTESIAN_POINT('Ctrl Pts',(-2.6639376472693,1.,2.82966813308998));
#46541=CARTESIAN_POINT('Ctrl Pts',(-2.66746339678107,1.,2.83622586853982));
#46542=CARTESIAN_POINT('Ctrl Pts',(-2.67092916452125,1.,2.84280157191323));
#46543=CARTESIAN_POINT('Ctrl Pts',(-2.67435421039677,1.,2.84941315703092));
#46544=CARTESIAN_POINT('Ctrl Pts',(-2.67775201955724,1.,2.85607274378018));
#46545=CARTESIAN_POINT('Ctrl Pts',(-2.68112602796308,1.,2.86278224277689));
#46546=CARTESIAN_POINT('Ctrl Pts',(-2.68447353139599,1.,2.86953736547238));
#46547=CARTESIAN_POINT('Ctrl Pts',(-2.68778807801686,1.,2.8763300724388));
#46548=CARTESIAN_POINT('Ctrl Pts',(-2.69106236420198,1.,2.88315153980466));
#46549=CARTESIAN_POINT('Ctrl Pts',(-2.69429113011374,1.,2.88999512410309));
#46550=CARTESIAN_POINT('Ctrl Pts',(-2.69747340630625,1.,2.89685866123671));
#46551=CARTESIAN_POINT('Ctrl Pts',(-2.70061095078692,1.,2.90374285605838));
#46552=CARTESIAN_POINT('Ctrl Pts',(-2.70370719782113,1.,2.91065019668329));
#46553=CARTESIAN_POINT('Ctrl Pts',(-2.70676602302518,1.,2.91758367994737));
#46554=CARTESIAN_POINT('Ctrl Pts',(-2.70979055994754,1.,2.92454558914778));
#46555=CARTESIAN_POINT('Ctrl Pts',(-2.71278207520817,1.,2.93153633192595));
#46556=CARTESIAN_POINT('Ctrl Pts',(-2.71574054592591,1.,2.93855503247266));
#46557=CARTESIAN_POINT('Ctrl Pts',(-2.71866514227965,1.,2.94560002559806));
#46558=CARTESIAN_POINT('Ctrl Pts',(-2.72155475123364,1.,2.95266939280621));
#46559=CARTESIAN_POINT('Ctrl Pts',(-2.72440846811729,1.,2.95976146492576));
#46560=CARTESIAN_POINT('Ctrl Pts',(-2.72722614084076,1.,2.96687537842451));
#46561=CARTESIAN_POINT('Ctrl Pts',(-2.73000819218414,1.,2.97401089032677));
#46562=CARTESIAN_POINT('Ctrl Pts',(-2.73275539286497,1.,2.98116814232129));
#46563=CARTESIAN_POINT('Ctrl Pts',(-2.73546864694536,1.,2.9883474369644));
#46564=CARTESIAN_POINT('Ctrl Pts',(-2.73814878711641,1.,2.99554902409778));
#46565=CARTESIAN_POINT('Ctrl Pts',(-2.74079632883931,1.,3.00277284351521));
#46566=CARTESIAN_POINT('Ctrl Pts',(-2.74341150239887,1.,3.01001855960162));
#46567=CARTESIAN_POINT('Ctrl Pts',(-2.74599436193625,1.,3.01728567646611));
#46568=CARTESIAN_POINT('Ctrl Pts',(-2.7485448718414,1.,3.02457362909245));
#46569=CARTESIAN_POINT('Ctrl Pts',(-2.75106299522979,1.,3.03188187589107));
#46570=CARTESIAN_POINT('Ctrl Pts',(-2.75354880060314,1.,3.03921001107977));
#46571=CARTESIAN_POINT('Ctrl Pts',(-2.75600247455925,1.,3.04655777351067));
#46572=CARTESIAN_POINT('Ctrl Pts',(-2.75842427252931,1.,3.05392498749847));
#46573=CARTESIAN_POINT('Ctrl Pts',(-2.76081448759882,1.,3.06131152247454));
#46574=CARTESIAN_POINT('Ctrl Pts',(-2.76317341453493,1.,3.0687172484321));
#46575=CARTESIAN_POINT('Ctrl Pts',(-2.76550131064852,1.,3.07614198408862));
#46576=CARTESIAN_POINT('Ctrl Pts',(-2.76779837829373,1.,3.08358548001504));
#46577=CARTESIAN_POINT('Ctrl Pts',(-2.7700647803451,1.,3.09104745382531));
#46578=CARTESIAN_POINT('Ctrl Pts',(-2.77230064796057,1.,3.0985276127786));
#46579=CARTESIAN_POINT('Ctrl Pts',(-2.77450609123362,1.,3.10602568032564));
#46580=CARTESIAN_POINT('Ctrl Pts',(-2.77668121002545,1.,3.11354142303921));
#46581=CARTESIAN_POINT('Ctrl Pts',(-2.77882610146731,1.,3.12107467037201));
#46582=CARTESIAN_POINT('Ctrl Pts',(-2.78094085161413,1.,3.12862530318457));
#46583=CARTESIAN_POINT('Ctrl Pts',(-2.78260859419319,1.,3.13467965833037));
#46584=CARTESIAN_POINT('Ctrl Pts',(-2.78384588958166,1.,3.13922819749279));
#46585=CARTESIAN_POINT('Ctrl Pts',(-2.7846647503589,1.,3.14226401018816));
#46586=CARTESIAN_POINT('Ctrl Pts',(-2.78507268004356,1.,3.14378277984898));
#46587=CARTESIAN_POINT('Origin',(-2.78507268004356,0.,3.14378277984898));
#46588=CARTESIAN_POINT('',(-2.66939624221984,1.,3.24257979115744));
#46589=CARTESIAN_POINT('Origin',(0.,0.,0.));
#46590=CARTESIAN_POINT('',(-2.71539546306824,1.,2.58633475775051));
#46591=CARTESIAN_POINT('Origin',(0.,1.,0.));
#46592=CARTESIAN_POINT('Ctrl Pts',(-2.71539546306824,1.,2.58633475775051));
#46593=CARTESIAN_POINT('Ctrl Pts',(-2.71539546306824,0.666666666666667,
2.58633475775051));
#46594=CARTESIAN_POINT('Ctrl Pts',(-2.71539546306824,0.333333333333333,
2.58633475775051));
#46595=CARTESIAN_POINT('Ctrl Pts',(-2.71539546306824,-0.333333333333333,
2.58633475775051));
#46596=CARTESIAN_POINT('Ctrl Pts',(-2.71539546306824,-0.666666666666667,
2.58633475775051));
#46597=CARTESIAN_POINT('Ctrl Pts',(-2.71539546306824,-1.,2.58633475775051));
#46598=CARTESIAN_POINT('Ctrl Pts',(-3.14378277984898,-1.,2.78507268004356));
#46599=CARTESIAN_POINT('Ctrl Pts',(-3.14378277984898,1.,2.78507268004356));
#46600=CARTESIAN_POINT('Ctrl Pts',(-3.14226401019149,-1.,2.78466475036183));
#46601=CARTESIAN_POINT('Ctrl Pts',(-3.14226401019149,1.,2.78466475036183));
#46602=CARTESIAN_POINT('Ctrl Pts',(-3.13922819750185,-1.,2.78384588958965));
#46603=CARTESIAN_POINT('Ctrl Pts',(-3.13922819750185,1.,2.78384588958965));
#46604=CARTESIAN_POINT('Ctrl Pts',(-3.1346796583452,-1.,2.78260859420629));
#46605=CARTESIAN_POINT('Ctrl Pts',(-3.1346796583452,1.,2.78260859420629));
#46606=CARTESIAN_POINT('Ctrl Pts',(-3.12862530320194,-1.,2.78094085162947));
#46607=CARTESIAN_POINT('Ctrl Pts',(-3.12862530320194,1.,2.78094085162947));
#46608=CARTESIAN_POINT('Ctrl Pts',(-3.12107467038623,-1.,2.77882610147986));
#46609=CARTESIAN_POINT('Ctrl Pts',(-3.12107467038623,1.,2.77882610147986));
#46610=CARTESIAN_POINT('Ctrl Pts',(-3.11354142304692,-1.,2.77668121003225));
#46611=CARTESIAN_POINT('Ctrl Pts',(-3.11354142304692,1.,2.77668121003225));
#46612=CARTESIAN_POINT('Ctrl Pts',(-3.10602568032641,-1.,2.7745060912343));
#46613=CARTESIAN_POINT('Ctrl Pts',(-3.10602568032641,1.,2.7745060912343));
#46614=CARTESIAN_POINT('Ctrl Pts',(-3.09852761277432,-1.,2.77230064795679));
#46615=CARTESIAN_POINT('Ctrl Pts',(-3.09852761277432,1.,2.77230064795679));
#46616=CARTESIAN_POINT('Ctrl Pts',(-3.09104745381882,-1.,2.77006478033937));
#46617=CARTESIAN_POINT('Ctrl Pts',(-3.09104745381882,1.,2.77006478033937));
#46618=CARTESIAN_POINT('Ctrl Pts',(-3.08358548000904,-1.,2.76779837828843));
#46619=CARTESIAN_POINT('Ctrl Pts',(-3.08358548000904,1.,2.76779837828843));
#46620=CARTESIAN_POINT('Ctrl Pts',(-3.07614198408488,-1.,2.76550131064522));
#46621=CARTESIAN_POINT('Ctrl Pts',(-3.07614198408488,1.,2.76550131064522));
#46622=CARTESIAN_POINT('Ctrl Pts',(-3.06871724843121,-1.,2.76317341453415));
#46623=CARTESIAN_POINT('Ctrl Pts',(-3.06871724843121,1.,2.76317341453415));
#46624=CARTESIAN_POINT('Ctrl Pts',(-3.06131152247599,-1.,2.76081448760011));
#46625=CARTESIAN_POINT('Ctrl Pts',(-3.06131152247599,1.,2.76081448760011));
#46626=CARTESIAN_POINT('Ctrl Pts',(-3.05392498750112,-1.,2.75842427253164));
#46627=CARTESIAN_POINT('Ctrl Pts',(-3.05392498750112,1.,2.75842427253164));
#46628=CARTESIAN_POINT('Ctrl Pts',(-3.04655777351333,-1.,2.7560024745616));
#46629=CARTESIAN_POINT('Ctrl Pts',(-3.04655777351333,1.,2.7560024745616));
#46630=CARTESIAN_POINT('Ctrl Pts',(-3.03921001108158,-1.,2.75354880060473));
#46631=CARTESIAN_POINT('Ctrl Pts',(-3.03921001108158,1.,2.75354880060473));
#46632=CARTESIAN_POINT('Ctrl Pts',(-3.03188187589168,-1.,2.75106299523032));
#46633=CARTESIAN_POINT('Ctrl Pts',(-3.03188187589168,1.,2.75106299523032));
#46634=CARTESIAN_POINT('Ctrl Pts',(-3.02457362909199,-1.,2.74854487184099));
#46635=CARTESIAN_POINT('Ctrl Pts',(-3.02457362909199,1.,2.74854487184099));
#46636=CARTESIAN_POINT('Ctrl Pts',(-3.01728567646502,-1.,2.74599436193528));
#46637=CARTESIAN_POINT('Ctrl Pts',(-3.01728567646502,1.,2.74599436193528));
#46638=CARTESIAN_POINT('Ctrl Pts',(-3.01001855960041,-1.,2.7434115023978));
#46639=CARTESIAN_POINT('Ctrl Pts',(-3.01001855960041,1.,2.7434115023978));
#46640=CARTESIAN_POINT('Ctrl Pts',(-3.00277284351431,-1.,2.74079632883852));
#46641=CARTESIAN_POINT('Ctrl Pts',(-3.00277284351431,1.,2.74079632883852));
#46642=CARTESIAN_POINT('Ctrl Pts',(-2.99554902409741,-1.,2.73814878711609));
#46643=CARTESIAN_POINT('Ctrl Pts',(-2.99554902409741,1.,2.73814878711609));
#46644=CARTESIAN_POINT('Ctrl Pts',(-2.98834743696455,-1.,2.73546864694548));
#46645=CARTESIAN_POINT('Ctrl Pts',(-2.98834743696455,1.,2.73546864694548));
#46646=CARTESIAN_POINT('Ctrl Pts',(-2.98116814232175,-1.,2.73275539286537));
#46647=CARTESIAN_POINT('Ctrl Pts',(-2.98116814232175,1.,2.73275539286537));
#46648=CARTESIAN_POINT('Ctrl Pts',(-2.97401089032729,-1.,2.7300081921846));
#46649=CARTESIAN_POINT('Ctrl Pts',(-2.97401089032729,1.,2.7300081921846));
#46650=CARTESIAN_POINT('Ctrl Pts',(-2.96687537842492,-1.,2.72722614084112));
#46651=CARTESIAN_POINT('Ctrl Pts',(-2.96687537842492,1.,2.72722614084112));
#46652=CARTESIAN_POINT('Ctrl Pts',(-2.95976146492595,-1.,2.72440846811745));
#46653=CARTESIAN_POINT('Ctrl Pts',(-2.95976146492595,1.,2.72440846811745));
#46654=CARTESIAN_POINT('Ctrl Pts',(-2.95266939280617,-1.,2.72155475123361));
#46655=CARTESIAN_POINT('Ctrl Pts',(-2.95266939280617,1.,2.72155475123361));
#46656=CARTESIAN_POINT('Ctrl Pts',(-2.94560002559789,-1.,2.71866514227952));
#46657=CARTESIAN_POINT('Ctrl Pts',(-2.94560002559789,1.,2.71866514227952));
#46658=CARTESIAN_POINT('Ctrl Pts',(-2.93855503247248,-1.,2.71574054592575));
#46659=CARTESIAN_POINT('Ctrl Pts',(-2.93855503247248,1.,2.71574054592575));
#46660=CARTESIAN_POINT('Ctrl Pts',(-2.93153633192583,-1.,2.71278207520807));
#46661=CARTESIAN_POINT('Ctrl Pts',(-2.93153633192583,1.,2.71278207520807));
#46662=CARTESIAN_POINT('Ctrl Pts',(-2.92454558914774,-1.,2.70979055994751));
#46663=CARTESIAN_POINT('Ctrl Pts',(-2.92454558914774,1.,2.70979055994751));
#46664=CARTESIAN_POINT('Ctrl Pts',(-2.91758367994738,-1.,2.70676602302518));
#46665=CARTESIAN_POINT('Ctrl Pts',(-2.91758367994738,1.,2.70676602302518));
#46666=CARTESIAN_POINT('Ctrl Pts',(-2.91065019668331,-1.,2.70370719782114));
#46667=CARTESIAN_POINT('Ctrl Pts',(-2.91065019668331,1.,2.70370719782114));
#46668=CARTESIAN_POINT('Ctrl Pts',(-2.90374285605839,-1.,2.70061095078692));
#46669=CARTESIAN_POINT('Ctrl Pts',(-2.90374285605839,1.,2.70061095078692));
#46670=CARTESIAN_POINT('Ctrl Pts',(-2.89685866123668,-1.,2.69747340630621));
#46671=CARTESIAN_POINT('Ctrl Pts',(-2.89685866123668,1.,2.69747340630621));
#46672=CARTESIAN_POINT('Ctrl Pts',(-2.88999512410304,-1.,2.69429113011369));
#46673=CARTESIAN_POINT('Ctrl Pts',(-2.88999512410304,1.,2.69429113011369));
#46674=CARTESIAN_POINT('Ctrl Pts',(-2.88315153980464,-1.,2.69106236420197));
#46675=CARTESIAN_POINT('Ctrl Pts',(-2.88315153980464,1.,2.69106236420197));
#46676=CARTESIAN_POINT('Ctrl Pts',(-2.87633007243885,-1.,2.68778807801691));
#46677=CARTESIAN_POINT('Ctrl Pts',(-2.87633007243885,1.,2.68778807801691));
#46678=CARTESIAN_POINT('Ctrl Pts',(-2.8695373654725,-1.,2.68447353139611));
#46679=CARTESIAN_POINT('Ctrl Pts',(-2.8695373654725,1.,2.68447353139611));
#46680=CARTESIAN_POINT('Ctrl Pts',(-2.86278224277705,-1.,2.68112602796323));
#46681=CARTESIAN_POINT('Ctrl Pts',(-2.86278224277705,1.,2.68112602796323));
#46682=CARTESIAN_POINT('Ctrl Pts',(-2.85607274378031,-1.,2.67775201955736));
#46683=CARTESIAN_POINT('Ctrl Pts',(-2.85607274378031,1.,2.67775201955736));
#46684=CARTESIAN_POINT('Ctrl Pts',(-2.84941315703096,-1.,2.67435421039682));
#46685=CARTESIAN_POINT('Ctrl Pts',(-2.84941315703096,1.,2.67435421039682));
#46686=CARTESIAN_POINT('Ctrl Pts',(-2.84280157191314,-1.,2.67092916452117));
#46687=CARTESIAN_POINT('Ctrl Pts',(-2.84280157191314,1.,2.67092916452117));
#46688=CARTESIAN_POINT('Ctrl Pts',(-2.8362258685396,-1.,2.66746339678085));
#46689=CARTESIAN_POINT('Ctrl Pts',(-2.8362258685396,1.,2.66746339678085));
#46690=CARTESIAN_POINT('Ctrl Pts',(-2.82966813308969,-1.,2.66393764726902));
#46691=CARTESIAN_POINT('Ctrl Pts',(-2.82966813308969,1.,2.66393764726902));
#46692=CARTESIAN_POINT('Ctrl Pts',(-2.82311188135053,-1.,2.66033388273437));
#46693=CARTESIAN_POINT('Ctrl Pts',(-2.82311188135053,1.,2.66033388273437));
#46694=CARTESIAN_POINT('Ctrl Pts',(-2.81654896073874,-1.,2.65664198781335));
#46695=CARTESIAN_POINT('Ctrl Pts',(-2.81654896073874,1.,2.65664198781335));
#46696=CARTESIAN_POINT('Ctrl Pts',(-2.80998526078179,-1.,2.65286529532221));
#46697=CARTESIAN_POINT('Ctrl Pts',(-2.80998526078179,1.,2.65286529532221));
#46698=CARTESIAN_POINT('Ctrl Pts',(-2.80345029781191,-1.,2.64902988983373));
#46699=CARTESIAN_POINT('Ctrl Pts',(-2.80345029781191,1.,2.64902988983373));
#46700=CARTESIAN_POINT('Ctrl Pts',(-2.7969891067079,-1.,2.6451766779937));
#46701=CARTESIAN_POINT('Ctrl Pts',(-2.7969891067079,1.,2.6451766779937));
#46702=CARTESIAN_POINT('Ctrl Pts',(-2.79064495573275,-1.,2.64134450532632));
#46703=CARTESIAN_POINT('Ctrl Pts',(-2.79064495573275,1.,2.64134450532632));
#46704=CARTESIAN_POINT('Ctrl Pts',(-2.78444351041594,-1.,2.63755471430322));
#46705=CARTESIAN_POINT('Ctrl Pts',(-2.78444351041594,1.,2.63755471430322));
#46706=CARTESIAN_POINT('Ctrl Pts',(-2.77837943466423,-1.,2.63379800904575));
#46707=CARTESIAN_POINT('Ctrl Pts',(-2.77837943466423,1.,2.63379800904575));
#46708=CARTESIAN_POINT('Ctrl Pts',(-2.77239433377839,-1.,2.63001305229548));
#46709=CARTESIAN_POINT('Ctrl Pts',(-2.77239433377839,1.,2.63001305229548));
#46710=CARTESIAN_POINT('Ctrl Pts',(-2.76639078478898,-1.,2.6260995650624));
#46711=CARTESIAN_POINT('Ctrl Pts',(-2.76639078478898,1.,2.6260995650624));
#46712=CARTESIAN_POINT('Ctrl Pts',(-2.76027271596564,-1.,2.62195665834491));
#46713=CARTESIAN_POINT('Ctrl Pts',(-2.76027271596564,1.,2.62195665834491));
#46714=CARTESIAN_POINT('Ctrl Pts',(-2.75398025025967,-1.,2.61751580407608));
#46715=CARTESIAN_POINT('Ctrl Pts',(-2.75398025025967,1.,2.61751580407608));
#46716=CARTESIAN_POINT('Ctrl Pts',(-2.74752219567307,-1.,2.61277170105864));
#46717=CARTESIAN_POINT('Ctrl Pts',(-2.74752219567307,1.,2.61277170105864));
#46718=CARTESIAN_POINT('Ctrl Pts',(-2.74102110999284,-1.,2.60782480638629));
#46719=CARTESIAN_POINT('Ctrl Pts',(-2.74102110999284,1.,2.60782480638629));
#46720=CARTESIAN_POINT('Ctrl Pts',(-2.73470730109906,-1.,2.60287635689));
#46721=CARTESIAN_POINT('Ctrl Pts',(-2.73470730109906,1.,2.60287635689));
#46722=CARTESIAN_POINT('Ctrl Pts',(-2.72886483481804,-1.,2.5981786903501));
#46723=CARTESIAN_POINT('Ctrl Pts',(-2.72886483481804,1.,2.5981786903501));
#46724=CARTESIAN_POINT('Ctrl Pts',(-2.72378896977273,-1.,2.59399625537407));
#46725=CARTESIAN_POINT('Ctrl Pts',(-2.72378896977273,1.,2.59399625537407));
#46726=CARTESIAN_POINT('Ctrl Pts',(-2.7197430895797,-1.,2.59056604771863));
#46727=CARTESIAN_POINT('Ctrl Pts',(-2.7197430895797,1.,2.59056604771863));
#46728=CARTESIAN_POINT('Ctrl Pts',(-2.71690570241274,-1.,2.58804906785078));
#46729=CARTESIAN_POINT('Ctrl Pts',(-2.71690570241274,1.,2.58804906785078));
#46730=CARTESIAN_POINT('Ctrl Pts',(-2.71566956750046,-1.,2.58682657352212));
#46731=CARTESIAN_POINT('Ctrl Pts',(-2.71566956750046,1.,2.58682657352212));
#46732=CARTESIAN_POINT('Ctrl Pts',(-2.71533674140979,-1.,2.58636629903847));
#46733=CARTESIAN_POINT('Ctrl Pts',(-2.71533674140979,1.,2.58636629903847));
#46734=CARTESIAN_POINT('Ctrl Pts',(-2.71537879705,-1.,2.58626222935706));
#46735=CARTESIAN_POINT('Ctrl Pts',(-2.71537879705,1.,2.58626222935706));
#46736=CARTESIAN_POINT('Ctrl Pts',(-2.71546581445404,-1.,2.58626089374824));
#46737=CARTESIAN_POINT('Ctrl Pts',(-2.71546581445404,1.,2.58626089374824));
#46738=CARTESIAN_POINT('',(-3.14378277984898,1.,2.78507268004356));
#46739=CARTESIAN_POINT('Ctrl Pts',(-3.14378277984898,1.,2.78507268004356));
#46740=CARTESIAN_POINT('Ctrl Pts',(-3.14226401019149,1.,2.78466475036183));
#46741=CARTESIAN_POINT('Ctrl Pts',(-3.13922819750185,1.,2.78384588958965));
#46742=CARTESIAN_POINT('Ctrl Pts',(-3.1346796583452,1.,2.78260859420629));
#46743=CARTESIAN_POINT('Ctrl Pts',(-3.12862530320194,1.,2.78094085162947));
#46744=CARTESIAN_POINT('Ctrl Pts',(-3.12107467038623,1.,2.77882610147986));
#46745=CARTESIAN_POINT('Ctrl Pts',(-3.11354142304692,1.,2.77668121003225));
#46746=CARTESIAN_POINT('Ctrl Pts',(-3.10602568032641,1.,2.7745060912343));
#46747=CARTESIAN_POINT('Ctrl Pts',(-3.09852761277432,1.,2.77230064795679));
#46748=CARTESIAN_POINT('Ctrl Pts',(-3.09104745381882,1.,2.77006478033937));
#46749=CARTESIAN_POINT('Ctrl Pts',(-3.08358548000904,1.,2.76779837828843));
#46750=CARTESIAN_POINT('Ctrl Pts',(-3.07614198408488,1.,2.76550131064522));
#46751=CARTESIAN_POINT('Ctrl Pts',(-3.06871724843121,1.,2.76317341453415));
#46752=CARTESIAN_POINT('Ctrl Pts',(-3.06131152247599,1.,2.76081448760011));
#46753=CARTESIAN_POINT('Ctrl Pts',(-3.05392498750112,1.,2.75842427253164));
#46754=CARTESIAN_POINT('Ctrl Pts',(-3.04655777351333,1.,2.7560024745616));
#46755=CARTESIAN_POINT('Ctrl Pts',(-3.03921001108158,1.,2.75354880060473));
#46756=CARTESIAN_POINT('Ctrl Pts',(-3.03188187589168,1.,2.75106299523032));
#46757=CARTESIAN_POINT('Ctrl Pts',(-3.02457362909199,1.,2.74854487184099));
#46758=CARTESIAN_POINT('Ctrl Pts',(-3.01728567646502,1.,2.74599436193528));
#46759=CARTESIAN_POINT('Ctrl Pts',(-3.01001855960041,1.,2.7434115023978));
#46760=CARTESIAN_POINT('Ctrl Pts',(-3.00277284351431,1.,2.74079632883852));
#46761=CARTESIAN_POINT('Ctrl Pts',(-2.99554902409741,1.,2.73814878711609));
#46762=CARTESIAN_POINT('Ctrl Pts',(-2.98834743696455,1.,2.73546864694548));
#46763=CARTESIAN_POINT('Ctrl Pts',(-2.98116814232175,1.,2.73275539286537));
#46764=CARTESIAN_POINT('Ctrl Pts',(-2.97401089032729,1.,2.7300081921846));
#46765=CARTESIAN_POINT('Ctrl Pts',(-2.96687537842492,1.,2.72722614084112));
#46766=CARTESIAN_POINT('Ctrl Pts',(-2.95976146492595,1.,2.72440846811745));
#46767=CARTESIAN_POINT('Ctrl Pts',(-2.95266939280617,1.,2.72155475123361));
#46768=CARTESIAN_POINT('Ctrl Pts',(-2.94560002559789,1.,2.71866514227952));
#46769=CARTESIAN_POINT('Ctrl Pts',(-2.93855503247248,1.,2.71574054592575));
#46770=CARTESIAN_POINT('Ctrl Pts',(-2.93153633192583,1.,2.71278207520807));
#46771=CARTESIAN_POINT('Ctrl Pts',(-2.92454558914774,1.,2.70979055994751));
#46772=CARTESIAN_POINT('Ctrl Pts',(-2.91758367994738,1.,2.70676602302518));
#46773=CARTESIAN_POINT('Ctrl Pts',(-2.91065019668331,1.,2.70370719782114));
#46774=CARTESIAN_POINT('Ctrl Pts',(-2.90374285605839,1.,2.70061095078692));
#46775=CARTESIAN_POINT('Ctrl Pts',(-2.89685866123668,1.,2.69747340630621));
#46776=CARTESIAN_POINT('Ctrl Pts',(-2.88999512410304,1.,2.69429113011369));
#46777=CARTESIAN_POINT('Ctrl Pts',(-2.88315153980464,1.,2.69106236420197));
#46778=CARTESIAN_POINT('Ctrl Pts',(-2.87633007243885,1.,2.68778807801691));
#46779=CARTESIAN_POINT('Ctrl Pts',(-2.8695373654725,1.,2.68447353139611));
#46780=CARTESIAN_POINT('Ctrl Pts',(-2.86278224277705,1.,2.68112602796323));
#46781=CARTESIAN_POINT('Ctrl Pts',(-2.85607274378031,1.,2.67775201955736));
#46782=CARTESIAN_POINT('Ctrl Pts',(-2.84941315703096,1.,2.67435421039682));
#46783=CARTESIAN_POINT('Ctrl Pts',(-2.84280157191314,1.,2.67092916452117));
#46784=CARTESIAN_POINT('Ctrl Pts',(-2.8362258685396,1.,2.66746339678085));
#46785=CARTESIAN_POINT('Ctrl Pts',(-2.82966813308969,1.,2.66393764726902));
#46786=CARTESIAN_POINT('Ctrl Pts',(-2.82311188135053,1.,2.66033388273437));
#46787=CARTESIAN_POINT('Ctrl Pts',(-2.81654896073874,1.,2.65664198781335));
#46788=CARTESIAN_POINT('Ctrl Pts',(-2.80998526078179,1.,2.65286529532221));
#46789=CARTESIAN_POINT('Ctrl Pts',(-2.80345029781191,1.,2.64902988983373));
#46790=CARTESIAN_POINT('Ctrl Pts',(-2.7969891067079,1.,2.6451766779937));
#46791=CARTESIAN_POINT('Ctrl Pts',(-2.79064495573275,1.,2.64134450532632));
#46792=CARTESIAN_POINT('Ctrl Pts',(-2.78444351041594,1.,2.63755471430322));
#46793=CARTESIAN_POINT('Ctrl Pts',(-2.77837943466423,1.,2.63379800904575));
#46794=CARTESIAN_POINT('Ctrl Pts',(-2.77239433377839,1.,2.63001305229548));
#46795=CARTESIAN_POINT('Ctrl Pts',(-2.76639078478898,1.,2.6260995650624));
#46796=CARTESIAN_POINT('Ctrl Pts',(-2.76027271596564,1.,2.62195665834491));
#46797=CARTESIAN_POINT('Ctrl Pts',(-2.75398025025967,1.,2.61751580407608));
#46798=CARTESIAN_POINT('Ctrl Pts',(-2.74752219567307,1.,2.61277170105864));
#46799=CARTESIAN_POINT('Ctrl Pts',(-2.74102110999284,1.,2.60782480638629));
#46800=CARTESIAN_POINT('Ctrl Pts',(-2.73470730109906,1.,2.60287635689));
#46801=CARTESIAN_POINT('Ctrl Pts',(-2.72886483481804,1.,2.5981786903501));
#46802=CARTESIAN_POINT('Ctrl Pts',(-2.72378896977273,1.,2.59399625537407));
#46803=CARTESIAN_POINT('Ctrl Pts',(-2.7197430895797,1.,2.59056604771863));
#46804=CARTESIAN_POINT('Ctrl Pts',(-2.7171186028189,1.,2.58823792682724));
#46805=CARTESIAN_POINT('Ctrl Pts',(-2.71591054189884,1.,2.58706285424469));
#46806=CARTESIAN_POINT('Ctrl Pts',(-2.71548946460616,1.,2.58656037976884));
#46807=CARTESIAN_POINT('Ctrl Pts',(-2.71540296615967,1.,2.58638312917291));
#46808=CARTESIAN_POINT('Ctrl Pts',(-2.71539546306824,1.,2.58633475775051));
#46809=CARTESIAN_POINT('',(-3.14378277984898,0.,2.78507268004356));
#46810=CARTESIAN_POINT('Ctrl Pts',(-2.97921217251145,-1.,2.27745358485296));
#46811=CARTESIAN_POINT('Ctrl Pts',(-2.97921217251145,1.,2.27745358485296));
#46812=CARTESIAN_POINT('Ctrl Pts',(-2.97919987915679,-1.,2.27736742984319));
#46813=CARTESIAN_POINT('Ctrl Pts',(-2.97919987915679,1.,2.27736742984319));
#46814=CARTESIAN_POINT('Ctrl Pts',(-2.97929608861798,-1.,2.2773096118942));
#46815=CARTESIAN_POINT('Ctrl Pts',(-2.97929608861798,1.,2.2773096118942));
#46816=CARTESIAN_POINT('Ctrl Pts',(-2.97980276183181,-1.,2.27756633755188));
#46817=CARTESIAN_POINT('Ctrl Pts',(-2.97980276183181,1.,2.27756633755188));
#46818=CARTESIAN_POINT('Ctrl Pts',(-2.98120357932994,-1.,2.27859601334547));
#46819=CARTESIAN_POINT('Ctrl Pts',(-2.98120357932994,1.,2.27859601334547));
#46820=CARTESIAN_POINT('Ctrl Pts',(-2.98413343613983,-1.,2.28100472516679));
#46821=CARTESIAN_POINT('Ctrl Pts',(-2.98413343613983,1.,2.28100472516679));
#46822=CARTESIAN_POINT('Ctrl Pts',(-2.9881543273478,-1.,2.28446419115919));
#46823=CARTESIAN_POINT('Ctrl Pts',(-2.9881543273478,1.,2.28446419115919));
#46824=CARTESIAN_POINT('Ctrl Pts',(-2.99307930984034,-1.,2.28882328690362));
#46825=CARTESIAN_POINT('Ctrl Pts',(-2.99307930984034,1.,2.28882328690362));
#46826=CARTESIAN_POINT('Ctrl Pts',(-2.99863310339691,-1.,2.29385894577754));
#46827=CARTESIAN_POINT('Ctrl Pts',(-2.99863310339691,1.,2.29385894577754));
#46828=CARTESIAN_POINT('Ctrl Pts',(-3.00450832658613,-1.,2.29932091315775));
#46829=CARTESIAN_POINT('Ctrl Pts',(-3.00450832658613,1.,2.29932091315775));
#46830=CARTESIAN_POINT('Ctrl Pts',(-3.01041131063823,-1.,2.30496809486482));
#46831=CARTESIAN_POINT('Ctrl Pts',(-3.01041131063823,1.,2.30496809486482));
#46832=CARTESIAN_POINT('Ctrl Pts',(-3.01610726819086,-1.,2.31060449886629));
#46833=CARTESIAN_POINT('Ctrl Pts',(-3.01610726819086,1.,2.31060449886629));
#46834=CARTESIAN_POINT('Ctrl Pts',(-3.02147780668161,-1.,2.31612479121631));
#46835=CARTESIAN_POINT('Ctrl Pts',(-3.02147780668161,1.,2.31612479121631));
#46836=CARTESIAN_POINT('Ctrl Pts',(-3.02652678416611,-1.,2.32151944306402));
#46837=CARTESIAN_POINT('Ctrl Pts',(-3.02652678416611,1.,2.32151944306402));
#46838=CARTESIAN_POINT('Ctrl Pts',(-3.03133125185136,-1.,2.32683687412097));
#46839=CARTESIAN_POINT('Ctrl Pts',(-3.03133125185136,1.,2.32683687412097));
#46840=CARTESIAN_POINT('Ctrl Pts',(-3.03600588555793,-1.,2.33215619079829));
#46841=CARTESIAN_POINT('Ctrl Pts',(-3.03600588555793,1.,2.33215619079829));
#46842=CARTESIAN_POINT('Ctrl Pts',(-3.04066496998544,-1.,2.33755792953706));
#46843=CARTESIAN_POINT('Ctrl Pts',(-3.04066496998544,1.,2.33755792953706));
#46844=CARTESIAN_POINT('Ctrl Pts',(-3.04537822217256,-1.,2.34309017083977));
#46845=CARTESIAN_POINT('Ctrl Pts',(-3.04537822217256,1.,2.34309017083977));
#46846=CARTESIAN_POINT('Ctrl Pts',(-3.05015565829918,-1.,2.34875673090771));
#46847=CARTESIAN_POINT('Ctrl Pts',(-3.05015565829918,1.,2.34875673090771));
#46848=CARTESIAN_POINT('Ctrl Pts',(-3.05497218368146,-1.,2.35453559889474));
#46849=CARTESIAN_POINT('Ctrl Pts',(-3.05497218368146,1.,2.35453559889474));
#46850=CARTESIAN_POINT('Ctrl Pts',(-3.0597826624004,-1.,2.36039011602072));
#46851=CARTESIAN_POINT('Ctrl Pts',(-3.0597826624004,1.,2.36039011602072));
#46852=CARTESIAN_POINT('Ctrl Pts',(-3.06453964643162,-1.,2.36628220107009));
#46853=CARTESIAN_POINT('Ctrl Pts',(-3.06453964643162,1.,2.36628220107009));
#46854=CARTESIAN_POINT('Ctrl Pts',(-3.069212754975,-1.,2.37218678163178));
#46855=CARTESIAN_POINT('Ctrl Pts',(-3.069212754975,1.,2.37218678163178));
#46856=CARTESIAN_POINT('Ctrl Pts',(-3.07379777492165,-1.,2.37809856205548));
#46857=CARTESIAN_POINT('Ctrl Pts',(-3.07379777492165,1.,2.37809856205548));
#46858=CARTESIAN_POINT('Ctrl Pts',(-3.07830597244326,-1.,2.38402401216126));
#46859=CARTESIAN_POINT('Ctrl Pts',(-3.07830597244326,1.,2.38402401216126));
#46860=CARTESIAN_POINT('Ctrl Pts',(-3.08275773747093,-1.,2.38997659219199));
#46861=CARTESIAN_POINT('Ctrl Pts',(-3.08275773747093,1.,2.38997659219199));
#46862=CARTESIAN_POINT('Ctrl Pts',(-3.08717489512914,-1.,2.39597098250631));
#46863=CARTESIAN_POINT('Ctrl Pts',(-3.08717489512914,1.,2.39597098250631));
#46864=CARTESIAN_POINT('Ctrl Pts',(-3.091572660511,-1.,2.40201704423341));
#46865=CARTESIAN_POINT('Ctrl Pts',(-3.091572660511,1.,2.40201704423341));
#46866=CARTESIAN_POINT('Ctrl Pts',(-3.09595472616076,-1.,2.40811612696369));
#46867=CARTESIAN_POINT('Ctrl Pts',(-3.09595472616076,1.,2.40811612696369));
#46868=CARTESIAN_POINT('Ctrl Pts',(-3.1003177502767,-1.,2.41426441798057));
#46869=CARTESIAN_POINT('Ctrl Pts',(-3.1003177502767,1.,2.41426441798057));
#46870=CARTESIAN_POINT('Ctrl Pts',(-3.10465410280896,-1.,2.42045498612489));
#46871=CARTESIAN_POINT('Ctrl Pts',(-3.10465410280896,1.,2.42045498612489));
#46872=CARTESIAN_POINT('Ctrl Pts',(-3.10895518969595,-1.,2.42668025870015));
#46873=CARTESIAN_POINT('Ctrl Pts',(-3.10895518969595,1.,2.42668025870015));
#46874=CARTESIAN_POINT('Ctrl Pts',(-3.11321477659018,-1.,2.43293449685144));
#46875=CARTESIAN_POINT('Ctrl Pts',(-3.11321477659018,1.,2.43293449685144));
#46876=CARTESIAN_POINT('Ctrl Pts',(-3.11743156744186,-1.,2.43921571477977));
#46877=CARTESIAN_POINT('Ctrl Pts',(-3.11743156744186,1.,2.43921571477977));
#46878=CARTESIAN_POINT('Ctrl Pts',(-3.12160740887768,-1.,2.44552433364715));
#46879=CARTESIAN_POINT('Ctrl Pts',(-3.12160740887768,1.,2.44552433364715));
#46880=CARTESIAN_POINT('Ctrl Pts',(-3.12574608210847,-1.,2.45186227369846));
#46881=CARTESIAN_POINT('Ctrl Pts',(-3.12574608210847,1.,2.45186227369846));
#46882=CARTESIAN_POINT('Ctrl Pts',(-3.12985188384371,-1.,2.45823188859366));
#46883=CARTESIAN_POINT('Ctrl Pts',(-3.12985188384371,1.,2.45823188859366));
#46884=CARTESIAN_POINT('Ctrl Pts',(-3.13392826623906,-1.,2.46463494332374));
#46885=CARTESIAN_POINT('Ctrl Pts',(-3.13392826623906,1.,2.46463494332374));
#46886=CARTESIAN_POINT('Ctrl Pts',(-3.13797654408943,-1.,2.47107164236838));
#46887=CARTESIAN_POINT('Ctrl Pts',(-3.13797654408943,1.,2.47107164236838));
#46888=CARTESIAN_POINT('Ctrl Pts',(-3.14199655778863,-1.,2.47754112428043));
#46889=CARTESIAN_POINT('Ctrl Pts',(-3.14199655778863,1.,2.47754112428043));
#46890=CARTESIAN_POINT('Ctrl Pts',(-3.14598722723896,-1.,2.4840418741839));
#46891=CARTESIAN_POINT('Ctrl Pts',(-3.14598722723896,1.,2.4840418741839));
#46892=CARTESIAN_POINT('Ctrl Pts',(-3.14994715298907,-1.,2.49057217131988));
#46893=CARTESIAN_POINT('Ctrl Pts',(-3.14994715298907,1.,2.49057217131988));
#46894=CARTESIAN_POINT('Ctrl Pts',(-3.15387518039046,-1.,2.49713050858896));
#46895=CARTESIAN_POINT('Ctrl Pts',(-3.15387518039046,1.,2.49713050858896));
#46896=CARTESIAN_POINT('Ctrl Pts',(-3.15777102413957,-1.,2.50371605688252));
#46897=CARTESIAN_POINT('Ctrl Pts',(-3.15777102413957,1.,2.50371605688252));
#46898=CARTESIAN_POINT('Ctrl Pts',(-3.16163506380157,-1.,2.51032851007894));
#46899=CARTESIAN_POINT('Ctrl Pts',(-3.16163506380157,1.,2.51032851007894));
#46900=CARTESIAN_POINT('Ctrl Pts',(-3.16546808277023,-1.,2.51696788755577));
#46901=CARTESIAN_POINT('Ctrl Pts',(-3.16546808277023,1.,2.51696788755577));
#46902=CARTESIAN_POINT('Ctrl Pts',(-3.16927102130736,-1.,2.52363434671788));
#46903=CARTESIAN_POINT('Ctrl Pts',(-3.16927102130736,1.,2.52363434671788));
#46904=CARTESIAN_POINT('Ctrl Pts',(-3.17304474093612,-1.,2.53032800406941));
#46905=CARTESIAN_POINT('Ctrl Pts',(-3.17304474093612,1.,2.53032800406941));
#46906=CARTESIAN_POINT('Ctrl Pts',(-3.17678974135318,-1.,2.53704871950948));
#46907=CARTESIAN_POINT('Ctrl Pts',(-3.17678974135318,1.,2.53704871950948));
#46908=CARTESIAN_POINT('Ctrl Pts',(-3.1805061975064,-1.,2.54379612553051));
#46909=CARTESIAN_POINT('Ctrl Pts',(-3.1805061975064,1.,2.54379612553051));
#46910=CARTESIAN_POINT('Ctrl Pts',(-3.18419408529594,-1.,2.55056972387731));
#46911=CARTESIAN_POINT('Ctrl Pts',(-3.18419408529594,1.,2.55056972387731));
#46912=CARTESIAN_POINT('Ctrl Pts',(-3.18785328116218,-1.,2.55736896206056));
#46913=CARTESIAN_POINT('Ctrl Pts',(-3.18785328116218,1.,2.55736896206056));
#46914=CARTESIAN_POINT('Ctrl Pts',(-3.19148366395139,-1.,2.56419331092858));
#46915=CARTESIAN_POINT('Ctrl Pts',(-3.19148366395139,1.,2.56419331092858));
#46916=CARTESIAN_POINT('Ctrl Pts',(-3.19508523784363,-1.,2.57104235897899));
#46917=CARTESIAN_POINT('Ctrl Pts',(-3.19508523784363,1.,2.57104235897899));
#46918=CARTESIAN_POINT('Ctrl Pts',(-3.19865814628682,-1.,2.57791581908875));
#46919=CARTESIAN_POINT('Ctrl Pts',(-3.19865814628682,1.,2.57791581908875));
#46920=CARTESIAN_POINT('Ctrl Pts',(-3.20220261408414,-1.,2.58481347777729));
#46921=CARTESIAN_POINT('Ctrl Pts',(-3.20220261408414,1.,2.58481347777729));
#46922=CARTESIAN_POINT('Ctrl Pts',(-3.2057189102873,-1.,2.59173516023481));
#46923=CARTESIAN_POINT('Ctrl Pts',(-3.2057189102873,1.,2.59173516023481));
#46924=CARTESIAN_POINT('Ctrl Pts',(-3.20920730569681,-1.,2.59868069194342));
#46925=CARTESIAN_POINT('Ctrl Pts',(-3.20920730569681,1.,2.59868069194342));
#46926=CARTESIAN_POINT('Ctrl Pts',(-3.21266802609682,-1.,2.60564985360017));
#46927=CARTESIAN_POINT('Ctrl Pts',(-3.21266802609682,1.,2.60564985360017));
#46928=CARTESIAN_POINT('Ctrl Pts',(-3.21610123233082,-1.,2.61264236719171));
#46929=CARTESIAN_POINT('Ctrl Pts',(-3.21610123233082,1.,2.61264236719171));
#46930=CARTESIAN_POINT('Ctrl Pts',(-3.21950704109321,-1.,2.61965792832947));
#46931=CARTESIAN_POINT('Ctrl Pts',(-3.21950704109321,1.,2.61965792832947));
#46932=CARTESIAN_POINT('Ctrl Pts',(-3.2228855361324,-1.,2.62669622735912));
#46933=CARTESIAN_POINT('Ctrl Pts',(-3.2228855361324,1.,2.62669622735912));
#46934=CARTESIAN_POINT('Ctrl Pts',(-3.2262367829246,-1.,2.63375697391372));
#46935=CARTESIAN_POINT('Ctrl Pts',(-3.2262367829246,1.,2.63375697391372));
#46936=CARTESIAN_POINT('Ctrl Pts',(-3.22956084358547,-1.,2.64083992181823));
#46937=CARTESIAN_POINT('Ctrl Pts',(-3.22956084358547,1.,2.64083992181823));
#46938=CARTESIAN_POINT('Ctrl Pts',(-3.23285778737096,-1.,2.64794488743038));
#46939=CARTESIAN_POINT('Ctrl Pts',(-3.23285778737096,1.,2.64794488743038));
#46940=CARTESIAN_POINT('Ctrl Pts',(-3.236127680639,-1.,2.65507173961555));
#46941=CARTESIAN_POINT('Ctrl Pts',(-3.236127680639,1.,2.65507173961555));
#46942=CARTESIAN_POINT('Ctrl Pts',(-3.23872200034785,-1.,2.6607906631847));
#46943=CARTESIAN_POINT('Ctrl Pts',(-3.23872200034785,1.,2.6607906631847));
#46944=CARTESIAN_POINT('Ctrl Pts',(-3.24065561086749,-1.,2.66508964663997));
#46945=CARTESIAN_POINT('Ctrl Pts',(-3.24065561086749,1.,2.66508964663997));
#46946=CARTESIAN_POINT('Ctrl Pts',(-3.24193929584471,-1.,2.66795998539579));
#46947=CARTESIAN_POINT('Ctrl Pts',(-3.24193929584471,1.,2.66795998539579));
#46948=CARTESIAN_POINT('Ctrl Pts',(-3.24257979115744,-1.,2.66939624221984));
#46949=CARTESIAN_POINT('Ctrl Pts',(-3.24257979115744,1.,2.66939624221984));
#46950=CARTESIAN_POINT('',(-2.97927412174279,1.,2.27737254473521));
#46951=CARTESIAN_POINT('Ctrl Pts',(-2.97927412174279,-1.,2.27737254473521));
#46952=CARTESIAN_POINT('Ctrl Pts',(-2.97927412174279,-0.666666666666667,
2.27737254473521));
#46953=CARTESIAN_POINT('Ctrl Pts',(-2.97927412174279,-0.333333333333333,
2.27737254473521));
#46954=CARTESIAN_POINT('Ctrl Pts',(-2.97927412174279,0.333333333333333,
2.27737254473521));
#46955=CARTESIAN_POINT('Ctrl Pts',(-2.97927412174279,0.666666666666667,
2.27737254473521));
#46956=CARTESIAN_POINT('Ctrl Pts',(-2.97927412174279,1.,2.27737254473521));
#46957=CARTESIAN_POINT('',(-3.24257979115744,1.,2.66939624221984));
#46958=CARTESIAN_POINT('',(-3.24257979115744,0.,2.66939624221984));
#46959=CARTESIAN_POINT('Ctrl Pts',(-2.97927412174279,1.,2.27737254473521));
#46960=CARTESIAN_POINT('Ctrl Pts',(-2.97932307137476,1.,2.27737238849287));
#46961=CARTESIAN_POINT('Ctrl Pts',(-2.9795116710597,1.,2.27743009389684));
#46962=CARTESIAN_POINT('Ctrl Pts',(-2.98007383024207,1.,2.27776738270289));
#46963=CARTESIAN_POINT('Ctrl Pts',(-2.9814234180956,1.,2.27877674853766));
#46964=CARTESIAN_POINT('Ctrl Pts',(-2.98413343613983,1.,2.28100472516679));
#46965=CARTESIAN_POINT('Ctrl Pts',(-2.9881543273478,1.,2.28446419115919));
#46966=CARTESIAN_POINT('Ctrl Pts',(-2.99307930984034,1.,2.28882328690362));
#46967=CARTESIAN_POINT('Ctrl Pts',(-2.99863310339691,1.,2.29385894577754));
#46968=CARTESIAN_POINT('Ctrl Pts',(-3.00450832658613,1.,2.29932091315775));
#46969=CARTESIAN_POINT('Ctrl Pts',(-3.01041131063823,1.,2.30496809486482));
#46970=CARTESIAN_POINT('Ctrl Pts',(-3.01610726819086,1.,2.31060449886629));
#46971=CARTESIAN_POINT('Ctrl Pts',(-3.02147780668161,1.,2.31612479121631));
#46972=CARTESIAN_POINT('Ctrl Pts',(-3.02652678416611,1.,2.32151944306402));
#46973=CARTESIAN_POINT('Ctrl Pts',(-3.03133125185136,1.,2.32683687412097));
#46974=CARTESIAN_POINT('Ctrl Pts',(-3.03600588555793,1.,2.33215619079829));
#46975=CARTESIAN_POINT('Ctrl Pts',(-3.04066496998544,1.,2.33755792953706));
#46976=CARTESIAN_POINT('Ctrl Pts',(-3.04537822217256,1.,2.34309017083977));
#46977=CARTESIAN_POINT('Ctrl Pts',(-3.05015565829918,1.,2.34875673090771));
#46978=CARTESIAN_POINT('Ctrl Pts',(-3.05497218368146,1.,2.35453559889474));
#46979=CARTESIAN_POINT('Ctrl Pts',(-3.0597826624004,1.,2.36039011602072));
#46980=CARTESIAN_POINT('Ctrl Pts',(-3.06453964643162,1.,2.36628220107009));
#46981=CARTESIAN_POINT('Ctrl Pts',(-3.069212754975,1.,2.37218678163178));
#46982=CARTESIAN_POINT('Ctrl Pts',(-3.07379777492165,1.,2.37809856205548));
#46983=CARTESIAN_POINT('Ctrl Pts',(-3.07830597244326,1.,2.38402401216126));
#46984=CARTESIAN_POINT('Ctrl Pts',(-3.08275773747093,1.,2.38997659219199));
#46985=CARTESIAN_POINT('Ctrl Pts',(-3.08717489512914,1.,2.39597098250631));
#46986=CARTESIAN_POINT('Ctrl Pts',(-3.091572660511,1.,2.40201704423341));
#46987=CARTESIAN_POINT('Ctrl Pts',(-3.09595472616076,1.,2.40811612696369));
#46988=CARTESIAN_POINT('Ctrl Pts',(-3.1003177502767,1.,2.41426441798057));
#46989=CARTESIAN_POINT('Ctrl Pts',(-3.10465410280896,1.,2.42045498612489));
#46990=CARTESIAN_POINT('Ctrl Pts',(-3.10895518969595,1.,2.42668025870015));
#46991=CARTESIAN_POINT('Ctrl Pts',(-3.11321477659018,1.,2.43293449685144));
#46992=CARTESIAN_POINT('Ctrl Pts',(-3.11743156744186,1.,2.43921571477977));
#46993=CARTESIAN_POINT('Ctrl Pts',(-3.12160740887768,1.,2.44552433364715));
#46994=CARTESIAN_POINT('Ctrl Pts',(-3.12574608210847,1.,2.45186227369846));
#46995=CARTESIAN_POINT('Ctrl Pts',(-3.12985188384371,1.,2.45823188859366));
#46996=CARTESIAN_POINT('Ctrl Pts',(-3.13392826623906,1.,2.46463494332374));
#46997=CARTESIAN_POINT('Ctrl Pts',(-3.13797654408943,1.,2.47107164236838));
#46998=CARTESIAN_POINT('Ctrl Pts',(-3.14199655778863,1.,2.47754112428043));
#46999=CARTESIAN_POINT('Ctrl Pts',(-3.14598722723896,1.,2.4840418741839));
#47000=CARTESIAN_POINT('Ctrl Pts',(-3.14994715298907,1.,2.49057217131988));
#47001=CARTESIAN_POINT('Ctrl Pts',(-3.15387518039046,1.,2.49713050858896));
#47002=CARTESIAN_POINT('Ctrl Pts',(-3.15777102413957,1.,2.50371605688252));
#47003=CARTESIAN_POINT('Ctrl Pts',(-3.16163506380157,1.,2.51032851007894));
#47004=CARTESIAN_POINT('Ctrl Pts',(-3.16546808277023,1.,2.51696788755577));
#47005=CARTESIAN_POINT('Ctrl Pts',(-3.16927102130736,1.,2.52363434671788));
#47006=CARTESIAN_POINT('Ctrl Pts',(-3.17304474093612,1.,2.53032800406941));
#47007=CARTESIAN_POINT('Ctrl Pts',(-3.17678974135318,1.,2.53704871950948));
#47008=CARTESIAN_POINT('Ctrl Pts',(-3.1805061975064,1.,2.54379612553051));
#47009=CARTESIAN_POINT('Ctrl Pts',(-3.18419408529594,1.,2.55056972387731));
#47010=CARTESIAN_POINT('Ctrl Pts',(-3.18785328116218,1.,2.55736896206056));
#47011=CARTESIAN_POINT('Ctrl Pts',(-3.19148366395139,1.,2.56419331092858));
#47012=CARTESIAN_POINT('Ctrl Pts',(-3.19508523784363,1.,2.57104235897899));
#47013=CARTESIAN_POINT('Ctrl Pts',(-3.19865814628682,1.,2.57791581908875));
#47014=CARTESIAN_POINT('Ctrl Pts',(-3.20220261408414,1.,2.58481347777729));
#47015=CARTESIAN_POINT('Ctrl Pts',(-3.2057189102873,1.,2.59173516023481));
#47016=CARTESIAN_POINT('Ctrl Pts',(-3.20920730569681,1.,2.59868069194342));
#47017=CARTESIAN_POINT('Ctrl Pts',(-3.21266802609682,1.,2.60564985360017));
#47018=CARTESIAN_POINT('Ctrl Pts',(-3.21610123233082,1.,2.61264236719171));
#47019=CARTESIAN_POINT('Ctrl Pts',(-3.21950704109321,1.,2.61965792832947));
#47020=CARTESIAN_POINT('Ctrl Pts',(-3.2228855361324,1.,2.62669622735912));
#47021=CARTESIAN_POINT('Ctrl Pts',(-3.2262367829246,1.,2.63375697391372));
#47022=CARTESIAN_POINT('Ctrl Pts',(-3.22956084358547,1.,2.64083992181823));
#47023=CARTESIAN_POINT('Ctrl Pts',(-3.23285778737096,1.,2.64794488743038));
#47024=CARTESIAN_POINT('Ctrl Pts',(-3.236127680639,1.,2.65507173961555));
#47025=CARTESIAN_POINT('Ctrl Pts',(-3.23872200034785,1.,2.6607906631847));
#47026=CARTESIAN_POINT('Ctrl Pts',(-3.24065561086749,1.,2.66508964663997));
#47027=CARTESIAN_POINT('Ctrl Pts',(-3.24193929584471,1.,2.66795998539579));
#47028=CARTESIAN_POINT('Ctrl Pts',(-3.24257979115744,1.,2.66939624221984));
#47029=CARTESIAN_POINT('Origin',(-3.24257979115744,0.,2.66939624221984));
#47030=CARTESIAN_POINT('',(-3.14378277984898,1.,2.78507268004356));
#47031=CARTESIAN_POINT('Origin',(0.,0.,0.));
#47032=CARTESIAN_POINT('',(-3.08655633322109,1.,2.12971124846838));
#47033=CARTESIAN_POINT('Origin',(0.,1.,0.));
#47034=CARTESIAN_POINT('Ctrl Pts',(-3.08655633322109,1.,2.12971124846838));
#47035=CARTESIAN_POINT('Ctrl Pts',(-3.08655633322109,0.666666666666667,
2.12971124846838));
#47036=CARTESIAN_POINT('Ctrl Pts',(-3.08655633322109,0.333333333333333,
2.12971124846838));
#47037=CARTESIAN_POINT('Ctrl Pts',(-3.08655633322109,-0.333333333333333,
2.12971124846838));
#47038=CARTESIAN_POINT('Ctrl Pts',(-3.08655633322109,-0.666666666666667,
2.12971124846838));
#47039=CARTESIAN_POINT('Ctrl Pts',(-3.08655633322109,-1.,2.12971124846838));
#47040=CARTESIAN_POINT('Ctrl Pts',(-3.54075895182139,-1.,2.25898783642071));
#47041=CARTESIAN_POINT('Ctrl Pts',(-3.54075895182139,1.,2.25898783642071));
#47042=CARTESIAN_POINT('Ctrl Pts',(-3.5391950664771,-1.,2.25882251694918));
#47043=CARTESIAN_POINT('Ctrl Pts',(-3.5391950664771,1.,2.25882251694918));
#47044=CARTESIAN_POINT('Ctrl Pts',(-3.53606853163247,-1.,2.25848864344599));
#47045=CARTESIAN_POINT('Ctrl Pts',(-3.53606853163247,1.,2.25848864344599));
#47046=CARTESIAN_POINT('Ctrl Pts',(-3.53138243689932,-1.,2.25797812951166));
#47047=CARTESIAN_POINT('Ctrl Pts',(-3.53138243689932,1.,2.25797812951166));
#47048=CARTESIAN_POINT('Ctrl Pts',(-3.52514172849666,-1.,2.25727802942141));
#47049=CARTESIAN_POINT('Ctrl Pts',(-3.52514172849666,1.,2.25727802942141));
#47050=CARTESIAN_POINT('Ctrl Pts',(-3.51735323669213,-1.,2.25637049456061));
#47051=CARTESIAN_POINT('Ctrl Pts',(-3.51735323669213,1.,2.25637049456061));
#47052=CARTESIAN_POINT('Ctrl Pts',(-3.50957720118209,-1.,2.25543046980351));
#47053=CARTESIAN_POINT('Ctrl Pts',(-3.50957720118209,1.,2.25543046980351));
#47054=CARTESIAN_POINT('Ctrl Pts',(-3.50181372618058,-1.,2.25445785151923));
#47055=CARTESIAN_POINT('Ctrl Pts',(-3.50181372618058,1.,2.25445785151923));
#47056=CARTESIAN_POINT('Ctrl Pts',(-3.49406296494309,-1.,2.25345251709453));
#47057=CARTESIAN_POINT('Ctrl Pts',(-3.49406296494309,1.,2.25345251709453));
#47058=CARTESIAN_POINT('Ctrl Pts',(-3.48632513240231,-1.,2.25241433138231));
#47059=CARTESIAN_POINT('Ctrl Pts',(-3.48632513240231,1.,2.25241433138231));
#47060=CARTESIAN_POINT('Ctrl Pts',(-3.47860048448015,-1.,2.25134314238258));
#47061=CARTESIAN_POINT('Ctrl Pts',(-3.47860048448015,1.,2.25134314238258));
#47062=CARTESIAN_POINT('Ctrl Pts',(-3.47088928979467,-1.,2.25023877475674));
#47063=CARTESIAN_POINT('Ctrl Pts',(-3.47088928979467,1.,2.25023877475674));
#47064=CARTESIAN_POINT('Ctrl Pts',(-3.46319180177474,-1.,2.24910102345977));
#47065=CARTESIAN_POINT('Ctrl Pts',(-3.46319180177474,1.,2.24910102345977));
#47066=CARTESIAN_POINT('Ctrl Pts',(-3.45550823512213,-1.,2.24792964960874));
#47067=CARTESIAN_POINT('Ctrl Pts',(-3.45550823512213,1.,2.24792964960874));
#47068=CARTESIAN_POINT('Ctrl Pts',(-3.44783872863448,-1.,2.24672437070139));
#47069=CARTESIAN_POINT('Ctrl Pts',(-3.44783872863448,1.,2.24672437070139));
#47070=CARTESIAN_POINT('Ctrl Pts',(-3.44018336460619,-1.,2.24548487526212));
#47071=CARTESIAN_POINT('Ctrl Pts',(-3.44018336460619,1.,2.24548487526212));
#47072=CARTESIAN_POINT('Ctrl Pts',(-3.43254222615007,-1.,2.24421085338856));
#47073=CARTESIAN_POINT('Ctrl Pts',(-3.43254222615007,1.,2.24421085338856));
#47074=CARTESIAN_POINT('Ctrl Pts',(-3.42491544683075,-1.,2.24290202531144));
#47075=CARTESIAN_POINT('Ctrl Pts',(-3.42491544683075,1.,2.24290202531144));
#47076=CARTESIAN_POINT('Ctrl Pts',(-3.41730325539119,-1.,2.24155816587811));
#47077=CARTESIAN_POINT('Ctrl Pts',(-3.41730325539119,1.,2.24155816587811));
#47078=CARTESIAN_POINT('Ctrl Pts',(-3.40970604190205,-1.,2.24017914395211));
#47079=CARTESIAN_POINT('Ctrl Pts',(-3.40970604190205,1.,2.24017914395211));
#47080=CARTESIAN_POINT('Ctrl Pts',(-3.40212434705511,-1.,2.23876491124064));
#47081=CARTESIAN_POINT('Ctrl Pts',(-3.40212434705511,1.,2.23876491124064));
#47082=CARTESIAN_POINT('Ctrl Pts',(-3.39455873448088,-1.,2.23731541452727));
#47083=CARTESIAN_POINT('Ctrl Pts',(-3.39455873448088,1.,2.23731541452727));
#47084=CARTESIAN_POINT('Ctrl Pts',(-3.38700968549522,-1.,2.23583052276281));
#47085=CARTESIAN_POINT('Ctrl Pts',(-3.38700968549522,1.,2.23583052276281));
#47086=CARTESIAN_POINT('Ctrl Pts',(-3.37947749555649,-1.,2.23430995599572));
#47087=CARTESIAN_POINT('Ctrl Pts',(-3.37947749555649,1.,2.23430995599572));
#47088=CARTESIAN_POINT('Ctrl Pts',(-3.37196214349356,-1.,2.23275319569253));
#47089=CARTESIAN_POINT('Ctrl Pts',(-3.37196214349356,1.,2.23275319569253));
#47090=CARTESIAN_POINT('Ctrl Pts',(-3.36446325227908,-1.,2.23115945849777));
#47091=CARTESIAN_POINT('Ctrl Pts',(-3.36446325227908,1.,2.23115945849777));
#47092=CARTESIAN_POINT('Ctrl Pts',(-3.35698038165529,-1.,2.22952789881011));
#47093=CARTESIAN_POINT('Ctrl Pts',(-3.35698038165529,1.,2.22952789881011));
#47094=CARTESIAN_POINT('Ctrl Pts',(-3.34951327111117,-1.,2.22785777756588));
#47095=CARTESIAN_POINT('Ctrl Pts',(-3.34951327111117,1.,2.22785777756588));
#47096=CARTESIAN_POINT('Ctrl Pts',(-3.34206209449371,-1.,2.22614863918044));
#47097=CARTESIAN_POINT('Ctrl Pts',(-3.34206209449371,1.,2.22614863918044));
#47098=CARTESIAN_POINT('Ctrl Pts',(-3.3346277284958,-1.,2.224400498785));
#47099=CARTESIAN_POINT('Ctrl Pts',(-3.3346277284958,1.,2.224400498785));
#47100=CARTESIAN_POINT('Ctrl Pts',(-3.32721196326019,-1.,2.22261398879623));
#47101=CARTESIAN_POINT('Ctrl Pts',(-3.32721196326019,1.,2.22261398879623));
#47102=CARTESIAN_POINT('Ctrl Pts',(-3.31981686778008,-1.,2.22078990842768));
#47103=CARTESIAN_POINT('Ctrl Pts',(-3.31981686778008,1.,2.22078990842768));
#47104=CARTESIAN_POINT('Ctrl Pts',(-3.31244421655662,-1.,2.21892881679083));
#47105=CARTESIAN_POINT('Ctrl Pts',(-3.31244421655662,1.,2.21892881679083));
#47106=CARTESIAN_POINT('Ctrl Pts',(-3.3050948781957,-1.,2.21703059947837));
#47107=CARTESIAN_POINT('Ctrl Pts',(-3.3050948781957,1.,2.21703059947837));
#47108=CARTESIAN_POINT('Ctrl Pts',(-3.29776825193162,-1.,2.21509406923369));
#47109=CARTESIAN_POINT('Ctrl Pts',(-3.29776825193162,1.,2.21509406923369));
#47110=CARTESIAN_POINT('Ctrl Pts',(-3.29046159238344,-1.,2.21311648827391));
#47111=CARTESIAN_POINT('Ctrl Pts',(-3.29046159238344,1.,2.21311648827391));
#47112=CARTESIAN_POINT('Ctrl Pts',(-3.28317133333127,-1.,2.21109449750638));
#47113=CARTESIAN_POINT('Ctrl Pts',(-3.28317133333127,1.,2.21109449750638));
#47114=CARTESIAN_POINT('Ctrl Pts',(-3.27589448005534,-1.,2.20902509417425));
#47115=CARTESIAN_POINT('Ctrl Pts',(-3.27589448005534,1.,2.20902509417425));
#47116=CARTESIAN_POINT('Ctrl Pts',(-3.2686300613678,-1.,2.20690665217741));
#47117=CARTESIAN_POINT('Ctrl Pts',(-3.2686300613678,1.,2.20690665217741));
#47118=CARTESIAN_POINT('Ctrl Pts',(-3.26138036637711,-1.,2.20473979048682));
#47119=CARTESIAN_POINT('Ctrl Pts',(-3.26138036637711,1.,2.20473979048682));
#47120=CARTESIAN_POINT('Ctrl Pts',(-3.25415277957789,-1.,2.20252866491554));
#47121=CARTESIAN_POINT('Ctrl Pts',(-3.25415277957789,1.,2.20252866491554));
#47122=CARTESIAN_POINT('Ctrl Pts',(-3.24695715874356,-1.,2.20027910880993));
#47123=CARTESIAN_POINT('Ctrl Pts',(-3.24695715874356,1.,2.20027910880993));
#47124=CARTESIAN_POINT('Ctrl Pts',(-3.23980245361323,-1.,2.19799623693263));
#47125=CARTESIAN_POINT('Ctrl Pts',(-3.23980245361323,1.,2.19799623693263));
#47126=CARTESIAN_POINT('Ctrl Pts',(-3.23269332296938,-1.,2.19568204933172));
#47127=CARTESIAN_POINT('Ctrl Pts',(-3.23269332296938,1.,2.19568204933172));
#47128=CARTESIAN_POINT('Ctrl Pts',(-3.22562734221636,-1.,2.19333345123531));
#47129=CARTESIAN_POINT('Ctrl Pts',(-3.22562734221636,1.,2.19333345123531));
#47130=CARTESIAN_POINT('Ctrl Pts',(-3.21859043114069,-1.,2.1909390194865));
#47131=CARTESIAN_POINT('Ctrl Pts',(-3.21859043114069,1.,2.1909390194865));
#47132=CARTESIAN_POINT('Ctrl Pts',(-3.21156188355736,-1.,2.18848253363878));
#47133=CARTESIAN_POINT('Ctrl Pts',(-3.21156188355736,1.,2.18848253363878));
#47134=CARTESIAN_POINT('Ctrl Pts',(-3.20452259717947,-1.,2.18594876115914));
#47135=CARTESIAN_POINT('Ctrl Pts',(-3.20452259717947,1.,2.18594876115914));
#47136=CARTESIAN_POINT('Ctrl Pts',(-3.197462937404,-1.,2.18332898656595));
#47137=CARTESIAN_POINT('Ctrl Pts',(-3.197462937404,1.,2.18332898656595));
#47138=CARTESIAN_POINT('Ctrl Pts',(-3.19038924261589,-1.,2.18062558031789));
#47139=CARTESIAN_POINT('Ctrl Pts',(-3.19038924261589,1.,2.18062558031789));
#47140=CARTESIAN_POINT('Ctrl Pts',(-3.18333474627851,-1.,2.17785968847172));
#47141=CARTESIAN_POINT('Ctrl Pts',(-3.18333474627851,1.,2.17785968847172));
#47142=CARTESIAN_POINT('Ctrl Pts',(-3.17635032802584,-1.,2.17506466903736));
#47143=CARTESIAN_POINT('Ctrl Pts',(-3.17635032802584,1.,2.17506466903736));
#47144=CARTESIAN_POINT('Ctrl Pts',(-3.16948480019555,-1.,2.17227212063857));
#47145=CARTESIAN_POINT('Ctrl Pts',(-3.16948480019555,1.,2.17227212063857));
#47146=CARTESIAN_POINT('Ctrl Pts',(-3.16276685102999,-1.,2.16949910801237));
#47147=CARTESIAN_POINT('Ctrl Pts',(-3.16276685102999,1.,2.16949910801237));
#47148=CARTESIAN_POINT('Ctrl Pts',(-3.15618975593627,-1.,2.1667372844767));
#47149=CARTESIAN_POINT('Ctrl Pts',(-3.15618975593627,1.,2.1667372844767));
#47150=CARTESIAN_POINT('Ctrl Pts',(-3.14968624388961,-1.,2.16393520288009));
#47151=CARTESIAN_POINT('Ctrl Pts',(-3.14968624388961,1.,2.16393520288009));
#47152=CARTESIAN_POINT('Ctrl Pts',(-3.14314440426882,-1.,2.16100905914341));
#47153=CARTESIAN_POINT('Ctrl Pts',(-3.14314440426882,1.,2.16100905914341));
#47154=CARTESIAN_POINT('Ctrl Pts',(-3.136453565629,-1.,2.15787423530583));
#47155=CARTESIAN_POINT('Ctrl Pts',(-3.136453565629,1.,2.15787423530583));
#47156=CARTESIAN_POINT('Ctrl Pts',(-3.12954386795575,-1.,2.15447241382872));
#47157=CARTESIAN_POINT('Ctrl Pts',(-3.12954386795575,1.,2.15447241382872));
#47158=CARTESIAN_POINT('Ctrl Pts',(-3.12242318152001,-1.,2.15079698090627));
#47159=CARTESIAN_POINT('Ctrl Pts',(-3.12242318152001,1.,2.15079698090627));
#47160=CARTESIAN_POINT('Ctrl Pts',(-3.11522827017075,-1.,2.1469279845768));
#47161=CARTESIAN_POINT('Ctrl Pts',(-3.11522827017075,1.,2.1469279845768));
#47162=CARTESIAN_POINT('Ctrl Pts',(-3.10821808669189,-1.,2.14302815602195));
#47163=CARTESIAN_POINT('Ctrl Pts',(-3.10821808669189,1.,2.14302815602195));
#47164=CARTESIAN_POINT('Ctrl Pts',(-3.1017126739137,-1.,2.13930228863968));
#47165=CARTESIAN_POINT('Ctrl Pts',(-3.1017126739137,1.,2.13930228863968));
#47166=CARTESIAN_POINT('Ctrl Pts',(-3.09604502421197,-1.,2.13596538661154));
#47167=CARTESIAN_POINT('Ctrl Pts',(-3.09604502421197,1.,2.13596538661154));
#47168=CARTESIAN_POINT('Ctrl Pts',(-3.09151235281832,-1.,2.13321032560805));
#47169=CARTESIAN_POINT('Ctrl Pts',(-3.09151235281832,1.,2.13321032560805));
#47170=CARTESIAN_POINT('Ctrl Pts',(-3.08831615619661,-1.,2.13116819908263));
#47171=CARTESIAN_POINT('Ctrl Pts',(-3.08831615619661,1.,2.13116819908263));
#47172=CARTESIAN_POINT('Ctrl Pts',(-3.08690399991003,-1.,2.1301541297915));
#47173=CARTESIAN_POINT('Ctrl Pts',(-3.08690399991003,1.,2.1301541297915));
#47174=CARTESIAN_POINT('Ctrl Pts',(-3.08650326866821,-1.,2.12975158752197));
#47175=CARTESIAN_POINT('Ctrl Pts',(-3.08650326866821,1.,2.12975158752197));
#47176=CARTESIAN_POINT('Ctrl Pts',(-3.08652852644876,-1.,2.12964222015945));
#47177=CARTESIAN_POINT('Ctrl Pts',(-3.08652852644876,1.,2.12964222015945));
#47178=CARTESIAN_POINT('Ctrl Pts',(-3.08661426358891,-1.,2.12962728847314));
#47179=CARTESIAN_POINT('Ctrl Pts',(-3.08661426358891,1.,2.12962728847314));
#47180=CARTESIAN_POINT('',(-3.54075895182139,1.,2.25898783642071));
#47181=CARTESIAN_POINT('Ctrl Pts',(-3.54075895182139,1.,2.25898783642071));
#47182=CARTESIAN_POINT('Ctrl Pts',(-3.5391950664771,1.,2.25882251694918));
#47183=CARTESIAN_POINT('Ctrl Pts',(-3.53606853163247,1.,2.25848864344599));
#47184=CARTESIAN_POINT('Ctrl Pts',(-3.53138243689932,1.,2.25797812951166));
#47185=CARTESIAN_POINT('Ctrl Pts',(-3.52514172849666,1.,2.25727802942141));
#47186=CARTESIAN_POINT('Ctrl Pts',(-3.51735323669213,1.,2.25637049456061));
#47187=CARTESIAN_POINT('Ctrl Pts',(-3.50957720118209,1.,2.25543046980351));
#47188=CARTESIAN_POINT('Ctrl Pts',(-3.50181372618058,1.,2.25445785151923));
#47189=CARTESIAN_POINT('Ctrl Pts',(-3.49406296494309,1.,2.25345251709453));
#47190=CARTESIAN_POINT('Ctrl Pts',(-3.48632513240231,1.,2.25241433138231));
#47191=CARTESIAN_POINT('Ctrl Pts',(-3.47860048448015,1.,2.25134314238258));
#47192=CARTESIAN_POINT('Ctrl Pts',(-3.47088928979467,1.,2.25023877475674));
#47193=CARTESIAN_POINT('Ctrl Pts',(-3.46319180177474,1.,2.24910102345977));
#47194=CARTESIAN_POINT('Ctrl Pts',(-3.45550823512213,1.,2.24792964960874));
#47195=CARTESIAN_POINT('Ctrl Pts',(-3.44783872863448,1.,2.24672437070139));
#47196=CARTESIAN_POINT('Ctrl Pts',(-3.44018336460619,1.,2.24548487526212));
#47197=CARTESIAN_POINT('Ctrl Pts',(-3.43254222615007,1.,2.24421085338856));
#47198=CARTESIAN_POINT('Ctrl Pts',(-3.42491544683075,1.,2.24290202531144));
#47199=CARTESIAN_POINT('Ctrl Pts',(-3.41730325539119,1.,2.24155816587811));
#47200=CARTESIAN_POINT('Ctrl Pts',(-3.40970604190205,1.,2.24017914395211));
#47201=CARTESIAN_POINT('Ctrl Pts',(-3.40212434705511,1.,2.23876491124064));
#47202=CARTESIAN_POINT('Ctrl Pts',(-3.39455873448088,1.,2.23731541452727));
#47203=CARTESIAN_POINT('Ctrl Pts',(-3.38700968549522,1.,2.23583052276281));
#47204=CARTESIAN_POINT('Ctrl Pts',(-3.37947749555649,1.,2.23430995599572));
#47205=CARTESIAN_POINT('Ctrl Pts',(-3.37196214349356,1.,2.23275319569253));
#47206=CARTESIAN_POINT('Ctrl Pts',(-3.36446325227908,1.,2.23115945849777));
#47207=CARTESIAN_POINT('Ctrl Pts',(-3.35698038165529,1.,2.22952789881011));
#47208=CARTESIAN_POINT('Ctrl Pts',(-3.34951327111117,1.,2.22785777756588));
#47209=CARTESIAN_POINT('Ctrl Pts',(-3.34206209449371,1.,2.22614863918044));
#47210=CARTESIAN_POINT('Ctrl Pts',(-3.3346277284958,1.,2.224400498785));
#47211=CARTESIAN_POINT('Ctrl Pts',(-3.32721196326019,1.,2.22261398879623));
#47212=CARTESIAN_POINT('Ctrl Pts',(-3.31981686778008,1.,2.22078990842768));
#47213=CARTESIAN_POINT('Ctrl Pts',(-3.31244421655662,1.,2.21892881679083));
#47214=CARTESIAN_POINT('Ctrl Pts',(-3.3050948781957,1.,2.21703059947837));
#47215=CARTESIAN_POINT('Ctrl Pts',(-3.29776825193162,1.,2.21509406923369));
#47216=CARTESIAN_POINT('Ctrl Pts',(-3.29046159238344,1.,2.21311648827391));
#47217=CARTESIAN_POINT('Ctrl Pts',(-3.28317133333127,1.,2.21109449750638));
#47218=CARTESIAN_POINT('Ctrl Pts',(-3.27589448005534,1.,2.20902509417425));
#47219=CARTESIAN_POINT('Ctrl Pts',(-3.2686300613678,1.,2.20690665217741));
#47220=CARTESIAN_POINT('Ctrl Pts',(-3.26138036637711,1.,2.20473979048682));
#47221=CARTESIAN_POINT('Ctrl Pts',(-3.25415277957789,1.,2.20252866491554));
#47222=CARTESIAN_POINT('Ctrl Pts',(-3.24695715874356,1.,2.20027910880993));
#47223=CARTESIAN_POINT('Ctrl Pts',(-3.23980245361323,1.,2.19799623693263));
#47224=CARTESIAN_POINT('Ctrl Pts',(-3.23269332296938,1.,2.19568204933172));
#47225=CARTESIAN_POINT('Ctrl Pts',(-3.22562734221636,1.,2.19333345123531));
#47226=CARTESIAN_POINT('Ctrl Pts',(-3.21859043114069,1.,2.1909390194865));
#47227=CARTESIAN_POINT('Ctrl Pts',(-3.21156188355736,1.,2.18848253363878));
#47228=CARTESIAN_POINT('Ctrl Pts',(-3.20452259717947,1.,2.18594876115914));
#47229=CARTESIAN_POINT('Ctrl Pts',(-3.197462937404,1.,2.18332898656595));
#47230=CARTESIAN_POINT('Ctrl Pts',(-3.19038924261589,1.,2.18062558031789));
#47231=CARTESIAN_POINT('Ctrl Pts',(-3.18333474627851,1.,2.17785968847172));
#47232=CARTESIAN_POINT('Ctrl Pts',(-3.17635032802584,1.,2.17506466903736));
#47233=CARTESIAN_POINT('Ctrl Pts',(-3.16948480019555,1.,2.17227212063857));
#47234=CARTESIAN_POINT('Ctrl Pts',(-3.16276685102999,1.,2.16949910801237));
#47235=CARTESIAN_POINT('Ctrl Pts',(-3.15618975593627,1.,2.1667372844767));
#47236=CARTESIAN_POINT('Ctrl Pts',(-3.14968624388961,1.,2.16393520288009));
#47237=CARTESIAN_POINT('Ctrl Pts',(-3.14314440426882,1.,2.16100905914341));
#47238=CARTESIAN_POINT('Ctrl Pts',(-3.136453565629,1.,2.15787423530583));
#47239=CARTESIAN_POINT('Ctrl Pts',(-3.12954386795575,1.,2.15447241382872));
#47240=CARTESIAN_POINT('Ctrl Pts',(-3.12242318152001,1.,2.15079698090627));
#47241=CARTESIAN_POINT('Ctrl Pts',(-3.11522827017075,1.,2.1469279845768));
#47242=CARTESIAN_POINT('Ctrl Pts',(-3.10821808669189,1.,2.14302815602195));
#47243=CARTESIAN_POINT('Ctrl Pts',(-3.1017126739137,1.,2.13930228863968));
#47244=CARTESIAN_POINT('Ctrl Pts',(-3.09604502421197,1.,2.13596538661154));
#47245=CARTESIAN_POINT('Ctrl Pts',(-3.09151235281832,1.,2.13321032560805));
#47246=CARTESIAN_POINT('Ctrl Pts',(-3.08855597949844,1.,2.13132142793056));
#47247=CARTESIAN_POINT('Ctrl Pts',(-3.08717896996213,1.,2.13034980480519));
#47248=CARTESIAN_POINT('Ctrl Pts',(-3.08668447250383,1.,2.12991938762497));
#47249=CARTESIAN_POINT('Ctrl Pts',(-3.0865713108946,1.,2.1297578506162));
#47250=CARTESIAN_POINT('Ctrl Pts',(-3.0865563332211,1.,2.12971124846838));
#47251=CARTESIAN_POINT('',(-3.54075895182139,0.,2.25898783642071));
#47252=CARTESIAN_POINT('Ctrl Pts',(-3.2988053601491,-1.,1.7833628895577));
#47253=CARTESIAN_POINT('Ctrl Pts',(-3.2988053601491,1.,1.7833628895577));
#47254=CARTESIAN_POINT('Ctrl Pts',(-3.29877974053316,-1.,1.78327971836342));
#47255=CARTESIAN_POINT('Ctrl Pts',(-3.29877974053316,1.,1.78327971836342));
#47256=CARTESIAN_POINT('Ctrl Pts',(-3.29886572077632,-1.,1.78320756177373));
#47257=CARTESIAN_POINT('Ctrl Pts',(-3.29886572077632,1.,1.78320756177373));
#47258=CARTESIAN_POINT('Ctrl Pts',(-3.29940631674303,-1.,1.7833818655594));
#47259=CARTESIAN_POINT('Ctrl Pts',(-3.29940631674303,1.,1.7833818655594));
#47260=CARTESIAN_POINT('Ctrl Pts',(-3.30095096463517,-1.,1.78417972819938));
#47261=CARTESIAN_POINT('Ctrl Pts',(-3.30095096463517,1.,1.78417972819938));
#47262=CARTESIAN_POINT('Ctrl Pts',(-3.30422155559112,-1.,1.78610045419846));
#47263=CARTESIAN_POINT('Ctrl Pts',(-3.30422155559112,1.,1.78610045419846));
#47264=CARTESIAN_POINT('Ctrl Pts',(-3.30873412266788,-1.,1.78888832245873));
#47265=CARTESIAN_POINT('Ctrl Pts',(-3.30873412266788,1.,1.78888832245873));
#47266=CARTESIAN_POINT('Ctrl Pts',(-3.31428038326424,-1.,1.79242331349949));
#47267=CARTESIAN_POINT('Ctrl Pts',(-3.31428038326424,1.,1.79242331349949));
#47268=CARTESIAN_POINT('Ctrl Pts',(-3.3205535510082,-1.,1.79652817033251));
#47269=CARTESIAN_POINT('Ctrl Pts',(-3.3205535510082,1.,1.79652817033251));
#47270=CARTESIAN_POINT('Ctrl Pts',(-3.32721088039578,-1.,1.80100380443406));
#47271=CARTESIAN_POINT('Ctrl Pts',(-3.32721088039578,1.,1.80100380443406));
#47272=CARTESIAN_POINT('Ctrl Pts',(-3.33392460276808,-1.,1.80565802981102));
#47273=CARTESIAN_POINT('Ctrl Pts',(-3.33392460276808,1.,1.80565802981102));
#47274=CARTESIAN_POINT('Ctrl Pts',(-3.34043216147606,-1.,1.81033399625352));
#47275=CARTESIAN_POINT('Ctrl Pts',(-3.34043216147606,1.,1.81033399625352));
#47276=CARTESIAN_POINT('Ctrl Pts',(-3.34660014370673,-1.,1.81494618732853));
#47277=CARTESIAN_POINT('Ctrl Pts',(-3.34660014370673,1.,1.81494618732853));
#47278=CARTESIAN_POINT('Ctrl Pts',(-3.35243086937598,-1.,1.81948458796829));
#47279=CARTESIAN_POINT('Ctrl Pts',(-3.35243086937598,1.,1.81948458796829));
#47280=CARTESIAN_POINT('Ctrl Pts',(-3.35800801557424,-1.,1.82398496829301));
#47281=CARTESIAN_POINT('Ctrl Pts',(-3.35800801557424,1.,1.82398496829301));
#47282=CARTESIAN_POINT('Ctrl Pts',(-3.36345722124158,-1.,1.82850752153199));
#47283=CARTESIAN_POINT('Ctrl Pts',(-3.36345722124158,1.,1.82850752153199));
#47284=CARTESIAN_POINT('Ctrl Pts',(-3.36890396271836,-1.,1.83311391452322));
#47285=CARTESIAN_POINT('Ctrl Pts',(-3.36890396271836,1.,1.83311391452322));
#47286=CARTESIAN_POINT('Ctrl Pts',(-3.37442462015853,-1.,1.83784072967077));
#47287=CARTESIAN_POINT('Ctrl Pts',(-3.37442462015853,1.,1.83784072967077));
#47288=CARTESIAN_POINT('Ctrl Pts',(-3.38002968341157,-1.,1.84269016931643));
#47289=CARTESIAN_POINT('Ctrl Pts',(-3.38002968341157,1.,1.84269016931643));
#47290=CARTESIAN_POINT('Ctrl Pts',(-3.38569092349592,-1.,1.84764441927753));
#47291=CARTESIAN_POINT('Ctrl Pts',(-3.38569092349592,1.,1.84764441927753));
#47292=CARTESIAN_POINT('Ctrl Pts',(-3.39135802549398,-1.,1.85267433291769));
#47293=CARTESIAN_POINT('Ctrl Pts',(-3.39135802549398,1.,1.85267433291769));
#47294=CARTESIAN_POINT('Ctrl Pts',(-3.39697816833067,-1.,1.85774972037062));
#47295=CARTESIAN_POINT('Ctrl Pts',(-3.39697816833067,1.,1.85774972037062));
#47296=CARTESIAN_POINT('Ctrl Pts',(-3.40251742305476,-1.,1.86285057051245));
#47297=CARTESIAN_POINT('Ctrl Pts',(-3.40251742305476,1.,1.86285057051245));
#47298=CARTESIAN_POINT('Ctrl Pts',(-3.40797080000549,-1.,1.86797231196654));
#47299=CARTESIAN_POINT('Ctrl Pts',(-3.40797080000549,1.,1.86797231196654));
#47300=CARTESIAN_POINT('Ctrl Pts',(-3.41335043875209,-1.,1.87311957248121));
#47301=CARTESIAN_POINT('Ctrl Pts',(-3.41335043875209,1.,1.87311957248121));
#47302=CARTESIAN_POINT('Ctrl Pts',(-3.41867858383771,-1.,1.87830245689344));
#47303=CARTESIAN_POINT('Ctrl Pts',(-3.41867858383771,1.,1.87830245689344));
#47304=CARTESIAN_POINT('Ctrl Pts',(-3.42397908819736,-1.,1.8835320506206));
#47305=CARTESIAN_POINT('Ctrl Pts',(-3.42397908819736,1.,1.8835320506206));
#47306=CARTESIAN_POINT('Ctrl Pts',(-3.42926852222158,-1.,1.88881571322009));
#47307=CARTESIAN_POINT('Ctrl Pts',(-3.42926852222158,1.,1.88881571322009));
#47308=CARTESIAN_POINT('Ctrl Pts',(-3.43455074411571,-1.,1.89415420002542));
#47309=CARTESIAN_POINT('Ctrl Pts',(-3.43455074411571,1.,1.89415420002542));
#47310=CARTESIAN_POINT('Ctrl Pts',(-3.4398218567809,-1.,1.89954426803384));
#47311=CARTESIAN_POINT('Ctrl Pts',(-3.4398218567809,1.,1.89954426803384));
#47312=CARTESIAN_POINT('Ctrl Pts',(-3.44507323983367,-1.,1.90498026502304));
#47313=CARTESIAN_POINT('Ctrl Pts',(-3.44507323983367,1.,1.90498026502304));
#47314=CARTESIAN_POINT('Ctrl Pts',(-3.45029522038888,-1.,1.91045605593639));
#47315=CARTESIAN_POINT('Ctrl Pts',(-3.45029522038888,1.,1.91045605593639));
#47316=CARTESIAN_POINT('Ctrl Pts',(-3.4554807430995,-1.,1.91596694784063));
#47317=CARTESIAN_POINT('Ctrl Pts',(-3.4554807430995,1.,1.91596694784063));
#47318=CARTESIAN_POINT('Ctrl Pts',(-3.46062821722485,-1.,1.92151118213212));
#47319=CARTESIAN_POINT('Ctrl Pts',(-3.46062821722485,1.,1.92151118213212));
#47320=CARTESIAN_POINT('Ctrl Pts',(-3.46573953254084,-1.,1.92708888591158));
#47321=CARTESIAN_POINT('Ctrl Pts',(-3.46573953254084,1.,1.92708888591158));
#47322=CARTESIAN_POINT('Ctrl Pts',(-3.47081872409781,-1.,1.93270136427081));
#47323=CARTESIAN_POINT('Ctrl Pts',(-3.47081872409781,1.,1.93270136427081));
#47324=CARTESIAN_POINT('Ctrl Pts',(-3.47587040389915,-1.,1.93835026973887));
#47325=CARTESIAN_POINT('Ctrl Pts',(-3.47587040389915,1.,1.93835026973887));
#47326=CARTESIAN_POINT('Ctrl Pts',(-3.48089825770416,-1.,1.94403680554065));
#47327=CARTESIAN_POINT('Ctrl Pts',(-3.48089825770416,1.,1.94403680554065));
#47328=CARTESIAN_POINT('Ctrl Pts',(-3.48590361610814,-1.,1.94976096795911));
#47329=CARTESIAN_POINT('Ctrl Pts',(-3.48590361610814,1.,1.94976096795911));
#47330=CARTESIAN_POINT('Ctrl Pts',(-3.49088618670987,-1.,1.95552193112084));
#47331=CARTESIAN_POINT('Ctrl Pts',(-3.49088618670987,1.,1.95552193112084));
#47332=CARTESIAN_POINT('Ctrl Pts',(-3.49584466573064,-1.,1.961318367765));
#47333=CARTESIAN_POINT('Ctrl Pts',(-3.49584466573064,1.,1.961318367765));
#47334=CARTESIAN_POINT('Ctrl Pts',(-3.50077740176267,-1.,1.96714879724052));
#47335=CARTESIAN_POINT('Ctrl Pts',(-3.50077740176267,1.,1.96714879724052));
#47336=CARTESIAN_POINT('Ctrl Pts',(-3.5056830186108,-1.,1.97301191162968));
#47337=CARTESIAN_POINT('Ctrl Pts',(-3.5056830186108,1.,1.97301191162968));
#47338=CARTESIAN_POINT('Ctrl Pts',(-3.51056110478287,-1.,1.97890693666288));
#47339=CARTESIAN_POINT('Ctrl Pts',(-3.51056110478287,1.,1.97890693666288));
#47340=CARTESIAN_POINT('Ctrl Pts',(-3.51541198728301,-1.,1.9848335106103));
#47341=CARTESIAN_POINT('Ctrl Pts',(-3.51541198728301,1.,1.9848335106103));
#47342=CARTESIAN_POINT('Ctrl Pts',(-3.52023644289142,-1.,1.99079153006112));
#47343=CARTESIAN_POINT('Ctrl Pts',(-3.52023644289142,1.,1.99079153006112));
#47344=CARTESIAN_POINT('Ctrl Pts',(-3.52503542491728,-1.,1.99678100339295));
#47345=CARTESIAN_POINT('Ctrl Pts',(-3.52503542491728,1.,1.99678100339295));
#47346=CARTESIAN_POINT('Ctrl Pts',(-3.52980980250224,-1.,2.00280191090366));
#47347=CARTESIAN_POINT('Ctrl Pts',(-3.52980980250224,1.,2.00280191090366));
#47348=CARTESIAN_POINT('Ctrl Pts',(-3.53456004727424,-1.,2.00885403604746));
#47349=CARTESIAN_POINT('Ctrl Pts',(-3.53456004727424,1.,2.00885403604746));
#47350=CARTESIAN_POINT('Ctrl Pts',(-3.53928627453642,-1.,2.01493698847351));
#47351=CARTESIAN_POINT('Ctrl Pts',(-3.53928627453642,1.,2.01493698847351));
#47352=CARTESIAN_POINT('Ctrl Pts',(-3.54398838254136,-1.,2.02105027983104));
#47353=CARTESIAN_POINT('Ctrl Pts',(-3.54398838254136,1.,2.02105027983104));
#47354=CARTESIAN_POINT('Ctrl Pts',(-3.54866616282227,-1.,2.02719338376175));
#47355=CARTESIAN_POINT('Ctrl Pts',(-3.54866616282227,1.,2.02719338376175));
#47356=CARTESIAN_POINT('Ctrl Pts',(-3.55331941293949,-1.,2.03336579658133));
#47357=CARTESIAN_POINT('Ctrl Pts',(-3.55331941293949,1.,2.03336579658133));
#47358=CARTESIAN_POINT('Ctrl Pts',(-3.55794807264844,-1.,2.03956711119976));
#47359=CARTESIAN_POINT('Ctrl Pts',(-3.55794807264844,1.,2.03956711119976));
#47360=CARTESIAN_POINT('Ctrl Pts',(-3.56255223871505,-1.,2.04579702158876));
#47361=CARTESIAN_POINT('Ctrl Pts',(-3.56255223871505,1.,2.04579702158876));
#47362=CARTESIAN_POINT('Ctrl Pts',(-3.56713209977904,-1.,2.05205528172911));
#47363=CARTESIAN_POINT('Ctrl Pts',(-3.56713209977904,1.,2.05205528172911));
#47364=CARTESIAN_POINT('Ctrl Pts',(-3.5716878942334,-1.,2.05834167687425));
#47365=CARTESIAN_POINT('Ctrl Pts',(-3.5716878942334,1.,2.05834167687425));
#47366=CARTESIAN_POINT('Ctrl Pts',(-3.57621986224402,-1.,2.06465599229234));
#47367=CARTESIAN_POINT('Ctrl Pts',(-3.57621986224402,1.,2.06465599229234));
#47368=CARTESIAN_POINT('Ctrl Pts',(-3.58072819250872,-1.,2.07099797606));
#47369=CARTESIAN_POINT('Ctrl Pts',(-3.58072819250872,1.,2.07099797606));
#47370=CARTESIAN_POINT('Ctrl Pts',(-3.58521300039988,-1.,2.07736732842524));
#47371=CARTESIAN_POINT('Ctrl Pts',(-3.58521300039988,1.,2.07736732842524));
#47372=CARTESIAN_POINT('Ctrl Pts',(-3.58967435355834,-1.,2.08376373049196));
#47373=CARTESIAN_POINT('Ctrl Pts',(-3.58967435355834,1.,2.08376373049196));
#47374=CARTESIAN_POINT('Ctrl Pts',(-3.5941122862608,-1.,2.09018686331706));
#47375=CARTESIAN_POINT('Ctrl Pts',(-3.5941122862608,1.,2.09018686331706));
#47376=CARTESIAN_POINT('Ctrl Pts',(-3.59852681775396,-1.,2.09663642986579));
#47377=CARTESIAN_POINT('Ctrl Pts',(-3.59852681775396,1.,2.09663642986579));
#47378=CARTESIAN_POINT('Ctrl Pts',(-3.60291797087849,-1.,2.10311217727687));
#47379=CARTESIAN_POINT('Ctrl Pts',(-3.60291797087849,1.,2.10311217727687));
#47380=CARTESIAN_POINT('Ctrl Pts',(-3.60728578530968,-1.,2.10961391333497));
#47381=CARTESIAN_POINT('Ctrl Pts',(-3.60728578530968,1.,2.10961391333497));
#47382=CARTESIAN_POINT('Ctrl Pts',(-3.61163030607452,-1.,2.11614149813928));
#47383=CARTESIAN_POINT('Ctrl Pts',(-3.61163030607452,1.,2.11614149813928));
#47384=CARTESIAN_POINT('Ctrl Pts',(-3.61508732215187,-1.,2.12138417125349));
#47385=CARTESIAN_POINT('Ctrl Pts',(-3.61508732215187,1.,2.12138417125349));
#47386=CARTESIAN_POINT('Ctrl Pts',(-3.61766963589442,-1.,2.12532774376144));
#47387=CARTESIAN_POINT('Ctrl Pts',(-3.61766963589442,1.,2.12532774376144));
#47388=CARTESIAN_POINT('Ctrl Pts',(-3.61938653648716,-1.,2.12796193131142));
#47389=CARTESIAN_POINT('Ctrl Pts',(-3.61938653648716,1.,2.12796193131142));
#47390=CARTESIAN_POINT('Ctrl Pts',(-3.62024382630768,-1.,2.12928030988903));
#47391=CARTESIAN_POINT('Ctrl Pts',(-3.62024382630768,1.,2.12928030988903));
#47392=CARTESIAN_POINT('',(-3.29885386921513,1.,1.78327315618341));
#47393=CARTESIAN_POINT('Ctrl Pts',(-3.29885386921513,-1.,1.78327315618341));
#47394=CARTESIAN_POINT('Ctrl Pts',(-3.29885386921513,-0.666666666666667,
1.78327315618341));
#47395=CARTESIAN_POINT('Ctrl Pts',(-3.29885386921513,-0.333333333333333,
1.78327315618341));
#47396=CARTESIAN_POINT('Ctrl Pts',(-3.29885386921513,0.333333333333333,
1.78327315618341));
#47397=CARTESIAN_POINT('Ctrl Pts',(-3.29885386921513,0.666666666666667,
1.78327315618341));
#47398=CARTESIAN_POINT('Ctrl Pts',(-3.29885386921513,1.,1.78327315618341));
#47399=CARTESIAN_POINT('',(-3.62024382630768,1.,2.12928030988903));
#47400=CARTESIAN_POINT('',(-3.62024382630768,0.,2.12928030988903));
#47401=CARTESIAN_POINT('Ctrl Pts',(-3.29885386921513,1.,1.78327315618341));
#47402=CARTESIAN_POINT('Ctrl Pts',(-3.29890219175423,1.,1.78326534445518));
#47403=CARTESIAN_POINT('Ctrl Pts',(-3.29909749657808,1.,1.78329283591905));
#47404=CARTESIAN_POINT('Ctrl Pts',(-3.299705498242,1.,1.78353803106924));
#47405=CARTESIAN_POINT('Ctrl Pts',(-3.30119637003393,1.,1.78432384788174));
#47406=CARTESIAN_POINT('Ctrl Pts',(-3.30422155559112,1.,1.78610045419846));
#47407=CARTESIAN_POINT('Ctrl Pts',(-3.30873412266788,1.,1.78888832245873));
#47408=CARTESIAN_POINT('Ctrl Pts',(-3.31428038326424,1.,1.79242331349949));
#47409=CARTESIAN_POINT('Ctrl Pts',(-3.3205535510082,1.,1.79652817033251));
#47410=CARTESIAN_POINT('Ctrl Pts',(-3.32721088039578,1.,1.80100380443406));
#47411=CARTESIAN_POINT('Ctrl Pts',(-3.33392460276808,1.,1.80565802981102));
#47412=CARTESIAN_POINT('Ctrl Pts',(-3.34043216147606,1.,1.81033399625352));
#47413=CARTESIAN_POINT('Ctrl Pts',(-3.34660014370673,1.,1.81494618732853));
#47414=CARTESIAN_POINT('Ctrl Pts',(-3.35243086937598,1.,1.81948458796829));
#47415=CARTESIAN_POINT('Ctrl Pts',(-3.35800801557424,1.,1.82398496829301));
#47416=CARTESIAN_POINT('Ctrl Pts',(-3.36345722124158,1.,1.82850752153199));
#47417=CARTESIAN_POINT('Ctrl Pts',(-3.36890396271836,1.,1.83311391452322));
#47418=CARTESIAN_POINT('Ctrl Pts',(-3.37442462015853,1.,1.83784072967077));
#47419=CARTESIAN_POINT('Ctrl Pts',(-3.38002968341157,1.,1.84269016931643));
#47420=CARTESIAN_POINT('Ctrl Pts',(-3.38569092349592,1.,1.84764441927753));
#47421=CARTESIAN_POINT('Ctrl Pts',(-3.39135802549398,1.,1.85267433291769));
#47422=CARTESIAN_POINT('Ctrl Pts',(-3.39697816833067,1.,1.85774972037062));
#47423=CARTESIAN_POINT('Ctrl Pts',(-3.40251742305476,1.,1.86285057051245));
#47424=CARTESIAN_POINT('Ctrl Pts',(-3.40797080000549,1.,1.86797231196654));
#47425=CARTESIAN_POINT('Ctrl Pts',(-3.41335043875209,1.,1.87311957248121));
#47426=CARTESIAN_POINT('Ctrl Pts',(-3.41867858383771,1.,1.87830245689344));
#47427=CARTESIAN_POINT('Ctrl Pts',(-3.42397908819736,1.,1.8835320506206));
#47428=CARTESIAN_POINT('Ctrl Pts',(-3.42926852222158,1.,1.88881571322009));
#47429=CARTESIAN_POINT('Ctrl Pts',(-3.43455074411571,1.,1.89415420002542));
#47430=CARTESIAN_POINT('Ctrl Pts',(-3.4398218567809,1.,1.89954426803384));
#47431=CARTESIAN_POINT('Ctrl Pts',(-3.44507323983367,1.,1.90498026502304));
#47432=CARTESIAN_POINT('Ctrl Pts',(-3.45029522038888,1.,1.91045605593639));
#47433=CARTESIAN_POINT('Ctrl Pts',(-3.4554807430995,1.,1.91596694784063));
#47434=CARTESIAN_POINT('Ctrl Pts',(-3.46062821722485,1.,1.92151118213212));
#47435=CARTESIAN_POINT('Ctrl Pts',(-3.46573953254084,1.,1.92708888591158));
#47436=CARTESIAN_POINT('Ctrl Pts',(-3.47081872409781,1.,1.93270136427081));
#47437=CARTESIAN_POINT('Ctrl Pts',(-3.47587040389915,1.,1.93835026973887));
#47438=CARTESIAN_POINT('Ctrl Pts',(-3.48089825770416,1.,1.94403680554065));
#47439=CARTESIAN_POINT('Ctrl Pts',(-3.48590361610814,1.,1.94976096795911));
#47440=CARTESIAN_POINT('Ctrl Pts',(-3.49088618670987,1.,1.95552193112084));
#47441=CARTESIAN_POINT('Ctrl Pts',(-3.49584466573064,1.,1.961318367765));
#47442=CARTESIAN_POINT('Ctrl Pts',(-3.50077740176267,1.,1.96714879724052));
#47443=CARTESIAN_POINT('Ctrl Pts',(-3.5056830186108,1.,1.97301191162968));
#47444=CARTESIAN_POINT('Ctrl Pts',(-3.51056110478287,1.,1.97890693666288));
#47445=CARTESIAN_POINT('Ctrl Pts',(-3.51541198728301,1.,1.9848335106103));
#47446=CARTESIAN_POINT('Ctrl Pts',(-3.52023644289142,1.,1.99079153006112));
#47447=CARTESIAN_POINT('Ctrl Pts',(-3.52503542491728,1.,1.99678100339295));
#47448=CARTESIAN_POINT('Ctrl Pts',(-3.52980980250224,1.,2.00280191090366));
#47449=CARTESIAN_POINT('Ctrl Pts',(-3.53456004727424,1.,2.00885403604746));
#47450=CARTESIAN_POINT('Ctrl Pts',(-3.53928627453642,1.,2.01493698847351));
#47451=CARTESIAN_POINT('Ctrl Pts',(-3.54398838254136,1.,2.02105027983104));
#47452=CARTESIAN_POINT('Ctrl Pts',(-3.54866616282227,1.,2.02719338376175));
#47453=CARTESIAN_POINT('Ctrl Pts',(-3.55331941293949,1.,2.03336579658133));
#47454=CARTESIAN_POINT('Ctrl Pts',(-3.55794807264844,1.,2.03956711119976));
#47455=CARTESIAN_POINT('Ctrl Pts',(-3.56255223871505,1.,2.04579702158876));
#47456=CARTESIAN_POINT('Ctrl Pts',(-3.56713209977904,1.,2.05205528172911));
#47457=CARTESIAN_POINT('Ctrl Pts',(-3.5716878942334,1.,2.05834167687425));
#47458=CARTESIAN_POINT('Ctrl Pts',(-3.57621986224402,1.,2.06465599229234));
#47459=CARTESIAN_POINT('Ctrl Pts',(-3.58072819250872,1.,2.07099797606));
#47460=CARTESIAN_POINT('Ctrl Pts',(-3.58521300039988,1.,2.07736732842524));
#47461=CARTESIAN_POINT('Ctrl Pts',(-3.58967435355834,1.,2.08376373049196));
#47462=CARTESIAN_POINT('Ctrl Pts',(-3.5941122862608,1.,2.09018686331706));
#47463=CARTESIAN_POINT('Ctrl Pts',(-3.59852681775396,1.,2.09663642986579));
#47464=CARTESIAN_POINT('Ctrl Pts',(-3.60291797087849,1.,2.10311217727687));
#47465=CARTESIAN_POINT('Ctrl Pts',(-3.60728578530968,1.,2.10961391333497));
#47466=CARTESIAN_POINT('Ctrl Pts',(-3.61163030607452,1.,2.11614149813928));
#47467=CARTESIAN_POINT('Ctrl Pts',(-3.61508732215187,1.,2.12138417125349));
#47468=CARTESIAN_POINT('Ctrl Pts',(-3.61766963589442,1.,2.12532774376144));
#47469=CARTESIAN_POINT('Ctrl Pts',(-3.61938653648716,1.,2.12796193131142));
#47470=CARTESIAN_POINT('Ctrl Pts',(-3.62024382630768,1.,2.12928030988903));
#47471=CARTESIAN_POINT('Origin',(-3.62024382630768,0.,2.12928030988903));
#47472=CARTESIAN_POINT('',(-3.54075895182139,1.,2.25898783642071));
#47473=CARTESIAN_POINT('Origin',(0.,0.,0.));
#47474=CARTESIAN_POINT('',(-3.38171594275687,1.,1.62064718014256));
#47475=CARTESIAN_POINT('Origin',(0.,1.,0.));
#47476=CARTESIAN_POINT('Ctrl Pts',(-3.38171594275687,1.,1.62064718014256));
#47477=CARTESIAN_POINT('Ctrl Pts',(-3.38171594275687,0.666666666666667,
1.62064718014256));
#47478=CARTESIAN_POINT('Ctrl Pts',(-3.38171594275687,0.333333333333333,
1.62064718014256));
#47479=CARTESIAN_POINT('Ctrl Pts',(-3.38171594275687,-0.333333333333333,
1.62064718014256));
#47480=CARTESIAN_POINT('Ctrl Pts',(-3.38171594275687,-0.666666666666667,
1.62064718014256));
#47481=CARTESIAN_POINT('Ctrl Pts',(-3.38171594275687,-1.,1.62064718014256));
#47482=CARTESIAN_POINT('Ctrl Pts',(-3.85054988729471,-1.,1.67727921511438));
#47483=CARTESIAN_POINT('Ctrl Pts',(-3.85054988729471,1.,1.67727921511438));
#47484=CARTESIAN_POINT('Ctrl Pts',(-3.84897939431104,-1.,1.6773605765671));
#47485=CARTESIAN_POINT('Ctrl Pts',(-3.84897939431104,1.,1.6773605765671));
#47486=CARTESIAN_POINT('Ctrl Pts',(-3.84583912297567,-1.,1.67751991140661));
#47487=CARTESIAN_POINT('Ctrl Pts',(-3.84583912297567,1.,1.67751991140661));
#47488=CARTESIAN_POINT('Ctrl Pts',(-3.8411308598706,-1.,1.67774874946867));
#47489=CARTESIAN_POINT('Ctrl Pts',(-3.8411308598706,1.,1.67774874946867));
#47490=CARTESIAN_POINT('Ctrl Pts',(-3.83485746516115,-1.,1.67803353065273));
#47491=CARTESIAN_POINT('Ctrl Pts',(-3.83485746516115,1.,1.67803353065273));
#47492=CARTESIAN_POINT('Ctrl Pts',(-3.82702289288453,-1.,1.67835555760094));
#47493=CARTESIAN_POINT('Ctrl Pts',(-3.82702289288453,1.,1.67835555760094));
#47494=CARTESIAN_POINT('Ctrl Pts',(-3.81919554100522,-1.,1.67864354606363));
#47495=CARTESIAN_POINT('Ctrl Pts',(-3.81919554100522,1.,1.67864354606363));
#47496=CARTESIAN_POINT('Ctrl Pts',(-3.81137549624273,-1.,1.67889737738311));
#47497=CARTESIAN_POINT('Ctrl Pts',(-3.81137549624273,1.,1.67889737738311));
#47498=CARTESIAN_POINT('Ctrl Pts',(-3.80356289078481,-1.,1.67911690648128));
#47499=CARTESIAN_POINT('Ctrl Pts',(-3.80356289078481,1.,1.67911690648128));
#47500=CARTESIAN_POINT('Ctrl Pts',(-3.7957579157763,-1.,1.67930196625203));
#47501=CARTESIAN_POINT('Ctrl Pts',(-3.7957579157763,1.,1.67930196625203));
#47502=CARTESIAN_POINT('Ctrl Pts',(-3.78796080021026,-1.,1.67945236653175));
#47503=CARTESIAN_POINT('Ctrl Pts',(-3.78796080021026,1.,1.67945236653175));
#47504=CARTESIAN_POINT('Ctrl Pts',(-3.78017178196859,-1.,1.67956789211943));
#47505=CARTESIAN_POINT('Ctrl Pts',(-3.78017178196859,1.,1.67956789211943));
#47506=CARTESIAN_POINT('Ctrl Pts',(-3.77239107928394,-1.,1.67964830084946));
#47507=CARTESIAN_POINT('Ctrl Pts',(-3.77239107928394,1.,1.67964830084946));
#47508=CARTESIAN_POINT('Ctrl Pts',(-3.76461886684523,-1.,1.67969332319322));
#47509=CARTESIAN_POINT('Ctrl Pts',(-3.76461886684523,1.,1.67969332319322));
#47510=CARTESIAN_POINT('Ctrl Pts',(-3.75685523754816,-1.,1.67970265841379));
#47511=CARTESIAN_POINT('Ctrl Pts',(-3.75685523754816,1.,1.67970265841379));
#47512=CARTESIAN_POINT('Ctrl Pts',(-3.74910022394845,-1.,1.67967598599665));
#47513=CARTESIAN_POINT('Ctrl Pts',(-3.74910022394845,1.,1.67967598599665));
#47514=CARTESIAN_POINT('Ctrl Pts',(-3.74135385965622,-1.,1.67961298685316));
#47515=CARTESIAN_POINT('Ctrl Pts',(-3.74135385965622,1.,1.67961298685316));
#47516=CARTESIAN_POINT('Ctrl Pts',(-3.73361623282617,-1.,1.67951336376434));
#47517=CARTESIAN_POINT('Ctrl Pts',(-3.73361623282617,1.,1.67951336376434));
#47518=CARTESIAN_POINT('Ctrl Pts',(-3.72588753416339,-1.,1.67937685856627));
#47519=CARTESIAN_POINT('Ctrl Pts',(-3.72588753416339,1.,1.67937685856627));
#47520=CARTESIAN_POINT('Ctrl Pts',(-3.71816812842188,-1.,1.6792032807165));
#47521=CARTESIAN_POINT('Ctrl Pts',(-3.71816812842188,1.,1.6792032807165));
#47522=CARTESIAN_POINT('Ctrl Pts',(-3.71045854208195,-1.,1.67899249793398));
#47523=CARTESIAN_POINT('Ctrl Pts',(-3.71045854208195,1.,1.67899249793398));
#47524=CARTESIAN_POINT('Ctrl Pts',(-3.70275932350998,-1.,1.6787443694862));
#47525=CARTESIAN_POINT('Ctrl Pts',(-3.70275932350998,1.,1.6787443694862));
#47526=CARTESIAN_POINT('Ctrl Pts',(-3.69507092759545,-1.,1.67845869064304));
#47527=CARTESIAN_POINT('Ctrl Pts',(-3.69507092759545,1.,1.67845869064304));
#47528=CARTESIAN_POINT('Ctrl Pts',(-3.68739360236505,-1.,1.67813513867973));
#47529=CARTESIAN_POINT('Ctrl Pts',(-3.68739360236505,1.,1.67813513867973));
#47530=CARTESIAN_POINT('Ctrl Pts',(-3.6797272457918,-1.,1.67777320475872));
#47531=CARTESIAN_POINT('Ctrl Pts',(-3.6797272457918,1.,1.67777320475872));
#47532=CARTESIAN_POINT('Ctrl Pts',(-3.67207136294639,-1.,1.67737217414901));
#47533=CARTESIAN_POINT('Ctrl Pts',(-3.67207136294639,1.,1.67737217414901));
#47534=CARTESIAN_POINT('Ctrl Pts',(-3.66442538671018,-1.,1.67693128053153));
#47535=CARTESIAN_POINT('Ctrl Pts',(-3.66442538671018,1.,1.67693128053153));
#47536=CARTESIAN_POINT('Ctrl Pts',(-3.65678894416442,-1.,1.67644983469459));
#47537=CARTESIAN_POINT('Ctrl Pts',(-3.65678894416442,1.,1.67644983469459));
#47538=CARTESIAN_POINT('Ctrl Pts',(-3.64916213574663,-1.,1.6759273594669));
#47539=CARTESIAN_POINT('Ctrl Pts',(-3.64916213574663,1.,1.6759273594669));
#47540=CARTESIAN_POINT('Ctrl Pts',(-3.6415458297232,-1.,1.67536373264839));
#47541=CARTESIAN_POINT('Ctrl Pts',(-3.6415458297232,1.,1.67536373264839));
#47542=CARTESIAN_POINT('Ctrl Pts',(-3.63394189312902,-1.,1.67475929882962));
#47543=CARTESIAN_POINT('Ctrl Pts',(-3.63394189312902,1.,1.67475929882962));
#47544=CARTESIAN_POINT('Ctrl Pts',(-3.62635249450908,-1.,1.67411452372265));
#47545=CARTESIAN_POINT('Ctrl Pts',(-3.62635249450908,1.,1.67411452372265));
#47546=CARTESIAN_POINT('Ctrl Pts',(-3.61877947398179,-1.,1.67342968196223));
#47547=CARTESIAN_POINT('Ctrl Pts',(-3.61877947398179,1.,1.67342968196223));
#47548=CARTESIAN_POINT('Ctrl Pts',(-3.61122367156182,-1.,1.67270452466968));
#47549=CARTESIAN_POINT('Ctrl Pts',(-3.61122367156182,1.,1.67270452466968));
#47550=CARTESIAN_POINT('Ctrl Pts',(-3.60368430815203,-1.,1.67193797318598));
#47551=CARTESIAN_POINT('Ctrl Pts',(-3.60368430815203,1.,1.67193797318598));
#47552=CARTESIAN_POINT('Ctrl Pts',(-3.59615824388808,-1.,1.67112775290706));
#47553=CARTESIAN_POINT('Ctrl Pts',(-3.59615824388808,1.,1.67112775290706));
#47554=CARTESIAN_POINT('Ctrl Pts',(-3.5886414309783,-1.,1.67027110397601));
#47555=CARTESIAN_POINT('Ctrl Pts',(-3.5886414309783,1.,1.67027110397601));
#47556=CARTESIAN_POINT('Ctrl Pts',(-3.58113044183823,-1.,1.66936552908228));
#47557=CARTESIAN_POINT('Ctrl Pts',(-3.58113044183823,1.,1.66936552908228));
#47558=CARTESIAN_POINT('Ctrl Pts',(-3.57362406285884,-1.,1.66840957407299));
#47559=CARTESIAN_POINT('Ctrl Pts',(-3.57362406285884,1.,1.66840957407299));
#47560=CARTESIAN_POINT('Ctrl Pts',(-3.56612465179429,-1.,1.66740349220308));
#47561=CARTESIAN_POINT('Ctrl Pts',(-3.56612465179429,1.,1.66740349220308));
#47562=CARTESIAN_POINT('Ctrl Pts',(-3.55864015233617,-1.,1.66635023293121));
#47563=CARTESIAN_POINT('Ctrl Pts',(-3.55864015233617,1.,1.66635023293121));
#47564=CARTESIAN_POINT('Ctrl Pts',(-3.5511812134288,-1.,1.66525401569004));
#47565=CARTESIAN_POINT('Ctrl Pts',(-3.5511812134288,1.,1.66525401569004));
#47566=CARTESIAN_POINT('Ctrl Pts',(-3.5437574747503,-1.,1.66411849222334));
#47567=CARTESIAN_POINT('Ctrl Pts',(-3.5437574747503,1.,1.66411849222334));
#47568=CARTESIAN_POINT('Ctrl Pts',(-3.53637385060225,-1.,1.66294490916113));
#47569=CARTESIAN_POINT('Ctrl Pts',(-3.53637385060225,1.,1.66294490916113));
#47570=CARTESIAN_POINT('Ctrl Pts',(-3.52902746211081,-1.,1.66173058912365));
#47571=CARTESIAN_POINT('Ctrl Pts',(-3.52902746211081,1.,1.66173058912365));
#47572=CARTESIAN_POINT('Ctrl Pts',(-3.52170261543787,-1.,1.66046645222266));
#47573=CARTESIAN_POINT('Ctrl Pts',(-3.52170261543787,1.,1.66046645222266));
#47574=CARTESIAN_POINT('Ctrl Pts',(-3.51437632188903,-1.,1.65913971687324));
#47575=CARTESIAN_POINT('Ctrl Pts',(-3.51437632188903,1.,1.65913971687324));
#47576=CARTESIAN_POINT('Ctrl Pts',(-3.5070273314651,-1.,1.65773832633617));
#47577=CARTESIAN_POINT('Ctrl Pts',(-3.5070273314651,1.,1.65773832633617));
#47578=CARTESIAN_POINT('Ctrl Pts',(-3.49964476477929,-1.,1.65625517961583));
#47579=CARTESIAN_POINT('Ctrl Pts',(-3.49964476477929,1.,1.65625517961583));
#47580=CARTESIAN_POINT('Ctrl Pts',(-3.49223525300194,-1.,1.65469162644476));
#47581=CARTESIAN_POINT('Ctrl Pts',(-3.49223525300194,1.,1.65469162644476));
#47582=CARTESIAN_POINT('Ctrl Pts',(-3.48483492840942,-1.,1.65306335367762));
#47583=CARTESIAN_POINT('Ctrl Pts',(-3.48483492840942,1.,1.65306335367762));
#47584=CARTESIAN_POINT('Ctrl Pts',(-3.47749926256543,-1.,1.65139534930353));
#47585=CARTESIAN_POINT('Ctrl Pts',(-3.47749926256543,1.,1.65139534930353));
#47586=CARTESIAN_POINT('Ctrl Pts',(-3.47028140996055,-1.,1.64971118698285));
#47587=CARTESIAN_POINT('Ctrl Pts',(-3.47028140996055,1.,1.64971118698285));
#47588=CARTESIAN_POINT('Ctrl Pts',(-3.46321237515029,-1.,1.64802323352752));
#47589=CARTESIAN_POINT('Ctrl Pts',(-3.46321237515029,1.,1.64802323352752));
#47590=CARTESIAN_POINT('Ctrl Pts',(-3.4562842106239,-1.,1.64632429697506));
#47591=CARTESIAN_POINT('Ctrl Pts',(-3.4562842106239,1.,1.64632429697506));
#47592=CARTESIAN_POINT('Ctrl Pts',(-3.44942242546693,-1.,1.64457408708059));
#47593=CARTESIAN_POINT('Ctrl Pts',(-3.44942242546693,1.,1.64457408708059));
#47594=CARTESIAN_POINT('Ctrl Pts',(-3.44250337701736,-1.,1.64270733821042));
#47595=CARTESIAN_POINT('Ctrl Pts',(-3.44250337701736,1.,1.64270733821042));
#47596=CARTESIAN_POINT('Ctrl Pts',(-3.43540451921397,-1.,1.64065778701952));
#47597=CARTESIAN_POINT('Ctrl Pts',(-3.43540451921397,1.,1.64065778701952));
#47598=CARTESIAN_POINT('Ctrl Pts',(-3.42804772926213,-1.,1.6383787624689));
#47599=CARTESIAN_POINT('Ctrl Pts',(-3.42804772926213,1.,1.6383787624689));
#47600=CARTESIAN_POINT('Ctrl Pts',(-3.4204397459095,-1.,1.63586250099804));
#47601=CARTESIAN_POINT('Ctrl Pts',(-3.4204397459095,1.,1.63586250099804));
#47602=CARTESIAN_POINT('Ctrl Pts',(-3.41272817148719,-1.,1.63316667054156));
#47603=CARTESIAN_POINT('Ctrl Pts',(-3.41272817148719,1.,1.63316667054156));
#47604=CARTESIAN_POINT('Ctrl Pts',(-3.40519422740596,-1.,1.63041148964996));
#47605=CARTESIAN_POINT('Ctrl Pts',(-3.40519422740596,1.,1.63041148964996));
#47606=CARTESIAN_POINT('Ctrl Pts',(-3.39818605298342,-1.,1.62774916464571));
#47607=CARTESIAN_POINT('Ctrl Pts',(-3.39818605298342,1.,1.62774916464571));
#47608=CARTESIAN_POINT('Ctrl Pts',(-3.39206617497078,-1.,1.62533996116793));
#47609=CARTESIAN_POINT('Ctrl Pts',(-3.39206617497078,1.,1.62533996116793));
#47610=CARTESIAN_POINT('Ctrl Pts',(-3.38715832178929,-1.,1.62332788556183));
#47611=CARTESIAN_POINT('Ctrl Pts',(-3.38715832178929,1.,1.62332788556183));
#47612=CARTESIAN_POINT('Ctrl Pts',(-3.38368201668123,-1.,1.62181089631134));
#47613=CARTESIAN_POINT('Ctrl Pts',(-3.38368201668123,1.,1.62181089631134));
#47614=CARTESIAN_POINT('Ctrl Pts',(-3.38212861099481,-1.,1.62103022180917));
#47615=CARTESIAN_POINT('Ctrl Pts',(-3.38212861099481,1.,1.62103022180917));
#47616=CARTESIAN_POINT('Ctrl Pts',(-3.38166984193496,-1.,1.6206953236804));
#47617=CARTESIAN_POINT('Ctrl Pts',(-3.38166984193496,1.,1.6206953236804));
#47618=CARTESIAN_POINT('Ctrl Pts',(-3.38167767992546,-1.,1.62058335162421));
#47619=CARTESIAN_POINT('Ctrl Pts',(-3.38167767992546,1.,1.62058335162421));
#47620=CARTESIAN_POINT('Ctrl Pts',(-3.38176002566879,-1.,1.62055519152808));
#47621=CARTESIAN_POINT('Ctrl Pts',(-3.38176002566879,1.,1.62055519152808));
#47622=CARTESIAN_POINT('',(-3.85054988729471,1.,1.67727921511438));
#47623=CARTESIAN_POINT('Ctrl Pts',(-3.85054988729471,1.,1.67727921511438));
#47624=CARTESIAN_POINT('Ctrl Pts',(-3.84897939431104,1.,1.6773605765671));
#47625=CARTESIAN_POINT('Ctrl Pts',(-3.84583912297567,1.,1.67751991140661));
#47626=CARTESIAN_POINT('Ctrl Pts',(-3.8411308598706,1.,1.67774874946867));
#47627=CARTESIAN_POINT('Ctrl Pts',(-3.83485746516115,1.,1.67803353065273));
#47628=CARTESIAN_POINT('Ctrl Pts',(-3.82702289288453,1.,1.67835555760094));
#47629=CARTESIAN_POINT('Ctrl Pts',(-3.81919554100522,1.,1.67864354606363));
#47630=CARTESIAN_POINT('Ctrl Pts',(-3.81137549624273,1.,1.67889737738311));
#47631=CARTESIAN_POINT('Ctrl Pts',(-3.80356289078481,1.,1.67911690648128));
#47632=CARTESIAN_POINT('Ctrl Pts',(-3.7957579157763,1.,1.67930196625203));
#47633=CARTESIAN_POINT('Ctrl Pts',(-3.78796080021026,1.,1.67945236653175));
#47634=CARTESIAN_POINT('Ctrl Pts',(-3.78017178196859,1.,1.67956789211943));
#47635=CARTESIAN_POINT('Ctrl Pts',(-3.77239107928394,1.,1.67964830084946));
#47636=CARTESIAN_POINT('Ctrl Pts',(-3.76461886684523,1.,1.67969332319322));
#47637=CARTESIAN_POINT('Ctrl Pts',(-3.75685523754816,1.,1.67970265841379));
#47638=CARTESIAN_POINT('Ctrl Pts',(-3.74910022394845,1.,1.67967598599665));
#47639=CARTESIAN_POINT('Ctrl Pts',(-3.74135385965622,1.,1.67961298685316));
#47640=CARTESIAN_POINT('Ctrl Pts',(-3.73361623282617,1.,1.67951336376434));
#47641=CARTESIAN_POINT('Ctrl Pts',(-3.72588753416339,1.,1.67937685856627));
#47642=CARTESIAN_POINT('Ctrl Pts',(-3.71816812842188,1.,1.6792032807165));
#47643=CARTESIAN_POINT('Ctrl Pts',(-3.71045854208195,1.,1.67899249793398));
#47644=CARTESIAN_POINT('Ctrl Pts',(-3.70275932350998,1.,1.6787443694862));
#47645=CARTESIAN_POINT('Ctrl Pts',(-3.69507092759545,1.,1.67845869064304));
#47646=CARTESIAN_POINT('Ctrl Pts',(-3.68739360236505,1.,1.67813513867973));
#47647=CARTESIAN_POINT('Ctrl Pts',(-3.6797272457918,1.,1.67777320475872));
#47648=CARTESIAN_POINT('Ctrl Pts',(-3.67207136294639,1.,1.67737217414901));
#47649=CARTESIAN_POINT('Ctrl Pts',(-3.66442538671018,1.,1.67693128053153));
#47650=CARTESIAN_POINT('Ctrl Pts',(-3.65678894416442,1.,1.67644983469459));
#47651=CARTESIAN_POINT('Ctrl Pts',(-3.64916213574663,1.,1.6759273594669));
#47652=CARTESIAN_POINT('Ctrl Pts',(-3.6415458297232,1.,1.67536373264839));
#47653=CARTESIAN_POINT('Ctrl Pts',(-3.63394189312902,1.,1.67475929882962));
#47654=CARTESIAN_POINT('Ctrl Pts',(-3.62635249450908,1.,1.67411452372265));
#47655=CARTESIAN_POINT('Ctrl Pts',(-3.61877947398179,1.,1.67342968196223));
#47656=CARTESIAN_POINT('Ctrl Pts',(-3.61122367156182,1.,1.67270452466968));
#47657=CARTESIAN_POINT('Ctrl Pts',(-3.60368430815203,1.,1.67193797318598));
#47658=CARTESIAN_POINT('Ctrl Pts',(-3.59615824388808,1.,1.67112775290706));
#47659=CARTESIAN_POINT('Ctrl Pts',(-3.5886414309783,1.,1.67027110397601));
#47660=CARTESIAN_POINT('Ctrl Pts',(-3.58113044183823,1.,1.66936552908228));
#47661=CARTESIAN_POINT('Ctrl Pts',(-3.57362406285884,1.,1.66840957407299));
#47662=CARTESIAN_POINT('Ctrl Pts',(-3.56612465179429,1.,1.66740349220308));
#47663=CARTESIAN_POINT('Ctrl Pts',(-3.55864015233617,1.,1.66635023293121));
#47664=CARTESIAN_POINT('Ctrl Pts',(-3.5511812134288,1.,1.66525401569004));
#47665=CARTESIAN_POINT('Ctrl Pts',(-3.5437574747503,1.,1.66411849222334));
#47666=CARTESIAN_POINT('Ctrl Pts',(-3.53637385060225,1.,1.66294490916113));
#47667=CARTESIAN_POINT('Ctrl Pts',(-3.52902746211081,1.,1.66173058912365));
#47668=CARTESIAN_POINT('Ctrl Pts',(-3.52170261543787,1.,1.66046645222266));
#47669=CARTESIAN_POINT('Ctrl Pts',(-3.51437632188903,1.,1.65913971687324));
#47670=CARTESIAN_POINT('Ctrl Pts',(-3.5070273314651,1.,1.65773832633617));
#47671=CARTESIAN_POINT('Ctrl Pts',(-3.49964476477929,1.,1.65625517961583));
#47672=CARTESIAN_POINT('Ctrl Pts',(-3.49223525300194,1.,1.65469162644476));
#47673=CARTESIAN_POINT('Ctrl Pts',(-3.48483492840942,1.,1.65306335367762));
#47674=CARTESIAN_POINT('Ctrl Pts',(-3.47749926256543,1.,1.65139534930353));
#47675=CARTESIAN_POINT('Ctrl Pts',(-3.47028140996055,1.,1.64971118698285));
#47676=CARTESIAN_POINT('Ctrl Pts',(-3.46321237515029,1.,1.64802323352752));
#47677=CARTESIAN_POINT('Ctrl Pts',(-3.4562842106239,1.,1.64632429697506));
#47678=CARTESIAN_POINT('Ctrl Pts',(-3.44942242546693,1.,1.64457408708059));
#47679=CARTESIAN_POINT('Ctrl Pts',(-3.44250337701736,1.,1.64270733821042));
#47680=CARTESIAN_POINT('Ctrl Pts',(-3.43540451921397,1.,1.64065778701952));
#47681=CARTESIAN_POINT('Ctrl Pts',(-3.42804772926213,1.,1.6383787624689));
#47682=CARTESIAN_POINT('Ctrl Pts',(-3.4204397459095,1.,1.63586250099804));
#47683=CARTESIAN_POINT('Ctrl Pts',(-3.41272817148719,1.,1.63316667054156));
#47684=CARTESIAN_POINT('Ctrl Pts',(-3.40519422740596,1.,1.63041148964996));
#47685=CARTESIAN_POINT('Ctrl Pts',(-3.39818605298342,1.,1.62774916464571));
#47686=CARTESIAN_POINT('Ctrl Pts',(-3.39206617497078,1.,1.62533996116793));
#47687=CARTESIAN_POINT('Ctrl Pts',(-3.38715832178929,1.,1.62332788556183));
#47688=CARTESIAN_POINT('Ctrl Pts',(-3.3839428576331,1.,1.62192472202795));
#47689=CARTESIAN_POINT('Ctrl Pts',(-3.38243080602536,1.,1.62118047294574));
#47690=CARTESIAN_POINT('Ctrl Pts',(-3.38187506457001,1.,1.62083271136059));
#47691=CARTESIAN_POINT('Ctrl Pts',(-3.38173802621243,1.,1.62069086551626));
#47692=CARTESIAN_POINT('Ctrl Pts',(-3.38171594275687,1.,1.62064718014256));
#47693=CARTESIAN_POINT('',(-3.85054988729471,0.,1.67727921511438));
#47694=CARTESIAN_POINT('Ctrl Pts',(-3.53717101171257,-1.,1.24535988127942));
#47695=CARTESIAN_POINT('Ctrl Pts',(-3.53717101171257,1.,1.24535988127942));
#47696=CARTESIAN_POINT('Ctrl Pts',(-3.53713269667534,-1.,1.24528174185147));
#47697=CARTESIAN_POINT('Ctrl Pts',(-3.53713269667534,1.,1.24528174185147));
#47698=CARTESIAN_POINT('Ctrl Pts',(-3.53720633058152,-1.,1.2451970233558));
#47699=CARTESIAN_POINT('Ctrl Pts',(-3.53720633058152,1.,1.2451970233558));
#47700=CARTESIAN_POINT('Ctrl Pts',(-3.53776753803428,-1.,1.24528461333177));
#47701=CARTESIAN_POINT('Ctrl Pts',(-3.53776753803428,1.,1.24528461333177));
#47702=CARTESIAN_POINT('Ctrl Pts',(-3.53941798196293,-1.,1.24583101679199));
#47703=CARTESIAN_POINT('Ctrl Pts',(-3.53941798196293,1.,1.24583101679199));
#47704=CARTESIAN_POINT('Ctrl Pts',(-3.54294877426113,-1.,1.2472164623202));
#47705=CARTESIAN_POINT('Ctrl Pts',(-3.54294877426113,1.,1.2472164623202));
#47706=CARTESIAN_POINT('Ctrl Pts',(-3.54784190282889,-1.,1.24926408627938));
#47707=CARTESIAN_POINT('Ctrl Pts',(-3.54784190282889,1.,1.24926408627938));
#47708=CARTESIAN_POINT('Ctrl Pts',(-3.5538728741862,-1.,1.25188792940508));
#47709=CARTESIAN_POINT('Ctrl Pts',(-3.5538728741862,1.,1.25188792940508));
#47710=CARTESIAN_POINT('Ctrl Pts',(-3.56071094990825,-1.,1.25496090899873));
#47711=CARTESIAN_POINT('Ctrl Pts',(-3.56071094990825,1.,1.25496090899873));
#47712=CARTESIAN_POINT('Ctrl Pts',(-3.56798645995025,-1.,1.25834000485626));
#47713=CARTESIAN_POINT('Ctrl Pts',(-3.56798645995025,1.,1.25834000485626));
#47714=CARTESIAN_POINT('Ctrl Pts',(-3.5753456065164,-1.,1.26188667142784));
#47715=CARTESIAN_POINT('Ctrl Pts',(-3.5753456065164,1.,1.26188667142784));
#47716=CARTESIAN_POINT('Ctrl Pts',(-3.58250452868699,-1.,1.26548706249891));
#47717=CARTESIAN_POINT('Ctrl Pts',(-3.58250452868699,1.,1.26548706249891));
#47718=CARTESIAN_POINT('Ctrl Pts',(-3.5893180784647,-1.,1.26907758484766));
#47719=CARTESIAN_POINT('Ctrl Pts',(-3.5893180784647,1.,1.26907758484766));
#47720=CARTESIAN_POINT('Ctrl Pts',(-3.59578698050164,-1.,1.27264798379365));
#47721=CARTESIAN_POINT('Ctrl Pts',(-3.59578698050164,1.,1.27264798379365));
#47722=CARTESIAN_POINT('Ctrl Pts',(-3.60199947736404,-1.,1.27622049908664));
#47723=CARTESIAN_POINT('Ctrl Pts',(-3.60199947736404,1.,1.27622049908664));
#47724=CARTESIAN_POINT('Ctrl Pts',(-3.60808907746372,-1.,1.27983492861703));
#47725=CARTESIAN_POINT('Ctrl Pts',(-3.60808907746372,1.,1.27983492861703));
#47726=CARTESIAN_POINT('Ctrl Pts',(-3.61418935913793,-1.,1.28353255117754));
#47727=CARTESIAN_POINT('Ctrl Pts',(-3.61418935913793,1.,1.28353255117754));
#47728=CARTESIAN_POINT('Ctrl Pts',(-3.62038148492295,-1.,1.2873375502936));
#47729=CARTESIAN_POINT('Ctrl Pts',(-3.62038148492295,1.,1.2873375502936));
#47730=CARTESIAN_POINT('Ctrl Pts',(-3.62667616004299,-1.,1.29125046021853));
#47731=CARTESIAN_POINT('Ctrl Pts',(-3.62667616004299,1.,1.29125046021853));
#47732=CARTESIAN_POINT('Ctrl Pts',(-3.63304271630995,-1.,1.29525810207744));
#47733=CARTESIAN_POINT('Ctrl Pts',(-3.63304271630995,1.,1.29525810207744));
#47734=CARTESIAN_POINT('Ctrl Pts',(-3.6394268987279,-1.,1.29933955906463));
#47735=CARTESIAN_POINT('Ctrl Pts',(-3.6394268987279,1.,1.29933955906463));
#47736=CARTESIAN_POINT('Ctrl Pts',(-3.64577181380125,-1.,1.30347327603778));
#47737=CARTESIAN_POINT('Ctrl Pts',(-3.64577181380125,1.,1.30347327603778));
#47738=CARTESIAN_POINT('Ctrl Pts',(-3.65204081987101,-1.,1.30764479590051));
#47739=CARTESIAN_POINT('Ctrl Pts',(-3.65204081987101,1.,1.30764479590051));
#47740=CARTESIAN_POINT('Ctrl Pts',(-3.65822827358655,-1.,1.31185038411231));
#47741=CARTESIAN_POINT('Ctrl Pts',(-3.65822827358655,1.,1.31185038411231));
#47742=CARTESIAN_POINT('Ctrl Pts',(-3.66434688899822,-1.,1.31609271239922));
#47743=CARTESIAN_POINT('Ctrl Pts',(-3.66434688899822,1.,1.31609271239922));
#47744=CARTESIAN_POINT('Ctrl Pts',(-3.67042021752668,-1.,1.3203782813777));
#47745=CARTESIAN_POINT('Ctrl Pts',(-3.67042021752668,1.,1.3203782813777));
#47746=CARTESIAN_POINT('Ctrl Pts',(-3.67647355257906,-1.,1.32471430856413));
#47747=CARTESIAN_POINT('Ctrl Pts',(-3.67647355257906,1.,1.32471430856413));
#47748=CARTESIAN_POINT('Ctrl Pts',(-3.68252441182534,-1.,1.32910547072734));
#47749=CARTESIAN_POINT('Ctrl Pts',(-3.68252441182534,1.,1.32910547072734));
#47750=CARTESIAN_POINT('Ctrl Pts',(-3.68857672413013,-1.,1.33355191034515));
#47751=CARTESIAN_POINT('Ctrl Pts',(-3.68857672413013,1.,1.33355191034515));
#47752=CARTESIAN_POINT('Ctrl Pts',(-3.69462613305692,-1.,1.33805103398214));
#47753=CARTESIAN_POINT('Ctrl Pts',(-3.69462613305692,1.,1.33805103398214));
#47754=CARTESIAN_POINT('Ctrl Pts',(-3.70066324015112,-1.,1.3425986075293));
#47755=CARTESIAN_POINT('Ctrl Pts',(-3.70066324015112,1.,1.3425986075293));
#47756=CARTESIAN_POINT('Ctrl Pts',(-3.7066775318825,-1.,1.34719008463535));
#47757=CARTESIAN_POINT('Ctrl Pts',(-3.7066775318825,1.,1.34719008463535));
#47758=CARTESIAN_POINT('Ctrl Pts',(-3.71266130563061,-1.,1.35182193384426));
#47759=CARTESIAN_POINT('Ctrl Pts',(-3.71266130563061,1.,1.35182193384426));
#47760=CARTESIAN_POINT('Ctrl Pts',(-3.71861271513318,-1.,1.35649266705038));
#47761=CARTESIAN_POINT('Ctrl Pts',(-3.71861271513318,1.,1.35649266705038));
#47762=CARTESIAN_POINT('Ctrl Pts',(-3.72453364678279,-1.,1.36120211416353));
#47763=CARTESIAN_POINT('Ctrl Pts',(-3.72453364678279,1.,1.36120211416353));
#47764=CARTESIAN_POINT('Ctrl Pts',(-3.73042829011293,-1.,1.36595093298674));
#47765=CARTESIAN_POINT('Ctrl Pts',(-3.73042829011293,1.,1.36595093298674));
#47766=CARTESIAN_POINT('Ctrl Pts',(-3.73630145885809,-1.,1.37074003422739));
#47767=CARTESIAN_POINT('Ctrl Pts',(-3.73630145885809,1.,1.37074003422739));
#47768=CARTESIAN_POINT('Ctrl Pts',(-3.7421569816256,-1.,1.3755700297169));
#47769=CARTESIAN_POINT('Ctrl Pts',(-3.7421569816256,1.,1.3755700297169));
#47770=CARTESIAN_POINT('Ctrl Pts',(-3.74799617204744,-1.,1.38044070763302));
#47771=CARTESIAN_POINT('Ctrl Pts',(-3.74799617204744,1.,1.38044070763302));
#47772=CARTESIAN_POINT('Ctrl Pts',(-3.75381861212728,-1.,1.38535129801185));
#47773=CARTESIAN_POINT('Ctrl Pts',(-3.75381861212728,1.,1.38535129801185));
#47774=CARTESIAN_POINT('Ctrl Pts',(-3.75962280650875,-1.,1.39030069388926));
#47775=CARTESIAN_POINT('Ctrl Pts',(-3.75962280650875,1.,1.39030069388926));
#47776=CARTESIAN_POINT('Ctrl Pts',(-3.76540689249078,-1.,1.39528769118054));
#47777=CARTESIAN_POINT('Ctrl Pts',(-3.76540689249078,1.,1.39528769118054));
#47778=CARTESIAN_POINT('Ctrl Pts',(-3.77116930621804,-1.,1.40031121335495));
#47779=CARTESIAN_POINT('Ctrl Pts',(-3.77116930621804,1.,1.40031121335495));
#47780=CARTESIAN_POINT('Ctrl Pts',(-3.77690952014209,-1.,1.40537056004702));
#47781=CARTESIAN_POINT('Ctrl Pts',(-3.77690952014209,1.,1.40537056004702));
#47782=CARTESIAN_POINT('Ctrl Pts',(-3.78262780065406,-1.,1.41046532282567));
#47783=CARTESIAN_POINT('Ctrl Pts',(-3.78262780065406,1.,1.41046532282567));
#47784=CARTESIAN_POINT('Ctrl Pts',(-3.78832489879369,-1.,1.41559527803808));
#47785=CARTESIAN_POINT('Ctrl Pts',(-3.78832489879369,1.,1.41559527803808));
#47786=CARTESIAN_POINT('Ctrl Pts',(-3.7940017574439,-1.,1.42076028482828));
#47787=CARTESIAN_POINT('Ctrl Pts',(-3.7940017574439,1.,1.42076028482828));
#47788=CARTESIAN_POINT('Ctrl Pts',(-3.79965923196365,-1.,1.42596018777301));
#47789=CARTESIAN_POINT('Ctrl Pts',(-3.79965923196365,1.,1.42596018777301));
#47790=CARTESIAN_POINT('Ctrl Pts',(-3.80529775429916,-1.,1.43119469921364));
#47791=CARTESIAN_POINT('Ctrl Pts',(-3.80529775429916,1.,1.43119469921364));
#47792=CARTESIAN_POINT('Ctrl Pts',(-3.81091737726965,-1.,1.43646341556783));
#47793=CARTESIAN_POINT('Ctrl Pts',(-3.81091737726965,1.,1.43646341556783));
#47794=CARTESIAN_POINT('Ctrl Pts',(-3.8165179239855,-1.,1.441765870414));
#47795=CARTESIAN_POINT('Ctrl Pts',(-3.8165179239855,1.,1.441765870414));
#47796=CARTESIAN_POINT('Ctrl Pts',(-3.82209910620591,-1.,1.44710157648562));
#47797=CARTESIAN_POINT('Ctrl Pts',(-3.82209910620591,1.,1.44710157648562));
#47798=CARTESIAN_POINT('Ctrl Pts',(-3.82766064519,-1.,1.45247006796807));
#47799=CARTESIAN_POINT('Ctrl Pts',(-3.82766064519,1.,1.45247006796807));
#47800=CARTESIAN_POINT('Ctrl Pts',(-3.83320241775199,-1.,1.45787095220763));
#47801=CARTESIAN_POINT('Ctrl Pts',(-3.83320241775199,1.,1.45787095220763));
#47802=CARTESIAN_POINT('Ctrl Pts',(-3.83872447159309,-1.,1.46330391180621));
#47803=CARTESIAN_POINT('Ctrl Pts',(-3.83872447159309,1.,1.46330391180621));
#47804=CARTESIAN_POINT('Ctrl Pts',(-3.84422695454469,-1.,1.46876867426374));
#47805=CARTESIAN_POINT('Ctrl Pts',(-3.84422695454469,1.,1.46876867426374));
#47806=CARTESIAN_POINT('Ctrl Pts',(-3.84971006847096,-1.,1.47426499018467));
#47807=CARTESIAN_POINT('Ctrl Pts',(-3.84971006847096,1.,1.47426499018467));
#47808=CARTESIAN_POINT('Ctrl Pts',(-3.85517401698952,-1.,1.47979260991063));
#47809=CARTESIAN_POINT('Ctrl Pts',(-3.85517401698952,1.,1.47979260991063));
#47810=CARTESIAN_POINT('Ctrl Pts',(-3.86061894706551,-1.,1.48535125510102));
#47811=CARTESIAN_POINT('Ctrl Pts',(-3.86061894706551,1.,1.48535125510102));
#47812=CARTESIAN_POINT('Ctrl Pts',(-3.86604492575933,-1.,1.49094061164604));
#47813=CARTESIAN_POINT('Ctrl Pts',(-3.86604492575933,1.,1.49094061164604));
#47814=CARTESIAN_POINT('Ctrl Pts',(-3.8714519699927,-1.,1.4965603539944));
#47815=CARTESIAN_POINT('Ctrl Pts',(-3.8714519699927,1.,1.4965603539944));
#47816=CARTESIAN_POINT('Ctrl Pts',(-3.87684006372665,-1.,1.50221016176766));
#47817=CARTESIAN_POINT('Ctrl Pts',(-3.87684006372665,1.,1.50221016176766));
#47818=CARTESIAN_POINT('Ctrl Pts',(-3.88220917950443,-1.,1.50788973857719));
#47819=CARTESIAN_POINT('Ctrl Pts',(-3.88220917950443,1.,1.50788973857719));
#47820=CARTESIAN_POINT('Ctrl Pts',(-3.88755930032927,-1.,1.51359883110181));
#47821=CARTESIAN_POINT('Ctrl Pts',(-3.88755930032927,1.,1.51359883110181));
#47822=CARTESIAN_POINT('Ctrl Pts',(-3.89289043531893,-1.,1.51933724328609));
#47823=CARTESIAN_POINT('Ctrl Pts',(-3.89289043531893,1.,1.51933724328609));
#47824=CARTESIAN_POINT('Ctrl Pts',(-3.8982026070607,-1.,1.52510482990784));
#47825=CARTESIAN_POINT('Ctrl Pts',(-3.8982026070607,1.,1.52510482990784));
#47826=CARTESIAN_POINT('Ctrl Pts',(-3.90243719629755,-1.,1.5297421605556));
#47827=CARTESIAN_POINT('Ctrl Pts',(-3.90243719629755,1.,1.5297421605556));
#47828=CARTESIAN_POINT('Ctrl Pts',(-3.90560462812846,-1.,1.53323321827311));
#47829=CARTESIAN_POINT('Ctrl Pts',(-3.90560462812846,1.,1.53323321827311));
#47830=CARTESIAN_POINT('Ctrl Pts',(-3.90771246854607,-1.,1.53556639217742));
#47831=CARTESIAN_POINT('Ctrl Pts',(-3.90771246854607,1.,1.53556639217742));
#47832=CARTESIAN_POINT('Ctrl Pts',(-3.90876544355381,-1.,1.53673442965255));
#47833=CARTESIAN_POINT('Ctrl Pts',(-3.90876544355381,1.,1.53673442965255));
#47834=CARTESIAN_POINT('',(-3.5372048861591,1.,1.24526366418208));
#47835=CARTESIAN_POINT('Ctrl Pts',(-3.5372048861591,-1.,1.24526366418208));
#47836=CARTESIAN_POINT('Ctrl Pts',(-3.5372048861591,-0.666666666666667,
1.24526366418208));
#47837=CARTESIAN_POINT('Ctrl Pts',(-3.5372048861591,-0.333333333333333,
1.24526366418208));
#47838=CARTESIAN_POINT('Ctrl Pts',(-3.5372048861591,0.333333333333333,1.24526366418208));
#47839=CARTESIAN_POINT('Ctrl Pts',(-3.5372048861591,0.666666666666667,1.24526366418208));
#47840=CARTESIAN_POINT('Ctrl Pts',(-3.5372048861591,1.,1.24526366418208));
#47841=CARTESIAN_POINT('',(-3.90876544355381,1.,1.53673442965255));
#47842=CARTESIAN_POINT('',(-3.90876544355381,0.,1.53673442965255));
#47843=CARTESIAN_POINT('Ctrl Pts',(-3.5372048861591,1.,1.24526366418208));
#47844=CARTESIAN_POINT('Ctrl Pts',(-3.53725139174402,1.,1.24524838931864));
#47845=CARTESIAN_POINT('Ctrl Pts',(-3.53744859265385,1.,1.24524498991133));
#47846=CARTESIAN_POINT('Ctrl Pts',(-3.53808746578052,1.,1.2453920538873));
#47847=CARTESIAN_POINT('Ctrl Pts',(-3.53968291129942,1.,1.24593497225964));
#47848=CARTESIAN_POINT('Ctrl Pts',(-3.54294877426113,1.,1.2472164623202));
#47849=CARTESIAN_POINT('Ctrl Pts',(-3.54784190282889,1.,1.24926408627938));
#47850=CARTESIAN_POINT('Ctrl Pts',(-3.5538728741862,1.,1.25188792940508));
#47851=CARTESIAN_POINT('Ctrl Pts',(-3.56071094990825,1.,1.25496090899873));
#47852=CARTESIAN_POINT('Ctrl Pts',(-3.56798645995025,1.,1.25834000485626));
#47853=CARTESIAN_POINT('Ctrl Pts',(-3.5753456065164,1.,1.26188667142784));
#47854=CARTESIAN_POINT('Ctrl Pts',(-3.58250452868699,1.,1.26548706249891));
#47855=CARTESIAN_POINT('Ctrl Pts',(-3.5893180784647,1.,1.26907758484766));
#47856=CARTESIAN_POINT('Ctrl Pts',(-3.59578698050164,1.,1.27264798379365));
#47857=CARTESIAN_POINT('Ctrl Pts',(-3.60199947736404,1.,1.27622049908664));
#47858=CARTESIAN_POINT('Ctrl Pts',(-3.60808907746372,1.,1.27983492861703));
#47859=CARTESIAN_POINT('Ctrl Pts',(-3.61418935913793,1.,1.28353255117754));
#47860=CARTESIAN_POINT('Ctrl Pts',(-3.62038148492295,1.,1.2873375502936));
#47861=CARTESIAN_POINT('Ctrl Pts',(-3.62667616004299,1.,1.29125046021853));
#47862=CARTESIAN_POINT('Ctrl Pts',(-3.63304271630995,1.,1.29525810207744));
#47863=CARTESIAN_POINT('Ctrl Pts',(-3.6394268987279,1.,1.29933955906463));
#47864=CARTESIAN_POINT('Ctrl Pts',(-3.64577181380125,1.,1.30347327603778));
#47865=CARTESIAN_POINT('Ctrl Pts',(-3.65204081987101,1.,1.30764479590051));
#47866=CARTESIAN_POINT('Ctrl Pts',(-3.65822827358655,1.,1.31185038411231));
#47867=CARTESIAN_POINT('Ctrl Pts',(-3.66434688899822,1.,1.31609271239922));
#47868=CARTESIAN_POINT('Ctrl Pts',(-3.67042021752668,1.,1.3203782813777));
#47869=CARTESIAN_POINT('Ctrl Pts',(-3.67647355257906,1.,1.32471430856413));
#47870=CARTESIAN_POINT('Ctrl Pts',(-3.68252441182534,1.,1.32910547072734));
#47871=CARTESIAN_POINT('Ctrl Pts',(-3.68857672413013,1.,1.33355191034515));
#47872=CARTESIAN_POINT('Ctrl Pts',(-3.69462613305692,1.,1.33805103398214));
#47873=CARTESIAN_POINT('Ctrl Pts',(-3.70066324015112,1.,1.3425986075293));
#47874=CARTESIAN_POINT('Ctrl Pts',(-3.7066775318825,1.,1.34719008463535));
#47875=CARTESIAN_POINT('Ctrl Pts',(-3.71266130563061,1.,1.35182193384426));
#47876=CARTESIAN_POINT('Ctrl Pts',(-3.71861271513318,1.,1.35649266705038));
#47877=CARTESIAN_POINT('Ctrl Pts',(-3.72453364678279,1.,1.36120211416353));
#47878=CARTESIAN_POINT('Ctrl Pts',(-3.73042829011293,1.,1.36595093298674));
#47879=CARTESIAN_POINT('Ctrl Pts',(-3.73630145885809,1.,1.37074003422739));
#47880=CARTESIAN_POINT('Ctrl Pts',(-3.7421569816256,1.,1.3755700297169));
#47881=CARTESIAN_POINT('Ctrl Pts',(-3.74799617204744,1.,1.38044070763302));
#47882=CARTESIAN_POINT('Ctrl Pts',(-3.75381861212728,1.,1.38535129801185));
#47883=CARTESIAN_POINT('Ctrl Pts',(-3.75962280650875,1.,1.39030069388926));
#47884=CARTESIAN_POINT('Ctrl Pts',(-3.76540689249078,1.,1.39528769118054));
#47885=CARTESIAN_POINT('Ctrl Pts',(-3.77116930621804,1.,1.40031121335495));
#47886=CARTESIAN_POINT('Ctrl Pts',(-3.77690952014209,1.,1.40537056004702));
#47887=CARTESIAN_POINT('Ctrl Pts',(-3.78262780065406,1.,1.41046532282567));
#47888=CARTESIAN_POINT('Ctrl Pts',(-3.78832489879369,1.,1.41559527803808));
#47889=CARTESIAN_POINT('Ctrl Pts',(-3.7940017574439,1.,1.42076028482828));
#47890=CARTESIAN_POINT('Ctrl Pts',(-3.79965923196365,1.,1.42596018777301));
#47891=CARTESIAN_POINT('Ctrl Pts',(-3.80529775429916,1.,1.43119469921364));
#47892=CARTESIAN_POINT('Ctrl Pts',(-3.81091737726965,1.,1.43646341556783));
#47893=CARTESIAN_POINT('Ctrl Pts',(-3.8165179239855,1.,1.441765870414));
#47894=CARTESIAN_POINT('Ctrl Pts',(-3.82209910620591,1.,1.44710157648562));
#47895=CARTESIAN_POINT('Ctrl Pts',(-3.82766064519,1.,1.45247006796807));
#47896=CARTESIAN_POINT('Ctrl Pts',(-3.83320241775199,1.,1.45787095220763));
#47897=CARTESIAN_POINT('Ctrl Pts',(-3.83872447159309,1.,1.46330391180621));
#47898=CARTESIAN_POINT('Ctrl Pts',(-3.84422695454469,1.,1.46876867426374));
#47899=CARTESIAN_POINT('Ctrl Pts',(-3.84971006847096,1.,1.47426499018467));
#47900=CARTESIAN_POINT('Ctrl Pts',(-3.85517401698952,1.,1.47979260991063));
#47901=CARTESIAN_POINT('Ctrl Pts',(-3.86061894706551,1.,1.48535125510102));
#47902=CARTESIAN_POINT('Ctrl Pts',(-3.86604492575933,1.,1.49094061164604));
#47903=CARTESIAN_POINT('Ctrl Pts',(-3.8714519699927,1.,1.4965603539944));
#47904=CARTESIAN_POINT('Ctrl Pts',(-3.87684006372665,1.,1.50221016176766));
#47905=CARTESIAN_POINT('Ctrl Pts',(-3.88220917950443,1.,1.50788973857719));
#47906=CARTESIAN_POINT('Ctrl Pts',(-3.88755930032927,1.,1.51359883110181));
#47907=CARTESIAN_POINT('Ctrl Pts',(-3.89289043531893,1.,1.51933724328609));
#47908=CARTESIAN_POINT('Ctrl Pts',(-3.8982026070607,1.,1.52510482990784));
#47909=CARTESIAN_POINT('Ctrl Pts',(-3.90243719629755,1.,1.5297421605556));
#47910=CARTESIAN_POINT('Ctrl Pts',(-3.90560462812846,1.,1.53323321827311));
#47911=CARTESIAN_POINT('Ctrl Pts',(-3.90771246854607,1.,1.53556639217742));
#47912=CARTESIAN_POINT('Ctrl Pts',(-3.90876544355381,1.,1.53673442965255));
#47913=CARTESIAN_POINT('Origin',(-3.90876544355381,0.,1.53673442965255));
#47914=CARTESIAN_POINT('',(-3.85054988729471,1.,1.67727921511438));
#47915=CARTESIAN_POINT('Origin',(0.,0.,0.));
#47916=CARTESIAN_POINT('',(-3.59360648251021,1.,1.071677399622));
#47917=CARTESIAN_POINT('Origin',(0.,1.,0.));
#47918=CARTESIAN_POINT('Ctrl Pts',(-3.59360648251021,1.,1.071677399622));
#47919=CARTESIAN_POINT('Ctrl Pts',(-3.59360648251021,0.666666666666667,
1.071677399622));
#47920=CARTESIAN_POINT('Ctrl Pts',(-3.59360648251021,0.333333333333333,
1.071677399622));
#47921=CARTESIAN_POINT('Ctrl Pts',(-3.59360648251021,-0.333333333333333,
1.071677399622));
#47922=CARTESIAN_POINT('Ctrl Pts',(-3.59360648251021,-0.666666666666667,
1.071677399622));
#47923=CARTESIAN_POINT('Ctrl Pts',(-3.59360648251021,-1.,1.071677399622));
#47924=CARTESIAN_POINT('Ctrl Pts',(-4.06552750530042,-1.,1.05427041296137));
#47925=CARTESIAN_POINT('Ctrl Pts',(-4.06552750530042,1.,1.05427041296137));
#47926=CARTESIAN_POINT('Ctrl Pts',(-4.06398907542679,-1.,1.05459645194934));
#47927=CARTESIAN_POINT('Ctrl Pts',(-4.06398907542679,1.,1.05459645194934));
#47928=CARTESIAN_POINT('Ctrl Pts',(-4.06091239150293,-1.,1.05524507177901));
#47929=CARTESIAN_POINT('Ctrl Pts',(-4.06091239150293,1.,1.05524507177901));
#47930=CARTESIAN_POINT('Ctrl Pts',(-4.05629789308941,-1.,1.0562076270849));
#47931=CARTESIAN_POINT('Ctrl Pts',(-4.05629789308941,1.,1.0562076270849));
#47932=CARTESIAN_POINT('Ctrl Pts',(-4.05014628387112,-1.,1.05747027728537));
#47933=CARTESIAN_POINT('Ctrl Pts',(-4.05014628387112,1.,1.05747027728537));
#47934=CARTESIAN_POINT('Ctrl Pts',(-4.04245854429333,-1.,1.05901393667039));
#47935=CARTESIAN_POINT('Ctrl Pts',(-4.04245854429333,1.,1.05901393667039));
#47936=CARTESIAN_POINT('Ctrl Pts',(-4.03477261142549,-1.,1.06052284712114));
#47937=CARTESIAN_POINT('Ctrl Pts',(-4.03477261142549,1.,1.06052284712114));
#47938=CARTESIAN_POINT('Ctrl Pts',(-4.02708855235732,-1.,1.06199687787488));
#47939=CARTESIAN_POINT('Ctrl Pts',(-4.02708855235732,1.,1.06199687787488));
#47940=CARTESIAN_POINT('Ctrl Pts',(-4.0194064749539,-1.,1.06343586496094));
#47941=CARTESIAN_POINT('Ctrl Pts',(-4.0194064749539,1.,1.06343586496094));
#47942=CARTESIAN_POINT('Ctrl Pts',(-4.0117265418656,-1.,1.06483961342894));
#47943=CARTESIAN_POINT('Ctrl Pts',(-4.0117265418656,1.,1.06483961342894));
#47944=CARTESIAN_POINT('Ctrl Pts',(-4.00404894951804,-1.,1.06620789963406));
#47945=CARTESIAN_POINT('Ctrl Pts',(-4.00404894951804,1.,1.06620789963406));
#47946=CARTESIAN_POINT('Ctrl Pts',(-3.99637389919958,-1.,1.06754047381188));
#47947=CARTESIAN_POINT('Ctrl Pts',(-3.99637389919958,1.,1.06754047381188));
#47948=CARTESIAN_POINT('Ctrl Pts',(-3.98870156857298,-1.,1.06883706263912));
#47949=CARTESIAN_POINT('Ctrl Pts',(-3.98870156857298,1.,1.06883706263912));
#47950=CARTESIAN_POINT('Ctrl Pts',(-3.98103208801289,-1.,1.07009737257815));
#47951=CARTESIAN_POINT('Ctrl Pts',(-3.98103208801289,1.,1.07009737257815));
#47952=CARTESIAN_POINT('Ctrl Pts',(-3.97336550222571,-1.,1.07132109206252));
#47953=CARTESIAN_POINT('Ctrl Pts',(-3.97336550222571,1.,1.07132109206252));
#47954=CARTESIAN_POINT('Ctrl Pts',(-3.96570179322681,-1.,1.07250789943095));
#47955=CARTESIAN_POINT('Ctrl Pts',(-3.96570179322681,1.,1.07250789943095));
#47956=CARTESIAN_POINT('Ctrl Pts',(-3.95804094429606,-1.,1.07365747426551));
#47957=CARTESIAN_POINT('Ctrl Pts',(-3.95804094429606,1.,1.07365747426551));
#47958=CARTESIAN_POINT('Ctrl Pts',(-3.95038299600754,-1.,1.07476950921607));
#47959=CARTESIAN_POINT('Ctrl Pts',(-3.95038299600754,1.,1.07476950921607));
#47960=CARTESIAN_POINT('Ctrl Pts',(-3.94272809633271,-1.,1.07584371946428));
#47961=CARTESIAN_POINT('Ctrl Pts',(-3.94272809633271,1.,1.07584371946428));
#47962=CARTESIAN_POINT('Ctrl Pts',(-3.93507657572743,-1.,1.07687985975348));
#47963=CARTESIAN_POINT('Ctrl Pts',(-3.93507657572743,1.,1.07687985975348));
#47964=CARTESIAN_POINT('Ctrl Pts',(-3.92742893349684,-1.,1.07787771707155));
#47965=CARTESIAN_POINT('Ctrl Pts',(-3.92742893349684,1.,1.07787771707155));
#47966=CARTESIAN_POINT('Ctrl Pts',(-3.91978568924062,-1.,1.07883706663524));
#47967=CARTESIAN_POINT('Ctrl Pts',(-3.91978568924062,1.,1.07883706663524));
#47968=CARTESIAN_POINT('Ctrl Pts',(-3.91214726022096,-1.,1.0797576350746));
#47969=CARTESIAN_POINT('Ctrl Pts',(-3.91214726022096,1.,1.0797576350746));
#47970=CARTESIAN_POINT('Ctrl Pts',(-3.90451384092564,-1.,1.08063906483822));
#47971=CARTESIAN_POINT('Ctrl Pts',(-3.90451384092564,1.,1.08063906483822));
#47972=CARTESIAN_POINT('Ctrl Pts',(-3.89688525098408,-1.,1.08148086931373));
#47973=CARTESIAN_POINT('Ctrl Pts',(-3.89688525098408,1.,1.08148086931373));
#47974=CARTESIAN_POINT('Ctrl Pts',(-3.88926088975182,-1.,1.08228241999363));
#47975=CARTESIAN_POINT('Ctrl Pts',(-3.88926088975182,1.,1.08228241999363));
#47976=CARTESIAN_POINT('Ctrl Pts',(-3.88164007721365,-1.,1.08304304871042));
#47977=CARTESIAN_POINT('Ctrl Pts',(-3.88164007721365,1.,1.08304304871042));
#47978=CARTESIAN_POINT('Ctrl Pts',(-3.87402233722563,-1.,1.0837621330751));
#47979=CARTESIAN_POINT('Ctrl Pts',(-3.87402233722563,1.,1.0837621330751));
#47980=CARTESIAN_POINT('Ctrl Pts',(-3.86640769434269,-1.,1.08443918607926));
#47981=CARTESIAN_POINT('Ctrl Pts',(-3.86640769434269,1.,1.08443918607926));
#47982=CARTESIAN_POINT('Ctrl Pts',(-3.85879698702511,-1.,1.08507395120054));
#47983=CARTESIAN_POINT('Ctrl Pts',(-3.85879698702511,1.,1.08507395120054));
#47984=CARTESIAN_POINT('Ctrl Pts',(-3.85119211322732,-1.,1.08566647671838));
#47985=CARTESIAN_POINT('Ctrl Pts',(-3.85119211322732,1.,1.08566647671838));
#47986=CARTESIAN_POINT('Ctrl Pts',(-3.84359528764934,-1.,1.08621688337601));
#47987=CARTESIAN_POINT('Ctrl Pts',(-3.84359528764934,1.,1.08621688337601));
#47988=CARTESIAN_POINT('Ctrl Pts',(-3.83600837071702,-1.,1.08672515456901));
#47989=CARTESIAN_POINT('Ctrl Pts',(-3.83600837071702,1.,1.08672515456901));
#47990=CARTESIAN_POINT('Ctrl Pts',(-3.82843215316985,-1.,1.08719091307558));
#47991=CARTESIAN_POINT('Ctrl Pts',(-3.82843215316985,1.,1.08719091307558));
#47992=CARTESIAN_POINT('Ctrl Pts',(-3.82086569676321,-1.,1.08761321539442));
#47993=CARTESIAN_POINT('Ctrl Pts',(-3.82086569676321,1.,1.08761321539442));
#47994=CARTESIAN_POINT('Ctrl Pts',(-3.81330554446324,-1.,1.08799030610861));
#47995=CARTESIAN_POINT('Ctrl Pts',(-3.81330554446324,1.,1.08799030610861));
#47996=CARTESIAN_POINT('Ctrl Pts',(-3.80574726657656,-1.,1.08832009255378));
#47997=CARTESIAN_POINT('Ctrl Pts',(-3.80574726657656,1.,1.08832009255378));
#47998=CARTESIAN_POINT('Ctrl Pts',(-3.79818708705252,-1.,1.08860064435776));
#47999=CARTESIAN_POINT('Ctrl Pts',(-3.79818708705252,1.,1.08860064435776));
#48000=CARTESIAN_POINT('Ctrl Pts',(-3.79062357974401,-1.,1.08883071512097));
#48001=CARTESIAN_POINT('Ctrl Pts',(-3.79062357974401,1.,1.08883071512097));
#48002=CARTESIAN_POINT('Ctrl Pts',(-3.78305911299511,-1.,1.08901018614638));
#48003=CARTESIAN_POINT('Ctrl Pts',(-3.78305911299511,1.,1.08901018614638));
#48004=CARTESIAN_POINT('Ctrl Pts',(-3.7755019940944,-1.,1.08914072791275));
#48005=CARTESIAN_POINT('Ctrl Pts',(-3.7755019940944,1.,1.08914072791275));
#48006=CARTESIAN_POINT('Ctrl Pts',(-3.76796340094469,-1.,1.08922484204263));
#48007=CARTESIAN_POINT('Ctrl Pts',(-3.76796340094469,1.,1.08922484204263));
#48008=CARTESIAN_POINT('Ctrl Pts',(-3.76045342580226,-1.,1.08926462734287));
#48009=CARTESIAN_POINT('Ctrl Pts',(-3.76045342580226,1.,1.08926462734287));
#48010=CARTESIAN_POINT('Ctrl Pts',(-3.75297711748138,-1.,1.08926054632927));
#48011=CARTESIAN_POINT('Ctrl Pts',(-3.75297711748138,1.,1.08926054632927));
#48012=CARTESIAN_POINT('Ctrl Pts',(-3.74553121371745,-1.,1.08921040494013));
#48013=CARTESIAN_POINT('Ctrl Pts',(-3.74553121371745,1.,1.08921040494013));
#48014=CARTESIAN_POINT('Ctrl Pts',(-3.73809879348209,-1.,1.08910769013288));
#48015=CARTESIAN_POINT('Ctrl Pts',(-3.73809879348209,1.,1.08910769013288));
#48016=CARTESIAN_POINT('Ctrl Pts',(-3.73065515162949,-1.,1.08894337390925));
#48017=CARTESIAN_POINT('Ctrl Pts',(-3.73065515162949,1.,1.08894337390925));
#48018=CARTESIAN_POINT('Ctrl Pts',(-3.72317741369364,-1.,1.08870887220072));
#48019=CARTESIAN_POINT('Ctrl Pts',(-3.72317741369364,1.,1.08870887220072));
#48020=CARTESIAN_POINT('Ctrl Pts',(-3.71565372339063,-1.,1.08839887334776));
#48021=CARTESIAN_POINT('Ctrl Pts',(-3.71565372339063,1.,1.08839887334776));
#48022=CARTESIAN_POINT('Ctrl Pts',(-3.70809084139476,-1.,1.0880136731219));
#48023=CARTESIAN_POINT('Ctrl Pts',(-3.70809084139476,1.,1.0880136731219));
#48024=CARTESIAN_POINT('Ctrl Pts',(-3.70052690909884,-1.,1.08756311291324));
#48025=CARTESIAN_POINT('Ctrl Pts',(-3.70052690909884,1.,1.08756311291324));
#48026=CARTESIAN_POINT('Ctrl Pts',(-3.69302062410229,-1.,1.08706319540291));
#48027=CARTESIAN_POINT('Ctrl Pts',(-3.69302062410229,1.,1.08706319540291));
#48028=CARTESIAN_POINT('Ctrl Pts',(-3.68562817420864,-1.,1.08652888882609));
#48029=CARTESIAN_POINT('Ctrl Pts',(-3.68562817420864,1.,1.08652888882609));
#48030=CARTESIAN_POINT('Ctrl Pts',(-3.67838211685148,-1.,1.08596755755768));
#48031=CARTESIAN_POINT('Ctrl Pts',(-3.67838211685148,1.,1.08596755755768));
#48032=CARTESIAN_POINT('Ctrl Pts',(-3.67127347729632,-1.,1.0853733414448));
#48033=CARTESIAN_POINT('Ctrl Pts',(-3.67127347729632,1.,1.0853733414448));
#48034=CARTESIAN_POINT('Ctrl Pts',(-3.66422237895256,-1.,1.0847180992287));
#48035=CARTESIAN_POINT('Ctrl Pts',(-3.66422237895256,1.,1.0847180992287));
#48036=CARTESIAN_POINT('Ctrl Pts',(-3.65709649161004,-1.,1.08395671077761));
#48037=CARTESIAN_POINT('Ctrl Pts',(-3.65709649161004,1.,1.08395671077761));
#48038=CARTESIAN_POINT('Ctrl Pts',(-3.64976441208197,-1.,1.08304289898577));
#48039=CARTESIAN_POINT('Ctrl Pts',(-3.64976441208197,1.,1.08304289898577));
#48040=CARTESIAN_POINT('Ctrl Pts',(-3.64214167843595,-1.,1.08194278850972));
#48041=CARTESIAN_POINT('Ctrl Pts',(-3.64214167843595,1.,1.08194278850972));
#48042=CARTESIAN_POINT('Ctrl Pts',(-3.63423373196602,-1.,1.08064765719887));
#48043=CARTESIAN_POINT('Ctrl Pts',(-3.63423373196602,1.,1.08064765719887));
#48044=CARTESIAN_POINT('Ctrl Pts',(-3.62619537902616,-1.,1.07919137290815));
#48045=CARTESIAN_POINT('Ctrl Pts',(-3.62619537902616,1.,1.07919137290815));
#48046=CARTESIAN_POINT('Ctrl Pts',(-3.61832318504957,-1.,1.07764868137729));
#48047=CARTESIAN_POINT('Ctrl Pts',(-3.61832318504957,1.,1.07764868137729));
#48048=CARTESIAN_POINT('Ctrl Pts',(-3.61098481349577,-1.,1.07611545402841));
#48049=CARTESIAN_POINT('Ctrl Pts',(-3.61098481349577,1.,1.07611545402841));
#48050=CARTESIAN_POINT('Ctrl Pts',(-3.6045633988796,-1.,1.0746932716863));
#48051=CARTESIAN_POINT('Ctrl Pts',(-3.6045633988796,1.,1.0746932716863));
#48052=CARTESIAN_POINT('Ctrl Pts',(-3.59940121154383,-1.,1.0734737254567));
#48053=CARTESIAN_POINT('Ctrl Pts',(-3.59940121154383,1.,1.0734737254567));
#48054=CARTESIAN_POINT('Ctrl Pts',(-3.59573039611837,-1.,1.07251922679108));
#48055=CARTESIAN_POINT('Ctrl Pts',(-3.59573039611837,1.,1.07251922679108));
#48056=CARTESIAN_POINT('Ctrl Pts',(-3.59407399103556,-1.,1.07199116987503));
#48057=CARTESIAN_POINT('Ctrl Pts',(-3.59407399103556,1.,1.07199116987503));
#48058=CARTESIAN_POINT('Ctrl Pts',(-3.59356848057451,-1.,1.07173216219041));
#48059=CARTESIAN_POINT('Ctrl Pts',(-3.59356848057451,1.,1.07173216219041));
#48060=CARTESIAN_POINT('Ctrl Pts',(-3.59355870577763,-1.,1.07162034256419));
#48061=CARTESIAN_POINT('Ctrl Pts',(-3.59355870577763,1.,1.07162034256419));
#48062=CARTESIAN_POINT('Ctrl Pts',(-3.59363563249864,-1.,1.07157964745328));
#48063=CARTESIAN_POINT('Ctrl Pts',(-3.59363563249864,1.,1.07157964745328));
#48064=CARTESIAN_POINT('',(-4.06552750530042,1.,1.05427041296137));
#48065=CARTESIAN_POINT('Ctrl Pts',(-4.06552750530042,1.,1.05427041296137));
#48066=CARTESIAN_POINT('Ctrl Pts',(-4.06398907542679,1.,1.05459645194934));
#48067=CARTESIAN_POINT('Ctrl Pts',(-4.06091239150293,1.,1.05524507177901));
#48068=CARTESIAN_POINT('Ctrl Pts',(-4.05629789308941,1.,1.0562076270849));
#48069=CARTESIAN_POINT('Ctrl Pts',(-4.05014628387112,1.,1.05747027728537));
#48070=CARTESIAN_POINT('Ctrl Pts',(-4.04245854429333,1.,1.05901393667039));
#48071=CARTESIAN_POINT('Ctrl Pts',(-4.03477261142549,1.,1.06052284712114));
#48072=CARTESIAN_POINT('Ctrl Pts',(-4.02708855235732,1.,1.06199687787488));
#48073=CARTESIAN_POINT('Ctrl Pts',(-4.0194064749539,1.,1.06343586496094));
#48074=CARTESIAN_POINT('Ctrl Pts',(-4.0117265418656,1.,1.06483961342894));
#48075=CARTESIAN_POINT('Ctrl Pts',(-4.00404894951804,1.,1.06620789963406));
#48076=CARTESIAN_POINT('Ctrl Pts',(-3.99637389919958,1.,1.06754047381188));
#48077=CARTESIAN_POINT('Ctrl Pts',(-3.98870156857298,1.,1.06883706263912));
#48078=CARTESIAN_POINT('Ctrl Pts',(-3.98103208801289,1.,1.07009737257815));
#48079=CARTESIAN_POINT('Ctrl Pts',(-3.97336550222571,1.,1.07132109206252));
#48080=CARTESIAN_POINT('Ctrl Pts',(-3.96570179322681,1.,1.07250789943095));
#48081=CARTESIAN_POINT('Ctrl Pts',(-3.95804094429606,1.,1.07365747426551));
#48082=CARTESIAN_POINT('Ctrl Pts',(-3.95038299600754,1.,1.07476950921607));
#48083=CARTESIAN_POINT('Ctrl Pts',(-3.94272809633271,1.,1.07584371946428));
#48084=CARTESIAN_POINT('Ctrl Pts',(-3.93507657572743,1.,1.07687985975348));
#48085=CARTESIAN_POINT('Ctrl Pts',(-3.92742893349684,1.,1.07787771707155));
#48086=CARTESIAN_POINT('Ctrl Pts',(-3.91978568924062,1.,1.07883706663524));
#48087=CARTESIAN_POINT('Ctrl Pts',(-3.91214726022096,1.,1.0797576350746));
#48088=CARTESIAN_POINT('Ctrl Pts',(-3.90451384092564,1.,1.08063906483822));
#48089=CARTESIAN_POINT('Ctrl Pts',(-3.89688525098408,1.,1.08148086931373));
#48090=CARTESIAN_POINT('Ctrl Pts',(-3.88926088975182,1.,1.08228241999363));
#48091=CARTESIAN_POINT('Ctrl Pts',(-3.88164007721365,1.,1.08304304871042));
#48092=CARTESIAN_POINT('Ctrl Pts',(-3.87402233722563,1.,1.0837621330751));
#48093=CARTESIAN_POINT('Ctrl Pts',(-3.86640769434269,1.,1.08443918607926));
#48094=CARTESIAN_POINT('Ctrl Pts',(-3.85879698702511,1.,1.08507395120054));
#48095=CARTESIAN_POINT('Ctrl Pts',(-3.85119211322732,1.,1.08566647671838));
#48096=CARTESIAN_POINT('Ctrl Pts',(-3.84359528764934,1.,1.08621688337601));
#48097=CARTESIAN_POINT('Ctrl Pts',(-3.83600837071702,1.,1.08672515456901));
#48098=CARTESIAN_POINT('Ctrl Pts',(-3.82843215316985,1.,1.08719091307558));
#48099=CARTESIAN_POINT('Ctrl Pts',(-3.82086569676321,1.,1.08761321539442));
#48100=CARTESIAN_POINT('Ctrl Pts',(-3.81330554446324,1.,1.08799030610861));
#48101=CARTESIAN_POINT('Ctrl Pts',(-3.80574726657656,1.,1.08832009255378));
#48102=CARTESIAN_POINT('Ctrl Pts',(-3.79818708705252,1.,1.08860064435776));
#48103=CARTESIAN_POINT('Ctrl Pts',(-3.79062357974401,1.,1.08883071512097));
#48104=CARTESIAN_POINT('Ctrl Pts',(-3.78305911299511,1.,1.08901018614638));
#48105=CARTESIAN_POINT('Ctrl Pts',(-3.7755019940944,1.,1.08914072791275));
#48106=CARTESIAN_POINT('Ctrl Pts',(-3.76796340094469,1.,1.08922484204263));
#48107=CARTESIAN_POINT('Ctrl Pts',(-3.76045342580226,1.,1.08926462734287));
#48108=CARTESIAN_POINT('Ctrl Pts',(-3.75297711748138,1.,1.08926054632927));
#48109=CARTESIAN_POINT('Ctrl Pts',(-3.74553121371745,1.,1.08921040494013));
#48110=CARTESIAN_POINT('Ctrl Pts',(-3.73809879348209,1.,1.08910769013288));
#48111=CARTESIAN_POINT('Ctrl Pts',(-3.73065515162949,1.,1.08894337390925));
#48112=CARTESIAN_POINT('Ctrl Pts',(-3.72317741369364,1.,1.08870887220072));
#48113=CARTESIAN_POINT('Ctrl Pts',(-3.71565372339063,1.,1.08839887334776));
#48114=CARTESIAN_POINT('Ctrl Pts',(-3.70809084139476,1.,1.0880136731219));
#48115=CARTESIAN_POINT('Ctrl Pts',(-3.70052690909884,1.,1.08756311291324));
#48116=CARTESIAN_POINT('Ctrl Pts',(-3.69302062410229,1.,1.08706319540291));
#48117=CARTESIAN_POINT('Ctrl Pts',(-3.68562817420864,1.,1.08652888882609));
#48118=CARTESIAN_POINT('Ctrl Pts',(-3.67838211685148,1.,1.08596755755768));
#48119=CARTESIAN_POINT('Ctrl Pts',(-3.67127347729632,1.,1.0853733414448));
#48120=CARTESIAN_POINT('Ctrl Pts',(-3.66422237895256,1.,1.0847180992287));
#48121=CARTESIAN_POINT('Ctrl Pts',(-3.65709649161004,1.,1.08395671077761));
#48122=CARTESIAN_POINT('Ctrl Pts',(-3.64976441208197,1.,1.08304289898577));
#48123=CARTESIAN_POINT('Ctrl Pts',(-3.64214167843595,1.,1.08194278850972));
#48124=CARTESIAN_POINT('Ctrl Pts',(-3.63423373196602,1.,1.08064765719887));
#48125=CARTESIAN_POINT('Ctrl Pts',(-3.62619537902616,1.,1.07919137290815));
#48126=CARTESIAN_POINT('Ctrl Pts',(-3.61832318504957,1.,1.07764868137729));
#48127=CARTESIAN_POINT('Ctrl Pts',(-3.61098481349577,1.,1.07611545402841));
#48128=CARTESIAN_POINT('Ctrl Pts',(-3.6045633988796,1.,1.0746932716863));
#48129=CARTESIAN_POINT('Ctrl Pts',(-3.59940121154383,1.,1.0734737254567));
#48130=CARTESIAN_POINT('Ctrl Pts',(-3.59600583195037,1.,1.07259084660947));
#48131=CARTESIAN_POINT('Ctrl Pts',(-3.59439597,1.,1.07209229745284));
#48132=CARTESIAN_POINT('Ctrl Pts',(-3.59379266874663,1.,1.07183575450716));
#48133=CARTESIAN_POINT('Ctrl Pts',(-3.59363512797985,1.,1.07171709254271));
#48134=CARTESIAN_POINT('Ctrl Pts',(-3.59360648251021,1.,1.071677399622));
#48135=CARTESIAN_POINT('',(-4.06552750530042,0.,1.05427041296137));
#48136=CARTESIAN_POINT('Ctrl Pts',(-3.68843977377012,-1.,0.676691979611561));
#48137=CARTESIAN_POINT('Ctrl Pts',(-3.68843977377012,1.,0.676691979611561));
#48138=CARTESIAN_POINT('Ctrl Pts',(-3.68838970675497,-1.,0.676620796001989));
#48139=CARTESIAN_POINT('Ctrl Pts',(-3.68838970675497,1.,0.676620796001989));
#48140=CARTESIAN_POINT('Ctrl Pts',(-3.68844918121303,-1.,0.676525601650855));
#48141=CARTESIAN_POINT('Ctrl Pts',(-3.68844918121303,1.,0.676525601650855));
#48142=CARTESIAN_POINT('Ctrl Pts',(-3.68901718136181,-1.,0.676524321061226));
#48143=CARTESIAN_POINT('Ctrl Pts',(-3.68901718136181,1.,0.676524321061226));
#48144=CARTESIAN_POINT('Ctrl Pts',(-3.69073278191994,-1.,0.67680581107509));
#48145=CARTESIAN_POINT('Ctrl Pts',(-3.69073278191994,1.,0.67680581107509));
#48146=CARTESIAN_POINT('Ctrl Pts',(-3.69443683573598,-1.,0.677621861865498));
#48147=CARTESIAN_POINT('Ctrl Pts',(-3.69443683573598,1.,0.677621861865498));
#48148=CARTESIAN_POINT('Ctrl Pts',(-3.69959004073005,-1.,0.678878822226026));
#48149=CARTESIAN_POINT('Ctrl Pts',(-3.69959004073005,1.,0.678878822226026));
#48150=CARTESIAN_POINT('Ctrl Pts',(-3.70595722031785,-1.,0.680526909710877));
#48151=CARTESIAN_POINT('Ctrl Pts',(-3.70595722031785,1.,0.680526909710877));
#48152=CARTESIAN_POINT('Ctrl Pts',(-3.71319182789943,-1.,0.68249234510893));
#48153=CARTESIAN_POINT('Ctrl Pts',(-3.71319182789943,1.,0.68249234510893));
#48154=CARTESIAN_POINT('Ctrl Pts',(-3.7209063713926,-1.,0.684691698167848));
#48155=CARTESIAN_POINT('Ctrl Pts',(-3.7209063713926,1.,0.684691698167848));
#48156=CARTESIAN_POINT('Ctrl Pts',(-3.72872973554051,-1.,0.687043475232354));
#48157=CARTESIAN_POINT('Ctrl Pts',(-3.72872973554051,1.,0.687043475232354));
#48158=CARTESIAN_POINT('Ctrl Pts',(-3.73636374475077,-1.,0.689479637354813));
#48159=CARTESIAN_POINT('Ctrl Pts',(-3.73636374475077,1.,0.689479637354813));
#48160=CARTESIAN_POINT('Ctrl Pts',(-3.74365508986712,-1.,0.69196008040082));
#48161=CARTESIAN_POINT('Ctrl Pts',(-3.74365508986712,1.,0.69196008040082));
#48162=CARTESIAN_POINT('Ctrl Pts',(-3.75060288243455,-1.,0.694474562581492));
#48163=CARTESIAN_POINT('Ctrl Pts',(-3.75060288243455,1.,0.694474562581492));
#48164=CARTESIAN_POINT('Ctrl Pts',(-3.75729775767023,-1.,0.697031245659743));
#48165=CARTESIAN_POINT('Ctrl Pts',(-3.75729775767023,1.,0.697031245659743));
#48166=CARTESIAN_POINT('Ctrl Pts',(-3.76387780603759,-1.,0.699648552230917));
#48167=CARTESIAN_POINT('Ctrl Pts',(-3.76387780603759,1.,0.699648552230917));
#48168=CARTESIAN_POINT('Ctrl Pts',(-3.77048141872872,-1.,0.702346356621551));
#48169=CARTESIAN_POINT('Ctrl Pts',(-3.77048141872872,1.,0.702346356621551));
#48170=CARTESIAN_POINT('Ctrl Pts',(-3.77719254217129,-1.,0.705135847999816));
#48171=CARTESIAN_POINT('Ctrl Pts',(-3.77719254217129,1.,0.705135847999816));
#48172=CARTESIAN_POINT('Ctrl Pts',(-3.78402183336605,-1.,0.708015879375459));
#48173=CARTESIAN_POINT('Ctrl Pts',(-3.78402183336605,1.,0.708015879375459));
#48174=CARTESIAN_POINT('Ctrl Pts',(-3.79093694007094,-1.,0.710978231689017));
#48175=CARTESIAN_POINT('Ctrl Pts',(-3.79093694007094,1.,0.710978231689017));
#48176=CARTESIAN_POINT('Ctrl Pts',(-3.79788100314975,-1.,0.71401073300664));
#48177=CARTESIAN_POINT('Ctrl Pts',(-3.79788100314975,1.,0.71401073300664));
#48178=CARTESIAN_POINT('Ctrl Pts',(-3.80479445759309,-1.,0.717100993669114));
#48179=CARTESIAN_POINT('Ctrl Pts',(-3.80479445759309,1.,0.717100993669114));
#48180=CARTESIAN_POINT('Ctrl Pts',(-3.81163885127344,-1.,0.720240466589236));
#48181=CARTESIAN_POINT('Ctrl Pts',(-3.81163885127344,1.,0.720240466589236));
#48182=CARTESIAN_POINT('Ctrl Pts',(-3.81840802610835,-1.,0.723426346019422));
#48183=CARTESIAN_POINT('Ctrl Pts',(-3.81840802610835,1.,0.723426346019422));
#48184=CARTESIAN_POINT('Ctrl Pts',(-3.82511495756713,-1.,0.726659281876664));
#48185=CARTESIAN_POINT('Ctrl Pts',(-3.82511495756713,1.,0.726659281876664));
#48186=CARTESIAN_POINT('Ctrl Pts',(-3.83178392403383,-1.,0.729942010490167));
#48187=CARTESIAN_POINT('Ctrl Pts',(-3.83178392403383,1.,0.729942010490167));
#48188=CARTESIAN_POINT('Ctrl Pts',(-3.83844103658009,-1.,0.733277703756078));
#48189=CARTESIAN_POINT('Ctrl Pts',(-3.83844103658009,1.,0.733277703756078));
#48190=CARTESIAN_POINT('Ctrl Pts',(-3.84510432881213,-1.,0.736668240497117));
#48191=CARTESIAN_POINT('Ctrl Pts',(-3.84510432881213,1.,0.736668240497117));
#48192=CARTESIAN_POINT('Ctrl Pts',(-3.85177770351216,-1.,0.740113146827137));
#48193=CARTESIAN_POINT('Ctrl Pts',(-3.85177770351216,1.,0.740113146827137));
#48194=CARTESIAN_POINT('Ctrl Pts',(-3.85845645217594,-1.,0.743610542737012));
#48195=CARTESIAN_POINT('Ctrl Pts',(-3.85845645217594,1.,0.743610542737012));
#48196=CARTESIAN_POINT('Ctrl Pts',(-3.86513062969889,-1.,0.747157716488871));
#48197=CARTESIAN_POINT('Ctrl Pts',(-3.86513062969889,1.,0.747157716488871));
#48198=CARTESIAN_POINT('Ctrl Pts',(-3.87178914078374,-1.,0.750751822383027));
#48199=CARTESIAN_POINT('Ctrl Pts',(-3.87178914078374,1.,0.750751822383027));
#48200=CARTESIAN_POINT('Ctrl Pts',(-3.87842382520065,-1.,0.754390577396856));
#48201=CARTESIAN_POINT('Ctrl Pts',(-3.87842382520065,1.,0.754390577396856));
#48202=CARTESIAN_POINT('Ctrl Pts',(-3.88503262662689,-1.,0.758072800564801));
#48203=CARTESIAN_POINT('Ctrl Pts',(-3.88503262662689,1.,0.758072800564801));
#48204=CARTESIAN_POINT('Ctrl Pts',(-3.89161738162245,-1.,0.761798028793969));
#48205=CARTESIAN_POINT('Ctrl Pts',(-3.89161738162245,1.,0.761798028793969));
#48206=CARTESIAN_POINT('Ctrl Pts',(-3.89818233104378,-1.,0.765566256401295));
#48207=CARTESIAN_POINT('Ctrl Pts',(-3.89818233104378,1.,0.765566256401295));
#48208=CARTESIAN_POINT('Ctrl Pts',(-3.90473237182633,-1.,0.769377629847874));
#48209=CARTESIAN_POINT('Ctrl Pts',(-3.90473237182633,1.,0.769377629847874));
#48210=CARTESIAN_POINT('Ctrl Pts',(-3.91127138115243,-1.,0.773232154506321));
#48211=CARTESIAN_POINT('Ctrl Pts',(-3.91127138115243,1.,0.773232154506321));
#48212=CARTESIAN_POINT('Ctrl Pts',(-3.9178006233448,-1.,0.777129415664956));
#48213=CARTESIAN_POINT('Ctrl Pts',(-3.9178006233448,1.,0.777129415664956));
#48214=CARTESIAN_POINT('Ctrl Pts',(-3.92431956510441,-1.,0.781068718228451));
#48215=CARTESIAN_POINT('Ctrl Pts',(-3.92431956510441,1.,0.781068718228451));
#48216=CARTESIAN_POINT('Ctrl Pts',(-3.93082655631789,-1.,0.785049202786507));
#48217=CARTESIAN_POINT('Ctrl Pts',(-3.93082655631789,1.,0.785049202786507));
#48218=CARTESIAN_POINT('Ctrl Pts',(-3.93731956885676,-1.,0.789069971469333));
#48219=CARTESIAN_POINT('Ctrl Pts',(-3.93731956885676,1.,0.789069971469333));
#48220=CARTESIAN_POINT('Ctrl Pts',(-3.94379688971283,-1.,0.793130205640961));
#48221=CARTESIAN_POINT('Ctrl Pts',(-3.94379688971283,1.,0.793130205640961));
#48222=CARTESIAN_POINT('Ctrl Pts',(-3.95025788827136,-1.,0.797229296085315));
#48223=CARTESIAN_POINT('Ctrl Pts',(-3.95025788827136,1.,0.797229296085315));
#48224=CARTESIAN_POINT('Ctrl Pts',(-3.95670276375108,-1.,0.801366797727049));
#48225=CARTESIAN_POINT('Ctrl Pts',(-3.95670276375108,1.,0.801366797727049));
#48226=CARTESIAN_POINT('Ctrl Pts',(-3.96313222295815,-1.,0.805542372178361));
#48227=CARTESIAN_POINT('Ctrl Pts',(-3.96313222295815,1.,0.805542372178361));
#48228=CARTESIAN_POINT('Ctrl Pts',(-3.96954717513232,-1.,0.80975573281809));
#48229=CARTESIAN_POINT('Ctrl Pts',(-3.96954717513232,1.,0.80975573281809));
#48230=CARTESIAN_POINT('Ctrl Pts',(-3.97594844078811,-1.,0.814006592328843));
#48231=CARTESIAN_POINT('Ctrl Pts',(-3.97594844078811,1.,0.814006592328843));
#48232=CARTESIAN_POINT('Ctrl Pts',(-3.98233640155404,-1.,0.818294599022293));
#48233=CARTESIAN_POINT('Ctrl Pts',(-3.98233640155404,1.,0.818294599022293));
#48234=CARTESIAN_POINT('Ctrl Pts',(-3.98871104646485,-1.,0.822619346022119));
#48235=CARTESIAN_POINT('Ctrl Pts',(-3.98871104646485,1.,0.822619346022119));
#48236=CARTESIAN_POINT('Ctrl Pts',(-3.99507212784431,-1.,0.826980400320789));
#48237=CARTESIAN_POINT('Ctrl Pts',(-3.99507212784431,1.,0.826980400320789));
#48238=CARTESIAN_POINT('Ctrl Pts',(-4.00141928477507,-1.,0.831377325741622));
#48239=CARTESIAN_POINT('Ctrl Pts',(-4.00141928477507,1.,0.831377325741622));
#48240=CARTESIAN_POINT('Ctrl Pts',(-4.00775216907856,-1.,0.835809705809646));
#48241=CARTESIAN_POINT('Ctrl Pts',(-4.00775216907856,1.,0.835809705809646));
#48242=CARTESIAN_POINT('Ctrl Pts',(-4.01407059766103,-1.,0.840277171975855));
#48243=CARTESIAN_POINT('Ctrl Pts',(-4.01407059766103,1.,0.840277171975855));
#48244=CARTESIAN_POINT('Ctrl Pts',(-4.02037456798441,-1.,0.844779403287745));
#48245=CARTESIAN_POINT('Ctrl Pts',(-4.02037456798441,1.,0.844779403287745));
#48246=CARTESIAN_POINT('Ctrl Pts',(-4.02666418343164,-1.,0.849316107474245));
#48247=CARTESIAN_POINT('Ctrl Pts',(-4.02666418343164,1.,0.849316107474245));
#48248=CARTESIAN_POINT('Ctrl Pts',(-4.03293960436756,-1.,0.853887006631755));
#48249=CARTESIAN_POINT('Ctrl Pts',(-4.03293960436756,1.,0.853887006631755));
#48250=CARTESIAN_POINT('Ctrl Pts',(-4.03920099284773,-1.,0.858491822322827));
#48251=CARTESIAN_POINT('Ctrl Pts',(-4.03920099284773,1.,0.858491822322827));
#48252=CARTESIAN_POINT('Ctrl Pts',(-4.04544845048584,-1.,0.863130256643259));
#48253=CARTESIAN_POINT('Ctrl Pts',(-4.04544845048584,1.,0.863130256643259));
#48254=CARTESIAN_POINT('Ctrl Pts',(-4.05168199437909,-1.,0.867801988859917));
#48255=CARTESIAN_POINT('Ctrl Pts',(-4.05168199437909,1.,0.867801988859917));
#48256=CARTESIAN_POINT('Ctrl Pts',(-4.0579015903134,-1.,0.872506694782446));
#48257=CARTESIAN_POINT('Ctrl Pts',(-4.0579015903134,1.,0.872506694782446));
#48258=CARTESIAN_POINT('Ctrl Pts',(-4.06410717232905,-1.,0.877244060485837));
#48259=CARTESIAN_POINT('Ctrl Pts',(-4.06410717232905,1.,0.877244060485837));
#48260=CARTESIAN_POINT('Ctrl Pts',(-4.07029866694192,-1.,0.882013797525692));
#48261=CARTESIAN_POINT('Ctrl Pts',(-4.07029866694192,1.,0.882013797525692));
#48262=CARTESIAN_POINT('Ctrl Pts',(-4.07647601773635,-1.,0.886815658358501));
#48263=CARTESIAN_POINT('Ctrl Pts',(-4.07647601773635,1.,0.886815658358501));
#48264=CARTESIAN_POINT('Ctrl Pts',(-4.08263920304799,-1.,0.891649447916277));
#48265=CARTESIAN_POINT('Ctrl Pts',(-4.08263920304799,1.,0.891649447916277));
#48266=CARTESIAN_POINT('Ctrl Pts',(-4.08878822246833,-1.,0.896515019231333));
#48267=CARTESIAN_POINT('Ctrl Pts',(-4.08878822246833,1.,0.896515019231333));
#48268=CARTESIAN_POINT('Ctrl Pts',(-4.09369611522387,-1.,0.900432820941674));
#48269=CARTESIAN_POINT('Ctrl Pts',(-4.09369611522387,1.,0.900432820941674));
#48270=CARTESIAN_POINT('Ctrl Pts',(-4.09737067245935,-1.,0.903385402441587));
#48271=CARTESIAN_POINT('Ctrl Pts',(-4.09737067245935,1.,0.903385402441587));
#48272=CARTESIAN_POINT('Ctrl Pts',(-4.09981755067523,-1.,0.905360112215337));
#48273=CARTESIAN_POINT('Ctrl Pts',(-4.09981755067523,1.,0.905360112215337));
#48274=CARTESIAN_POINT('Ctrl Pts',(-4.10104028313088,-1.,0.906349047628866));
#48275=CARTESIAN_POINT('Ctrl Pts',(-4.10104028313088,1.,0.906349047628866));
#48276=CARTESIAN_POINT('',(-3.68845817949586,1.,0.676591647975429));
#48277=CARTESIAN_POINT('Ctrl Pts',(-3.68845817949586,-1.,0.676591647975428));
#48278=CARTESIAN_POINT('Ctrl Pts',(-3.68845817949586,-0.666666666666667,
0.676591647975428));
#48279=CARTESIAN_POINT('Ctrl Pts',(-3.68845817949586,-0.333333333333333,
0.676591647975428));
#48280=CARTESIAN_POINT('Ctrl Pts',(-3.68845817949586,0.333333333333333,
0.676591647975428));
#48281=CARTESIAN_POINT('Ctrl Pts',(-3.68845817949586,0.666666666666667,
0.676591647975429));
#48282=CARTESIAN_POINT('Ctrl Pts',(-3.68845817949586,1.,0.676591647975429));
#48283=CARTESIAN_POINT('',(-4.10104028313088,1.,0.906349047628866));
#48284=CARTESIAN_POINT('',(-4.10104028313088,0.,0.906349047628866));
#48285=CARTESIAN_POINT('Ctrl Pts',(-3.68845817949586,1.,0.676591647975428));
#48286=CARTESIAN_POINT('Ctrl Pts',(-3.68850172300477,1.,0.676569286094606));
#48287=CARTESIAN_POINT('Ctrl Pts',(-3.68869596425969,1.,0.676535079520806));
#48288=CARTESIAN_POINT('Ctrl Pts',(-3.68934997767243,1.,0.676580391119396));
#48289=CARTESIAN_POINT('Ctrl Pts',(-3.69101071175464,1.,0.676867042599401));
#48290=CARTESIAN_POINT('Ctrl Pts',(-3.69443683573598,1.,0.677621861865498));
#48291=CARTESIAN_POINT('Ctrl Pts',(-3.69959004073005,1.,0.678878822226026));
#48292=CARTESIAN_POINT('Ctrl Pts',(-3.70595722031785,1.,0.680526909710877));
#48293=CARTESIAN_POINT('Ctrl Pts',(-3.71319182789943,1.,0.68249234510893));
#48294=CARTESIAN_POINT('Ctrl Pts',(-3.7209063713926,1.,0.684691698167848));
#48295=CARTESIAN_POINT('Ctrl Pts',(-3.72872973554051,1.,0.687043475232354));
#48296=CARTESIAN_POINT('Ctrl Pts',(-3.73636374475077,1.,0.689479637354813));
#48297=CARTESIAN_POINT('Ctrl Pts',(-3.74365508986712,1.,0.69196008040082));
#48298=CARTESIAN_POINT('Ctrl Pts',(-3.75060288243455,1.,0.694474562581492));
#48299=CARTESIAN_POINT('Ctrl Pts',(-3.75729775767023,1.,0.697031245659743));
#48300=CARTESIAN_POINT('Ctrl Pts',(-3.76387780603759,1.,0.699648552230917));
#48301=CARTESIAN_POINT('Ctrl Pts',(-3.77048141872872,1.,0.702346356621551));
#48302=CARTESIAN_POINT('Ctrl Pts',(-3.77719254217129,1.,0.705135847999816));
#48303=CARTESIAN_POINT('Ctrl Pts',(-3.78402183336605,1.,0.708015879375459));
#48304=CARTESIAN_POINT('Ctrl Pts',(-3.79093694007094,1.,0.710978231689017));
#48305=CARTESIAN_POINT('Ctrl Pts',(-3.79788100314975,1.,0.71401073300664));
#48306=CARTESIAN_POINT('Ctrl Pts',(-3.80479445759309,1.,0.717100993669114));
#48307=CARTESIAN_POINT('Ctrl Pts',(-3.81163885127344,1.,0.720240466589236));
#48308=CARTESIAN_POINT('Ctrl Pts',(-3.81840802610835,1.,0.723426346019422));
#48309=CARTESIAN_POINT('Ctrl Pts',(-3.82511495756713,1.,0.726659281876664));
#48310=CARTESIAN_POINT('Ctrl Pts',(-3.83178392403383,1.,0.729942010490167));
#48311=CARTESIAN_POINT('Ctrl Pts',(-3.83844103658009,1.,0.733277703756078));
#48312=CARTESIAN_POINT('Ctrl Pts',(-3.84510432881213,1.,0.736668240497117));
#48313=CARTESIAN_POINT('Ctrl Pts',(-3.85177770351216,1.,0.740113146827137));
#48314=CARTESIAN_POINT('Ctrl Pts',(-3.85845645217594,1.,0.743610542737012));
#48315=CARTESIAN_POINT('Ctrl Pts',(-3.86513062969889,1.,0.747157716488871));
#48316=CARTESIAN_POINT('Ctrl Pts',(-3.87178914078374,1.,0.750751822383027));
#48317=CARTESIAN_POINT('Ctrl Pts',(-3.87842382520065,1.,0.754390577396856));
#48318=CARTESIAN_POINT('Ctrl Pts',(-3.88503262662689,1.,0.758072800564801));
#48319=CARTESIAN_POINT('Ctrl Pts',(-3.89161738162245,1.,0.761798028793969));
#48320=CARTESIAN_POINT('Ctrl Pts',(-3.89818233104378,1.,0.765566256401295));
#48321=CARTESIAN_POINT('Ctrl Pts',(-3.90473237182633,1.,0.769377629847874));
#48322=CARTESIAN_POINT('Ctrl Pts',(-3.91127138115243,1.,0.773232154506321));
#48323=CARTESIAN_POINT('Ctrl Pts',(-3.9178006233448,1.,0.777129415664956));
#48324=CARTESIAN_POINT('Ctrl Pts',(-3.92431956510441,1.,0.781068718228451));
#48325=CARTESIAN_POINT('Ctrl Pts',(-3.93082655631789,1.,0.785049202786507));
#48326=CARTESIAN_POINT('Ctrl Pts',(-3.93731956885676,1.,0.789069971469333));
#48327=CARTESIAN_POINT('Ctrl Pts',(-3.94379688971283,1.,0.793130205640961));
#48328=CARTESIAN_POINT('Ctrl Pts',(-3.95025788827136,1.,0.797229296085315));
#48329=CARTESIAN_POINT('Ctrl Pts',(-3.95670276375108,1.,0.801366797727049));
#48330=CARTESIAN_POINT('Ctrl Pts',(-3.96313222295815,1.,0.805542372178361));
#48331=CARTESIAN_POINT('Ctrl Pts',(-3.96954717513232,1.,0.80975573281809));
#48332=CARTESIAN_POINT('Ctrl Pts',(-3.97594844078811,1.,0.814006592328843));
#48333=CARTESIAN_POINT('Ctrl Pts',(-3.98233640155404,1.,0.818294599022293));
#48334=CARTESIAN_POINT('Ctrl Pts',(-3.98871104646485,1.,0.822619346022119));
#48335=CARTESIAN_POINT('Ctrl Pts',(-3.99507212784431,1.,0.826980400320789));
#48336=CARTESIAN_POINT('Ctrl Pts',(-4.00141928477507,1.,0.831377325741622));
#48337=CARTESIAN_POINT('Ctrl Pts',(-4.00775216907856,1.,0.835809705809646));
#48338=CARTESIAN_POINT('Ctrl Pts',(-4.01407059766103,1.,0.840277171975855));
#48339=CARTESIAN_POINT('Ctrl Pts',(-4.02037456798441,1.,0.844779403287745));
#48340=CARTESIAN_POINT('Ctrl Pts',(-4.02666418343164,1.,0.849316107474245));
#48341=CARTESIAN_POINT('Ctrl Pts',(-4.03293960436756,1.,0.853887006631755));
#48342=CARTESIAN_POINT('Ctrl Pts',(-4.03920099284773,1.,0.858491822322827));
#48343=CARTESIAN_POINT('Ctrl Pts',(-4.04544845048584,1.,0.863130256643259));
#48344=CARTESIAN_POINT('Ctrl Pts',(-4.05168199437909,1.,0.867801988859917));
#48345=CARTESIAN_POINT('Ctrl Pts',(-4.0579015903134,1.,0.872506694782446));
#48346=CARTESIAN_POINT('Ctrl Pts',(-4.06410717232905,1.,0.877244060485837));
#48347=CARTESIAN_POINT('Ctrl Pts',(-4.07029866694192,1.,0.882013797525692));
#48348=CARTESIAN_POINT('Ctrl Pts',(-4.07647601773635,1.,0.886815658358501));
#48349=CARTESIAN_POINT('Ctrl Pts',(-4.08263920304799,1.,0.891649447916277));
#48350=CARTESIAN_POINT('Ctrl Pts',(-4.08878822246833,1.,0.896515019231333));
#48351=CARTESIAN_POINT('Ctrl Pts',(-4.09369611522387,1.,0.900432820941674));
#48352=CARTESIAN_POINT('Ctrl Pts',(-4.09737067245935,1.,0.903385402441587));
#48353=CARTESIAN_POINT('Ctrl Pts',(-4.09981755067523,1.,0.905360112215337));
#48354=CARTESIAN_POINT('Ctrl Pts',(-4.10104028313088,1.,0.906349047628866));
#48355=CARTESIAN_POINT('Origin',(-4.10104028313088,0.,0.906349047628866));
#48356=CARTESIAN_POINT('',(-4.06552750530042,1.,1.05427041296137));
#48357=CARTESIAN_POINT('Origin',(0.,0.,0.));
#48358=CARTESIAN_POINT('',(-3.71701050416802,1.,0.496319364829374));
#48359=CARTESIAN_POINT('Origin',(0.,1.,0.));
#48360=CARTESIAN_POINT('Ctrl Pts',(-3.71701050416802,1.,0.496319364829374));
#48361=CARTESIAN_POINT('Ctrl Pts',(-3.71701050416802,0.666666666666667,
0.496319364829374));
#48362=CARTESIAN_POINT('Ctrl Pts',(-3.71701050416802,0.333333333333333,
0.496319364829374));
#48363=CARTESIAN_POINT('Ctrl Pts',(-3.71701050416802,-0.333333333333333,
0.496319364829374));
#48364=CARTESIAN_POINT('Ctrl Pts',(-3.71701050416802,-0.666666666666667,
0.496319364829374));
#48365=CARTESIAN_POINT('Ctrl Pts',(-3.71701050416802,-1.,0.496319364829374));
#48366=CARTESIAN_POINT('Ctrl Pts',(-4.18039834341342,-1.,0.405301974318349));
#48367=CARTESIAN_POINT('Ctrl Pts',(-4.18039834341342,1.,0.405301974318349));
#48368=CARTESIAN_POINT('Ctrl Pts',(-4.17892985789908,-1.,0.40586466267963));
#48369=CARTESIAN_POINT('Ctrl Pts',(-4.17892985789908,1.,0.40586466267963));
#48370=CARTESIAN_POINT('Ctrl Pts',(-4.17599251955585,-1.,0.406986596326602));
#48371=CARTESIAN_POINT('Ctrl Pts',(-4.17599251955585,1.,0.406986596326602));
#48372=CARTESIAN_POINT('Ctrl Pts',(-4.17158541009947,-1.,0.408659167570153));
#48373=CARTESIAN_POINT('Ctrl Pts',(-4.17158541009947,1.,0.408659167570153));
#48374=CARTESIAN_POINT('Ctrl Pts',(-4.16570705940731,-1.,0.410868596148613));
#48375=CARTESIAN_POINT('Ctrl Pts',(-4.16570705940731,1.,0.410868596148613));
#48376=CARTESIAN_POINT('Ctrl Pts',(-4.1583554501909,-1.,0.413595877953269));
#48377=CARTESIAN_POINT('Ctrl Pts',(-4.1583554501909,1.,0.413595877953269));
#48378=CARTESIAN_POINT('Ctrl Pts',(-4.15100018950989,-1.,0.416288556008986));
#48379=CARTESIAN_POINT('Ctrl Pts',(-4.15100018950989,1.,0.416288556008986));
#48380=CARTESIAN_POINT('Ctrl Pts',(-4.14364132317223,-1.,0.418946490667799));
#48381=CARTESIAN_POINT('Ctrl Pts',(-4.14364132317223,1.,0.418946490667799));
#48382=CARTESIAN_POINT('Ctrl Pts',(-4.13627893206433,-1.,0.421569503103971));
#48383=CARTESIAN_POINT('Ctrl Pts',(-4.13627893206433,1.,0.421569503103971));
#48384=CARTESIAN_POINT('Ctrl Pts',(-4.1289131463371,-1.,0.424157375323155));
#48385=CARTESIAN_POINT('Ctrl Pts',(-4.1289131463371,1.,0.424157375323155));
#48386=CARTESIAN_POINT('Ctrl Pts',(-4.1215441250121,-1.,0.426709855706243));
#48387=CARTESIAN_POINT('Ctrl Pts',(-4.1215441250121,1.,0.426709855706243));
#48388=CARTESIAN_POINT('Ctrl Pts',(-4.1141720278277,-1.,0.429226666075372));
#48389=CARTESIAN_POINT('Ctrl Pts',(-4.1141720278277,1.,0.429226666075372));
#48390=CARTESIAN_POINT('Ctrl Pts',(-4.10679698750219,-1.,0.431707508679772));
#48391=CARTESIAN_POINT('Ctrl Pts',(-4.10679698750219,1.,0.431707508679772));
#48392=CARTESIAN_POINT('Ctrl Pts',(-4.09941908688567,-1.,0.434152073200642));
#48393=CARTESIAN_POINT('Ctrl Pts',(-4.09941908688567,1.,0.434152073200642));
#48394=CARTESIAN_POINT('Ctrl Pts',(-4.09203832139439,-1.,0.436560044913814));
#48395=CARTESIAN_POINT('Ctrl Pts',(-4.09203832139439,1.,0.436560044913814));
#48396=CARTESIAN_POINT('Ctrl Pts',(-4.08465462294625,-1.,0.438931108931613));
#48397=CARTESIAN_POINT('Ctrl Pts',(-4.08465462294625,1.,0.438931108931613));
#48398=CARTESIAN_POINT('Ctrl Pts',(-4.07726792490256,-1.,0.441264951396587));
#48399=CARTESIAN_POINT('Ctrl Pts',(-4.07726792490256,1.,0.441264951396587));
#48400=CARTESIAN_POINT('Ctrl Pts',(-4.0698782192577,-1.,0.443561262395408));
#48401=CARTESIAN_POINT('Ctrl Pts',(-4.0698782192577,1.,0.443561262395408));
#48402=CARTESIAN_POINT('Ctrl Pts',(-4.06248560760596,-1.,0.445819737468478));
#48403=CARTESIAN_POINT('Ctrl Pts',(-4.06248560760596,1.,0.445819737468478));
#48404=CARTESIAN_POINT('Ctrl Pts',(-4.05509037796815,-1.,0.448040082683976));
#48405=CARTESIAN_POINT('Ctrl Pts',(-4.05509037796815,1.,0.448040082683976));
#48406=CARTESIAN_POINT('Ctrl Pts',(-4.0476929901797,-1.,0.450222009543774));
#48407=CARTESIAN_POINT('Ctrl Pts',(-4.0476929901797,1.,0.450222009543774));
#48408=CARTESIAN_POINT('Ctrl Pts',(-4.0402939222793,-1.,0.452365214748779));
#48409=CARTESIAN_POINT('Ctrl Pts',(-4.0402939222793,1.,0.452365214748779));
#48410=CARTESIAN_POINT('Ctrl Pts',(-4.03289354362745,-1.,0.454469363020495));
#48411=CARTESIAN_POINT('Ctrl Pts',(-4.03289354362745,1.,0.454469363020495));
#48412=CARTESIAN_POINT('Ctrl Pts',(-4.02549199038414,-1.,0.456534070784968));
#48413=CARTESIAN_POINT('Ctrl Pts',(-4.02549199038414,1.,0.456534070784968));
#48414=CARTESIAN_POINT('Ctrl Pts',(-4.01808900827647,-1.,0.458558885637001));
#48415=CARTESIAN_POINT('Ctrl Pts',(-4.01808900827647,1.,0.458558885637001));
#48416=CARTESIAN_POINT('Ctrl Pts',(-4.01068390573469,-1.,0.460543280768577));
#48417=CARTESIAN_POINT('Ctrl Pts',(-4.01068390573469,1.,0.460543280768577));
#48418=CARTESIAN_POINT('Ctrl Pts',(-4.00327590659129,-1.,0.462486702616252));
#48419=CARTESIAN_POINT('Ctrl Pts',(-4.00327590659129,1.,0.462486702616252));
#48420=CARTESIAN_POINT('Ctrl Pts',(-3.99586444320135,-1.,0.464388610938995));
#48421=CARTESIAN_POINT('Ctrl Pts',(-3.99586444320135,1.,0.464388610938995));
#48422=CARTESIAN_POINT('Ctrl Pts',(-3.98844946363258,-1.,0.466248520883034));
#48423=CARTESIAN_POINT('Ctrl Pts',(-3.98844946363258,1.,0.466248520883034));
#48424=CARTESIAN_POINT('Ctrl Pts',(-3.98103175589349,-1.,0.468066047920139));
#48425=CARTESIAN_POINT('Ctrl Pts',(-3.98103175589349,1.,0.468066047920139));
#48426=CARTESIAN_POINT('Ctrl Pts',(-3.97361320212413,-1.,0.469840942829878));
#48427=CARTESIAN_POINT('Ctrl Pts',(-3.97361320212413,1.,0.469840942829878));
#48428=CARTESIAN_POINT('Ctrl Pts',(-3.96619600864626,-1.,0.471572978413493));
#48429=CARTESIAN_POINT('Ctrl Pts',(-3.96619600864626,1.,0.471572978413493));
#48430=CARTESIAN_POINT('Ctrl Pts',(-3.95878201038332,-1.,0.473261847236296));
#48431=CARTESIAN_POINT('Ctrl Pts',(-3.95878201038332,1.,0.473261847236296));
#48432=CARTESIAN_POINT('Ctrl Pts',(-3.95137192932898,-1.,0.47490705302179));
#48433=CARTESIAN_POINT('Ctrl Pts',(-3.95137192932898,1.,0.47490705302179));
#48434=CARTESIAN_POINT('Ctrl Pts',(-3.94396469119385,-1.,0.476507810658534));
#48435=CARTESIAN_POINT('Ctrl Pts',(-3.94396469119385,1.,0.476507810658534));
#48436=CARTESIAN_POINT('Ctrl Pts',(-3.93655660689819,-1.,0.478062927140957));
#48437=CARTESIAN_POINT('Ctrl Pts',(-3.93655660689819,1.,0.478062927140957));
#48438=CARTESIAN_POINT('Ctrl Pts',(-3.92914297392067,-1.,0.479571028525566));
#48439=CARTESIAN_POINT('Ctrl Pts',(-3.92914297392067,1.,0.479571028525566));
#48440=CARTESIAN_POINT('Ctrl Pts',(-3.92171976072334,-1.,0.481030798910735));
#48441=CARTESIAN_POINT('Ctrl Pts',(-3.92171976072334,1.,0.481030798910735));
#48442=CARTESIAN_POINT('Ctrl Pts',(-3.91428536373749,-1.,0.482441230340708));
#48443=CARTESIAN_POINT('Ctrl Pts',(-3.91428536373749,1.,0.482441230340708));
#48444=CARTESIAN_POINT('Ctrl Pts',(-3.90684210358063,-1.,0.48380183508916));
#48445=CARTESIAN_POINT('Ctrl Pts',(-3.90684210358063,1.,0.48380183508916));
#48446=CARTESIAN_POINT('Ctrl Pts',(-3.89939844658529,-1.,0.485112963522246));
#48447=CARTESIAN_POINT('Ctrl Pts',(-3.89939844658529,1.,0.485112963522246));
#48448=CARTESIAN_POINT('Ctrl Pts',(-3.89196582437574,-1.,0.486375337854133));
#48449=CARTESIAN_POINT('Ctrl Pts',(-3.89196582437574,1.,0.486375337854133));
#48450=CARTESIAN_POINT('Ctrl Pts',(-3.88455453328156,-1.,0.487589452275179));
#48451=CARTESIAN_POINT('Ctrl Pts',(-3.88455453328156,1.,0.487589452275179));
#48452=CARTESIAN_POINT('Ctrl Pts',(-3.87716963231115,-1.,0.488754973798281));
#48453=CARTESIAN_POINT('Ctrl Pts',(-3.87716963231115,1.,0.488754973798281));
#48454=CARTESIAN_POINT('Ctrl Pts',(-3.86980755613694,-1.,0.489870245704899));
#48455=CARTESIAN_POINT('Ctrl Pts',(-3.86980755613694,1.,0.489870245704899));
#48456=CARTESIAN_POINT('Ctrl Pts',(-3.86245057319215,-1.,0.490931482170849));
#48457=CARTESIAN_POINT('Ctrl Pts',(-3.86245057319215,1.,0.490931482170849));
#48458=CARTESIAN_POINT('Ctrl Pts',(-3.85507287020223,-1.,0.49193363108376));
#48459=CARTESIAN_POINT('Ctrl Pts',(-3.85507287020223,1.,0.49193363108376));
#48460=CARTESIAN_POINT('Ctrl Pts',(-3.84765051147965,-1.,0.492871792414095));
#48461=CARTESIAN_POINT('Ctrl Pts',(-3.84765051147965,1.,0.492871792414095));
#48462=CARTESIAN_POINT('Ctrl Pts',(-3.84017095578438,-1.,0.493742574629117));
#48463=CARTESIAN_POINT('Ctrl Pts',(-3.84017095578438,1.,0.493742574629117));
#48464=CARTESIAN_POINT('Ctrl Pts',(-3.8326409268245,-1.,0.494545212256425));
#48465=CARTESIAN_POINT('Ctrl Pts',(-3.8326409268245,1.,0.494545212256425));
#48466=CARTESIAN_POINT('Ctrl Pts',(-3.82509963594156,-1.,0.495283458893903));
#48467=CARTESIAN_POINT('Ctrl Pts',(-3.82509963594156,1.,0.495283458893903));
#48468=CARTESIAN_POINT('Ctrl Pts',(-3.81760756144099,-1.,0.495963937875572));
#48469=CARTESIAN_POINT('Ctrl Pts',(-3.81760756144099,1.,0.495963937875572));
#48470=CARTESIAN_POINT('Ctrl Pts',(-3.81022254090909,-1.,0.496592643443789));
#48471=CARTESIAN_POINT('Ctrl Pts',(-3.81022254090909,1.,0.496592643443789));
#48472=CARTESIAN_POINT('Ctrl Pts',(-3.80297788298545,-1.,0.49717175620109));
#48473=CARTESIAN_POINT('Ctrl Pts',(-3.80297788298545,1.,0.49717175620109));
#48474=CARTESIAN_POINT('Ctrl Pts',(-3.79586380669959,-1.,0.49769689210058));
#48475=CARTESIAN_POINT('Ctrl Pts',(-3.79586380669959,1.,0.49769689210058));
#48476=CARTESIAN_POINT('Ctrl Pts',(-3.78879701661152,-1.,0.498152751800819));
#48477=CARTESIAN_POINT('Ctrl Pts',(-3.78879701661152,1.,0.498152751800819));
#48478=CARTESIAN_POINT('Ctrl Pts',(-3.78163975337189,-1.,0.498515471679378));
#48479=CARTESIAN_POINT('Ctrl Pts',(-3.78163975337189,1.,0.498515471679378));
#48480=CARTESIAN_POINT('Ctrl Pts',(-3.77425499225089,-1.,0.498759900365687));
#48481=CARTESIAN_POINT('Ctrl Pts',(-3.77425499225089,1.,0.498759900365687));
#48482=CARTESIAN_POINT('Ctrl Pts',(-3.76655401191144,-1.,0.498865792335185));
#48483=CARTESIAN_POINT('Ctrl Pts',(-3.76655401191144,1.,0.498865792335185));
#48484=CARTESIAN_POINT('Ctrl Pts',(-3.75854082221127,-1.,0.498823681615513));
#48485=CARTESIAN_POINT('Ctrl Pts',(-3.75854082221127,1.,0.498823681615513));
#48486=CARTESIAN_POINT('Ctrl Pts',(-3.75037362168103,-1.,0.498642802042929));
#48487=CARTESIAN_POINT('Ctrl Pts',(-3.75037362168103,1.,0.498642802042929));
#48488=CARTESIAN_POINT('Ctrl Pts',(-3.74235701735109,-1.,0.498350586058176));
#48489=CARTESIAN_POINT('Ctrl Pts',(-3.74235701735109,1.,0.498350586058176));
#48490=CARTESIAN_POINT('Ctrl Pts',(-3.73486914372834,-1.,0.497984209510495));
#48491=CARTESIAN_POINT('Ctrl Pts',(-3.73486914372834,1.,0.497984209510495));
#48492=CARTESIAN_POINT('Ctrl Pts',(-3.72830430904794,-1.,0.497584067153279));
#48493=CARTESIAN_POINT('Ctrl Pts',(-3.72830430904794,1.,0.497584067153279));
#48494=CARTESIAN_POINT('Ctrl Pts',(-3.72301489774241,-1.,0.497187079575794));
#48495=CARTESIAN_POINT('Ctrl Pts',(-3.72301489774241,1.,0.497187079575794));
#48496=CARTESIAN_POINT('Ctrl Pts',(-3.71923995965807,-1.,0.496818574419988));
#48497=CARTESIAN_POINT('Ctrl Pts',(-3.71923995965807,1.,0.496818574419988));
#48498=CARTESIAN_POINT('Ctrl Pts',(-3.71752134136931,-1.,0.496556137603856));
#48499=CARTESIAN_POINT('Ctrl Pts',(-3.71752134136931,1.,0.496556137603856));
#48500=CARTESIAN_POINT('Ctrl Pts',(-3.71698153685229,-1.,0.496379397992181));
#48501=CARTESIAN_POINT('Ctrl Pts',(-3.71698153685229,1.,0.496379397992181));
#48502=CARTESIAN_POINT('Ctrl Pts',(-3.71695438995598,-1.,0.496270484166233));
#48503=CARTESIAN_POINT('Ctrl Pts',(-3.71695438995598,1.,0.496270484166233));
#48504=CARTESIAN_POINT('Ctrl Pts',(-3.71702400346349,-1.,0.496218256089211));
#48505=CARTESIAN_POINT('Ctrl Pts',(-3.71702400346349,1.,0.496218256089211));
#48506=CARTESIAN_POINT('',(-4.18039834341342,1.,0.405301974318349));
#48507=CARTESIAN_POINT('Ctrl Pts',(-4.18039834341342,1.,0.405301974318349));
#48508=CARTESIAN_POINT('Ctrl Pts',(-4.17892985789908,1.,0.40586466267963));
#48509=CARTESIAN_POINT('Ctrl Pts',(-4.17599251955585,1.,0.406986596326602));
#48510=CARTESIAN_POINT('Ctrl Pts',(-4.17158541009947,1.,0.408659167570153));
#48511=CARTESIAN_POINT('Ctrl Pts',(-4.16570705940731,1.,0.410868596148613));
#48512=CARTESIAN_POINT('Ctrl Pts',(-4.1583554501909,1.,0.413595877953269));
#48513=CARTESIAN_POINT('Ctrl Pts',(-4.15100018950989,1.,0.416288556008986));
#48514=CARTESIAN_POINT('Ctrl Pts',(-4.14364132317223,1.,0.418946490667799));
#48515=CARTESIAN_POINT('Ctrl Pts',(-4.13627893206433,1.,0.421569503103971));
#48516=CARTESIAN_POINT('Ctrl Pts',(-4.1289131463371,1.,0.424157375323155));
#48517=CARTESIAN_POINT('Ctrl Pts',(-4.1215441250121,1.,0.426709855706243));
#48518=CARTESIAN_POINT('Ctrl Pts',(-4.1141720278277,1.,0.429226666075372));
#48519=CARTESIAN_POINT('Ctrl Pts',(-4.10679698750219,1.,0.431707508679772));
#48520=CARTESIAN_POINT('Ctrl Pts',(-4.09941908688567,1.,0.434152073200642));
#48521=CARTESIAN_POINT('Ctrl Pts',(-4.09203832139439,1.,0.436560044913814));
#48522=CARTESIAN_POINT('Ctrl Pts',(-4.08465462294625,1.,0.438931108931613));
#48523=CARTESIAN_POINT('Ctrl Pts',(-4.07726792490256,1.,0.441264951396587));
#48524=CARTESIAN_POINT('Ctrl Pts',(-4.0698782192577,1.,0.443561262395408));
#48525=CARTESIAN_POINT('Ctrl Pts',(-4.06248560760596,1.,0.445819737468478));
#48526=CARTESIAN_POINT('Ctrl Pts',(-4.05509037796815,1.,0.448040082683976));
#48527=CARTESIAN_POINT('Ctrl Pts',(-4.0476929901797,1.,0.450222009543774));
#48528=CARTESIAN_POINT('Ctrl Pts',(-4.0402939222793,1.,0.452365214748779));
#48529=CARTESIAN_POINT('Ctrl Pts',(-4.03289354362745,1.,0.454469363020495));
#48530=CARTESIAN_POINT('Ctrl Pts',(-4.02549199038414,1.,0.456534070784968));
#48531=CARTESIAN_POINT('Ctrl Pts',(-4.01808900827647,1.,0.458558885637001));
#48532=CARTESIAN_POINT('Ctrl Pts',(-4.01068390573469,1.,0.460543280768577));
#48533=CARTESIAN_POINT('Ctrl Pts',(-4.00327590659129,1.,0.462486702616252));
#48534=CARTESIAN_POINT('Ctrl Pts',(-3.99586444320135,1.,0.464388610938995));
#48535=CARTESIAN_POINT('Ctrl Pts',(-3.98844946363258,1.,0.466248520883034));
#48536=CARTESIAN_POINT('Ctrl Pts',(-3.98103175589349,1.,0.468066047920139));
#48537=CARTESIAN_POINT('Ctrl Pts',(-3.97361320212413,1.,0.469840942829878));
#48538=CARTESIAN_POINT('Ctrl Pts',(-3.96619600864626,1.,0.471572978413493));
#48539=CARTESIAN_POINT('Ctrl Pts',(-3.95878201038332,1.,0.473261847236296));
#48540=CARTESIAN_POINT('Ctrl Pts',(-3.95137192932898,1.,0.47490705302179));
#48541=CARTESIAN_POINT('Ctrl Pts',(-3.94396469119385,1.,0.476507810658534));
#48542=CARTESIAN_POINT('Ctrl Pts',(-3.93655660689819,1.,0.478062927140957));
#48543=CARTESIAN_POINT('Ctrl Pts',(-3.92914297392067,1.,0.479571028525566));
#48544=CARTESIAN_POINT('Ctrl Pts',(-3.92171976072334,1.,0.481030798910735));
#48545=CARTESIAN_POINT('Ctrl Pts',(-3.91428536373749,1.,0.482441230340708));
#48546=CARTESIAN_POINT('Ctrl Pts',(-3.90684210358063,1.,0.48380183508916));
#48547=CARTESIAN_POINT('Ctrl Pts',(-3.89939844658529,1.,0.485112963522246));
#48548=CARTESIAN_POINT('Ctrl Pts',(-3.89196582437574,1.,0.486375337854133));
#48549=CARTESIAN_POINT('Ctrl Pts',(-3.88455453328156,1.,0.487589452275179));
#48550=CARTESIAN_POINT('Ctrl Pts',(-3.87716963231115,1.,0.488754973798281));
#48551=CARTESIAN_POINT('Ctrl Pts',(-3.86980755613694,1.,0.489870245704899));
#48552=CARTESIAN_POINT('Ctrl Pts',(-3.86245057319215,1.,0.490931482170849));
#48553=CARTESIAN_POINT('Ctrl Pts',(-3.85507287020223,1.,0.49193363108376));
#48554=CARTESIAN_POINT('Ctrl Pts',(-3.84765051147965,1.,0.492871792414095));
#48555=CARTESIAN_POINT('Ctrl Pts',(-3.84017095578438,1.,0.493742574629117));
#48556=CARTESIAN_POINT('Ctrl Pts',(-3.8326409268245,1.,0.494545212256425));
#48557=CARTESIAN_POINT('Ctrl Pts',(-3.82509963594156,1.,0.495283458893903));
#48558=CARTESIAN_POINT('Ctrl Pts',(-3.81760756144099,1.,0.495963937875572));
#48559=CARTESIAN_POINT('Ctrl Pts',(-3.81022254090909,1.,0.496592643443789));
#48560=CARTESIAN_POINT('Ctrl Pts',(-3.80297788298545,1.,0.49717175620109));
#48561=CARTESIAN_POINT('Ctrl Pts',(-3.79586380669959,1.,0.49769689210058));
#48562=CARTESIAN_POINT('Ctrl Pts',(-3.78879701661152,1.,0.498152751800819));
#48563=CARTESIAN_POINT('Ctrl Pts',(-3.78163975337189,1.,0.498515471679378));
#48564=CARTESIAN_POINT('Ctrl Pts',(-3.77425499225089,1.,0.498759900365687));
#48565=CARTESIAN_POINT('Ctrl Pts',(-3.76655401191144,1.,0.498865792335185));
#48566=CARTESIAN_POINT('Ctrl Pts',(-3.75854082221127,1.,0.498823681615513));
#48567=CARTESIAN_POINT('Ctrl Pts',(-3.75037362168103,1.,0.498642802042929));
#48568=CARTESIAN_POINT('Ctrl Pts',(-3.74235701735109,1.,0.498350586058176));
#48569=CARTESIAN_POINT('Ctrl Pts',(-3.73486914372834,1.,0.497984209510495));
#48570=CARTESIAN_POINT('Ctrl Pts',(-3.72830430904794,1.,0.497584067153279));
#48571=CARTESIAN_POINT('Ctrl Pts',(-3.72301489774241,1.,0.497187079575794));
#48572=CARTESIAN_POINT('Ctrl Pts',(-3.7195232082259,1.,0.496846224822535));
#48573=CARTESIAN_POINT('Ctrl Pts',(-3.71785517607694,1.,0.496605651526313));
#48574=CARTESIAN_POINT('Ctrl Pts',(-3.71721917030465,1.,0.496446644158827));
#48575=CARTESIAN_POINT('Ctrl Pts',(-3.71704500630521,1.,0.496354087925645));
#48576=CARTESIAN_POINT('Ctrl Pts',(-3.71701050416802,1.,0.496319364829374));
#48577=CARTESIAN_POINT('',(-4.18039834341342,0.,0.405301974318349));
#48578=CARTESIAN_POINT('Ctrl Pts',(-3.74888690736767,-1.,0.091361675593742));
#48579=CARTESIAN_POINT('Ctrl Pts',(-3.74888690736767,1.,0.091361675593742));
#48580=CARTESIAN_POINT('Ctrl Pts',(-3.74882632119067,-1.,0.0912992005792584));
#48581=CARTESIAN_POINT('Ctrl Pts',(-3.74882632119067,1.,0.0912992005792584));
#48582=CARTESIAN_POINT('Ctrl Pts',(-3.74887017174206,-1.,0.0911958743735234));
#48583=CARTESIAN_POINT('Ctrl Pts',(-3.74887017174206,1.,0.0911958743735234));
#48584=CARTESIAN_POINT('Ctrl Pts',(-3.74943097853811,-1.,0.0911057547506599));
#48585=CARTESIAN_POINT('Ctrl Pts',(-3.74943097853811,1.,0.0911057547506599));
#48586=CARTESIAN_POINT('Ctrl Pts',(-3.75116949194623,-1.,0.0911154000998141));
#48587=CARTESIAN_POINT('Ctrl Pts',(-3.75116949194623,1.,0.0911154000998141));
#48588=CARTESIAN_POINT('Ctrl Pts',(-3.75495560118212,-1.,0.0913419622736397));
#48589=CARTESIAN_POINT('Ctrl Pts',(-3.75495560118212,1.,0.0913419622736397));
#48590=CARTESIAN_POINT('Ctrl Pts',(-3.76024199359303,-1.,0.0917773084998334));
#48591=CARTESIAN_POINT('Ctrl Pts',(-3.76024199359303,1.,0.0917773084998334));
#48592=CARTESIAN_POINT('Ctrl Pts',(-3.76678860031841,-1.,0.092409058960269));
#48593=CARTESIAN_POINT('Ctrl Pts',(-3.76678860031841,1.,0.092409058960269));
#48594=CARTESIAN_POINT('Ctrl Pts',(-3.77424159971059,-1.,0.0932185546203178));
#48595=CARTESIAN_POINT('Ctrl Pts',(-3.77424159971059,1.,0.0932185546203178));
#48596=CARTESIAN_POINT('Ctrl Pts',(-3.782205218991,-1.,0.0941840095090813));
#48597=CARTESIAN_POINT('Ctrl Pts',(-3.782205218991,1.,0.0941840095090813));
#48598=CARTESIAN_POINT('Ctrl Pts',(-3.79030016353111,-1.,0.09528298851008));
#48599=CARTESIAN_POINT('Ctrl Pts',(-3.79030016353111,1.,0.09528298851008));
#48600=CARTESIAN_POINT('Ctrl Pts',(-3.79822128513845,-1.,0.0964949352873131));
#48601=CARTESIAN_POINT('Ctrl Pts',(-3.79822128513845,1.,0.0964949352873131));
#48602=CARTESIAN_POINT('Ctrl Pts',(-3.80581088847809,-1.,0.0978042222906642));
#48603=CARTESIAN_POINT('Ctrl Pts',(-3.80581088847809,1.,0.0978042222906642));
#48604=CARTESIAN_POINT('Ctrl Pts',(-3.81306649386461,-1.,0.0992008728096513));
#48605=CARTESIAN_POINT('Ctrl Pts',(-3.81306649386461,1.,0.0992008728096513));
#48606=CARTESIAN_POINT('Ctrl Pts',(-3.82007889742625,-1.,0.100678769650632));
#48607=CARTESIAN_POINT('Ctrl Pts',(-3.82007889742625,1.,0.100678769650632));
#48608=CARTESIAN_POINT('Ctrl Pts',(-3.82698737143255,-1.,0.102234506488456));
#48609=CARTESIAN_POINT('Ctrl Pts',(-3.82698737143255,1.,0.102234506488456));
#48610=CARTESIAN_POINT('Ctrl Pts',(-3.83393171228002,-1.,0.103866063811622));
#48611=CARTESIAN_POINT('Ctrl Pts',(-3.83393171228002,1.,0.103866063811622));
#48612=CARTESIAN_POINT('Ctrl Pts',(-3.84099658324803,-1.,0.105571360916569));
#48613=CARTESIAN_POINT('Ctrl Pts',(-3.84099658324803,1.,0.105571360916569));
#48614=CARTESIAN_POINT('Ctrl Pts',(-3.84819233070317,-1.,0.107347597812183));
#48615=CARTESIAN_POINT('Ctrl Pts',(-3.84819233070317,1.,0.107347597812183));
#48616=CARTESIAN_POINT('Ctrl Pts',(-3.855485714969,-1.,0.109191717634943));
#48617=CARTESIAN_POINT('Ctrl Pts',(-3.855485714969,1.,0.109191717634943));
#48618=CARTESIAN_POINT('Ctrl Pts',(-3.86281867282965,-1.,0.11110059303626));
#48619=CARTESIAN_POINT('Ctrl Pts',(-3.86281867282965,1.,0.11110059303626));
#48620=CARTESIAN_POINT('Ctrl Pts',(-3.87013043445014,-1.,0.113071304914561));
#48621=CARTESIAN_POINT('Ctrl Pts',(-3.87013043445014,1.,0.113071304914561));
#48622=CARTESIAN_POINT('Ctrl Pts',(-3.87738168405343,-1.,0.11510142664947));
#48623=CARTESIAN_POINT('Ctrl Pts',(-3.87738168405343,1.,0.11510142664947));
#48624=CARTESIAN_POINT('Ctrl Pts',(-3.88456590045767,-1.,0.117189150373144));
#48625=CARTESIAN_POINT('Ctrl Pts',(-3.88456590045767,1.,0.117189150373144));
#48626=CARTESIAN_POINT('Ctrl Pts',(-3.89169600105201,-1.,0.119333088190417));
#48627=CARTESIAN_POINT('Ctrl Pts',(-3.89169600105201,1.,0.119333088190417));
#48628=CARTESIAN_POINT('Ctrl Pts',(-3.89879639336952,-1.,0.121532144765723));
#48629=CARTESIAN_POINT('Ctrl Pts',(-3.89879639336952,1.,0.121532144765723));
#48630=CARTESIAN_POINT('Ctrl Pts',(-3.90589336320508,-1.,0.123785368272377));
#48631=CARTESIAN_POINT('Ctrl Pts',(-3.90589336320508,1.,0.123785368272377));
#48632=CARTESIAN_POINT('Ctrl Pts',(-3.91300501605392,-1.,0.126091793324136));
#48633=CARTESIAN_POINT('Ctrl Pts',(-3.91300501605392,1.,0.126091793324136));
#48634=CARTESIAN_POINT('Ctrl Pts',(-3.92013513251642,-1.,0.128450341339528));
#48635=CARTESIAN_POINT('Ctrl Pts',(-3.92013513251642,1.,0.128450341339528));
#48636=CARTESIAN_POINT('Ctrl Pts',(-3.9272787679596,-1.,0.130859892027798));
#48637=CARTESIAN_POINT('Ctrl Pts',(-3.9272787679596,1.,0.130859892027798));
#48638=CARTESIAN_POINT('Ctrl Pts',(-3.93442567551035,-1.,0.133319322794189));
#48639=CARTESIAN_POINT('Ctrl Pts',(-3.93442567551035,1.,0.133319322794189));
#48640=CARTESIAN_POINT('Ctrl Pts',(-3.94156445130744,-1.,0.135827558661188));
#48641=CARTESIAN_POINT('Ctrl Pts',(-3.94156445130744,1.,0.135827558661188));
#48642=CARTESIAN_POINT('Ctrl Pts',(-3.94868667844355,-1.,0.138383621255159));
#48643=CARTESIAN_POINT('Ctrl Pts',(-3.94868667844355,1.,0.138383621255159));
#48644=CARTESIAN_POINT('Ctrl Pts',(-3.95579014116899,-1.,0.140986665829937));
#48645=CARTESIAN_POINT('Ctrl Pts',(-3.95579014116899,1.,0.140986665829937));
#48646=CARTESIAN_POINT('Ctrl Pts',(-3.96287658098896,-1.,0.143635947692791));
#48647=CARTESIAN_POINT('Ctrl Pts',(-3.96287658098896,1.,0.143635947692791));
#48648=CARTESIAN_POINT('Ctrl Pts',(-3.96995018565891,-1.,0.146330797814513));
#48649=CARTESIAN_POINT('Ctrl Pts',(-3.96995018565891,1.,0.146330797814513));
#48650=CARTESIAN_POINT('Ctrl Pts',(-3.97701581473643,-1.,0.149070594803543));
#48651=CARTESIAN_POINT('Ctrl Pts',(-3.97701581473643,1.,0.149070594803543));
#48652=CARTESIAN_POINT('Ctrl Pts',(-3.9840772985098,-1.,0.151854737441405));
#48653=CARTESIAN_POINT('Ctrl Pts',(-3.9840772985098,1.,0.151854737441405));
#48654=CARTESIAN_POINT('Ctrl Pts',(-3.99113582086059,-1.,0.154682618338563));
#48655=CARTESIAN_POINT('Ctrl Pts',(-3.99113582086059,1.,0.154682618338563));
#48656=CARTESIAN_POINT('Ctrl Pts',(-3.99819074631874,-1.,0.157553634383809));
#48657=CARTESIAN_POINT('Ctrl Pts',(-3.99819074631874,1.,0.157553634383809));
#48658=CARTESIAN_POINT('Ctrl Pts',(-4.00524031064509,-1.,0.160467194882219));
#48659=CARTESIAN_POINT('Ctrl Pts',(-4.00524031064509,1.,0.160467194882219));
#48660=CARTESIAN_POINT('Ctrl Pts',(-4.01228237022301,-1.,0.163422730287458));
#48661=CARTESIAN_POINT('Ctrl Pts',(-4.01228237022301,1.,0.163422730287458));
#48662=CARTESIAN_POINT('Ctrl Pts',(-4.01931510507143,-1.,0.166419700015847));
#48663=CARTESIAN_POINT('Ctrl Pts',(-4.01931510507143,1.,0.166419700015847));
#48664=CARTESIAN_POINT('Ctrl Pts',(-4.0263377970371,-1.,0.169457601001653));
#48665=CARTESIAN_POINT('Ctrl Pts',(-4.0263377970371,1.,0.169457601001653));
#48666=CARTESIAN_POINT('Ctrl Pts',(-4.03335057326093,-1.,0.172535962484466));
#48667=CARTESIAN_POINT('Ctrl Pts',(-4.03335057326093,1.,0.172535962484466));
#48668=CARTESIAN_POINT('Ctrl Pts',(-4.04035407891161,-1.,0.175654339673757));
#48669=CARTESIAN_POINT('Ctrl Pts',(-4.04035407891161,1.,0.175654339673757));
#48670=CARTESIAN_POINT('Ctrl Pts',(-4.04734916719722,-1.,0.178812307240715));
#48671=CARTESIAN_POINT('Ctrl Pts',(-4.04734916719722,1.,0.178812307240715));
#48672=CARTESIAN_POINT('Ctrl Pts',(-4.05433660358402,-1.,0.18200945304855));
#48673=CARTESIAN_POINT('Ctrl Pts',(-4.05433660358402,1.,0.18200945304855));
#48674=CARTESIAN_POINT('Ctrl Pts',(-4.06131670998589,-1.,0.185245370038948));
#48675=CARTESIAN_POINT('Ctrl Pts',(-4.06131670998589,1.,0.185245370038948));
#48676=CARTESIAN_POINT('Ctrl Pts',(-4.06828941192308,-1.,0.188519658060255));
#48677=CARTESIAN_POINT('Ctrl Pts',(-4.06828941192308,1.,0.188519658060255));
#48678=CARTESIAN_POINT('Ctrl Pts',(-4.07525439703137,-1.,0.191831928181081));
#48679=CARTESIAN_POINT('Ctrl Pts',(-4.07525439703137,1.,0.191831928181081));
#48680=CARTESIAN_POINT('Ctrl Pts',(-4.08221124060385,-1.,0.195181806054714));
#48681=CARTESIAN_POINT('Ctrl Pts',(-4.08221124060385,1.,0.195181806054714));
#48682=CARTESIAN_POINT('Ctrl Pts',(-4.08915953359753,-1.,0.19856893480081));
#48683=CARTESIAN_POINT('Ctrl Pts',(-4.08915953359753,1.,0.19856893480081));
#48684=CARTESIAN_POINT('Ctrl Pts',(-4.09609903751912,-1.,0.201992979049984));
#48685=CARTESIAN_POINT('Ctrl Pts',(-4.09609903751912,1.,0.201992979049984));
#48686=CARTESIAN_POINT('Ctrl Pts',(-4.10302969965374,-1.,0.205453622198233));
#48687=CARTESIAN_POINT('Ctrl Pts',(-4.10302969965374,1.,0.205453622198233));
#48688=CARTESIAN_POINT('Ctrl Pts',(-4.10995157639026,-1.,0.208950559400172));
#48689=CARTESIAN_POINT('Ctrl Pts',(-4.10995157639026,1.,0.208950559400172));
#48690=CARTESIAN_POINT('Ctrl Pts',(-4.11686478264545,-1.,0.212483491087068));
#48691=CARTESIAN_POINT('Ctrl Pts',(-4.11686478264545,1.,0.212483491087068));
#48692=CARTESIAN_POINT('Ctrl Pts',(-4.12376943492249,-1.,0.216052116898425));
#48693=CARTESIAN_POINT('Ctrl Pts',(-4.12376943492249,1.,0.216052116898425));
#48694=CARTESIAN_POINT('Ctrl Pts',(-4.13066558698156,-1.,0.219656126701851));
#48695=CARTESIAN_POINT('Ctrl Pts',(-4.13066558698156,1.,0.219656126701851));
#48696=CARTESIAN_POINT('Ctrl Pts',(-4.13755320553563,-1.,0.223295201038383));
#48697=CARTESIAN_POINT('Ctrl Pts',(-4.13755320553563,1.,0.223295201038383));
#48698=CARTESIAN_POINT('Ctrl Pts',(-4.14443220607733,-1.,0.226969025061243));
#48699=CARTESIAN_POINT('Ctrl Pts',(-4.14443220607733,1.,0.226969025061243));
#48700=CARTESIAN_POINT('Ctrl Pts',(-4.15130247435029,-1.,0.230677299028738));
#48701=CARTESIAN_POINT('Ctrl Pts',(-4.15130247435029,1.,0.230677299028738));
#48702=CARTESIAN_POINT('Ctrl Pts',(-4.1581638926525,-1.,0.234419749543143));
#48703=CARTESIAN_POINT('Ctrl Pts',(-4.1581638926525,1.,0.234419749543143));
#48704=CARTESIAN_POINT('Ctrl Pts',(-4.1650163665385,-1.,0.238196140933976));
#48705=CARTESIAN_POINT('Ctrl Pts',(-4.1650163665385,1.,0.238196140933976));
#48706=CARTESIAN_POINT('Ctrl Pts',(-4.17185984409533,-1.,0.242006283923911));
#48707=CARTESIAN_POINT('Ctrl Pts',(-4.17185984409533,1.,0.242006283923911));
#48708=CARTESIAN_POINT('Ctrl Pts',(-4.17869430192868,-1.,0.245850033418583));
#48709=CARTESIAN_POINT('Ctrl Pts',(-4.17869430192868,1.,0.245850033418583));
#48710=CARTESIAN_POINT('Ctrl Pts',(-4.18415464959491,-1.,0.248951836910963));
#48711=CARTESIAN_POINT('Ctrl Pts',(-4.18415464959491,1.,0.248951836910963));
#48712=CARTESIAN_POINT('Ctrl Pts',(-4.18824585244066,-1.,0.251293239837692));
#48713=CARTESIAN_POINT('Ctrl Pts',(-4.18824585244066,1.,0.251293239837692));
#48714=CARTESIAN_POINT('Ctrl Pts',(-4.19097151819241,-1.,0.252860861572565));
#48715=CARTESIAN_POINT('Ctrl Pts',(-4.19097151819241,1.,0.252860861572565));
#48716=CARTESIAN_POINT('Ctrl Pts',(-4.1923339003649,-1.,0.253646344052521));
#48717=CARTESIAN_POINT('Ctrl Pts',(-4.1923339003649,1.,0.253646344052521));
#48718=CARTESIAN_POINT('',(-3.74888939116255,1.,0.0912596999166825));
#48719=CARTESIAN_POINT('Ctrl Pts',(-3.74888939116255,-1.,0.091259699916682));
#48720=CARTESIAN_POINT('Ctrl Pts',(-3.74888939116255,-0.666666666666667,
0.091259699916682));
#48721=CARTESIAN_POINT('Ctrl Pts',(-3.74888939116255,-0.333333333333333,
0.091259699916682));
#48722=CARTESIAN_POINT('Ctrl Pts',(-3.74888939116255,0.333333333333333,
0.091259699916682));
#48723=CARTESIAN_POINT('Ctrl Pts',(-3.74888939116255,0.666666666666667,
0.0912596999166817));
#48724=CARTESIAN_POINT('Ctrl Pts',(-3.74888939116255,1.,0.0912596999166817));
#48725=CARTESIAN_POINT('',(-4.1923339003649,1.,0.253646344052521));
#48726=CARTESIAN_POINT('',(-4.1923339003649,0.,0.253646344052521));
#48727=CARTESIAN_POINT('Ctrl Pts',(-3.74888939116255,1.,0.0912596999166823));
#48728=CARTESIAN_POINT('Ctrl Pts',(-3.74892890040974,1.,0.0912308016421982));
#48729=CARTESIAN_POINT('Ctrl Pts',(-3.74911539914542,1.,0.0911666301812817));
#48730=CARTESIAN_POINT('Ctrl Pts',(-3.74976844886346,1.,0.0911090736805509));
#48731=CARTESIAN_POINT('Ctrl Pts',(-3.75145357872422,1.,0.0911323999574425));
#48732=CARTESIAN_POINT('Ctrl Pts',(-3.75495560118212,1.,0.0913419622736397));
#48733=CARTESIAN_POINT('Ctrl Pts',(-3.76024199359303,1.,0.0917773084998334));
#48734=CARTESIAN_POINT('Ctrl Pts',(-3.76678860031841,1.,0.092409058960269));
#48735=CARTESIAN_POINT('Ctrl Pts',(-3.77424159971059,1.,0.0932185546203178));
#48736=CARTESIAN_POINT('Ctrl Pts',(-3.782205218991,1.,0.0941840095090813));
#48737=CARTESIAN_POINT('Ctrl Pts',(-3.79030016353111,1.,0.09528298851008));
#48738=CARTESIAN_POINT('Ctrl Pts',(-3.79822128513845,1.,0.0964949352873131));
#48739=CARTESIAN_POINT('Ctrl Pts',(-3.80581088847809,1.,0.0978042222906642));
#48740=CARTESIAN_POINT('Ctrl Pts',(-3.81306649386461,1.,0.0992008728096513));
#48741=CARTESIAN_POINT('Ctrl Pts',(-3.82007889742625,1.,0.100678769650632));
#48742=CARTESIAN_POINT('Ctrl Pts',(-3.82698737143255,1.,0.102234506488456));
#48743=CARTESIAN_POINT('Ctrl Pts',(-3.83393171228002,1.,0.103866063811622));
#48744=CARTESIAN_POINT('Ctrl Pts',(-3.84099658324803,1.,0.105571360916569));
#48745=CARTESIAN_POINT('Ctrl Pts',(-3.84819233070317,1.,0.107347597812183));
#48746=CARTESIAN_POINT('Ctrl Pts',(-3.855485714969,1.,0.109191717634943));
#48747=CARTESIAN_POINT('Ctrl Pts',(-3.86281867282965,1.,0.11110059303626));
#48748=CARTESIAN_POINT('Ctrl Pts',(-3.87013043445014,1.,0.113071304914561));
#48749=CARTESIAN_POINT('Ctrl Pts',(-3.87738168405343,1.,0.11510142664947));
#48750=CARTESIAN_POINT('Ctrl Pts',(-3.88456590045767,1.,0.117189150373144));
#48751=CARTESIAN_POINT('Ctrl Pts',(-3.89169600105201,1.,0.119333088190417));
#48752=CARTESIAN_POINT('Ctrl Pts',(-3.89879639336952,1.,0.121532144765723));
#48753=CARTESIAN_POINT('Ctrl Pts',(-3.90589336320508,1.,0.123785368272377));
#48754=CARTESIAN_POINT('Ctrl Pts',(-3.91300501605392,1.,0.126091793324136));
#48755=CARTESIAN_POINT('Ctrl Pts',(-3.92013513251642,1.,0.128450341339528));
#48756=CARTESIAN_POINT('Ctrl Pts',(-3.9272787679596,1.,0.130859892027798));
#48757=CARTESIAN_POINT('Ctrl Pts',(-3.93442567551035,1.,0.133319322794189));
#48758=CARTESIAN_POINT('Ctrl Pts',(-3.94156445130744,1.,0.135827558661188));
#48759=CARTESIAN_POINT('Ctrl Pts',(-3.94868667844355,1.,0.138383621255159));
#48760=CARTESIAN_POINT('Ctrl Pts',(-3.95579014116899,1.,0.140986665829937));
#48761=CARTESIAN_POINT('Ctrl Pts',(-3.96287658098896,1.,0.143635947692791));
#48762=CARTESIAN_POINT('Ctrl Pts',(-3.96995018565891,1.,0.146330797814513));
#48763=CARTESIAN_POINT('Ctrl Pts',(-3.97701581473643,1.,0.149070594803543));
#48764=CARTESIAN_POINT('Ctrl Pts',(-3.9840772985098,1.,0.151854737441405));
#48765=CARTESIAN_POINT('Ctrl Pts',(-3.99113582086059,1.,0.154682618338563));
#48766=CARTESIAN_POINT('Ctrl Pts',(-3.99819074631874,1.,0.157553634383809));
#48767=CARTESIAN_POINT('Ctrl Pts',(-4.00524031064509,1.,0.160467194882219));
#48768=CARTESIAN_POINT('Ctrl Pts',(-4.01228237022301,1.,0.163422730287458));
#48769=CARTESIAN_POINT('Ctrl Pts',(-4.01931510507143,1.,0.166419700015847));
#48770=CARTESIAN_POINT('Ctrl Pts',(-4.0263377970371,1.,0.169457601001653));
#48771=CARTESIAN_POINT('Ctrl Pts',(-4.03335057326093,1.,0.172535962484466));
#48772=CARTESIAN_POINT('Ctrl Pts',(-4.04035407891161,1.,0.175654339673757));
#48773=CARTESIAN_POINT('Ctrl Pts',(-4.04734916719722,1.,0.178812307240715));
#48774=CARTESIAN_POINT('Ctrl Pts',(-4.05433660358402,1.,0.18200945304855));
#48775=CARTESIAN_POINT('Ctrl Pts',(-4.06131670998589,1.,0.185245370038948));
#48776=CARTESIAN_POINT('Ctrl Pts',(-4.06828941192308,1.,0.188519658060255));
#48777=CARTESIAN_POINT('Ctrl Pts',(-4.07525439703137,1.,0.191831928181081));
#48778=CARTESIAN_POINT('Ctrl Pts',(-4.08221124060385,1.,0.195181806054714));
#48779=CARTESIAN_POINT('Ctrl Pts',(-4.08915953359753,1.,0.19856893480081));
#48780=CARTESIAN_POINT('Ctrl Pts',(-4.09609903751912,1.,0.201992979049984));
#48781=CARTESIAN_POINT('Ctrl Pts',(-4.10302969965374,1.,0.205453622198233));
#48782=CARTESIAN_POINT('Ctrl Pts',(-4.10995157639026,1.,0.208950559400172));
#48783=CARTESIAN_POINT('Ctrl Pts',(-4.11686478264545,1.,0.212483491087068));
#48784=CARTESIAN_POINT('Ctrl Pts',(-4.12376943492249,1.,0.216052116898425));
#48785=CARTESIAN_POINT('Ctrl Pts',(-4.13066558698156,1.,0.219656126701851));
#48786=CARTESIAN_POINT('Ctrl Pts',(-4.13755320553563,1.,0.223295201038383));
#48787=CARTESIAN_POINT('Ctrl Pts',(-4.14443220607733,1.,0.226969025061243));
#48788=CARTESIAN_POINT('Ctrl Pts',(-4.15130247435029,1.,0.230677299028738));
#48789=CARTESIAN_POINT('Ctrl Pts',(-4.1581638926525,1.,0.234419749543143));
#48790=CARTESIAN_POINT('Ctrl Pts',(-4.1650163665385,1.,0.238196140933976));
#48791=CARTESIAN_POINT('Ctrl Pts',(-4.17185984409533,1.,0.242006283923911));
#48792=CARTESIAN_POINT('Ctrl Pts',(-4.17869430192868,1.,0.245850033418583));
#48793=CARTESIAN_POINT('Ctrl Pts',(-4.18415464959491,1.,0.248951836910963));
#48794=CARTESIAN_POINT('Ctrl Pts',(-4.18824585244066,1.,0.251293239837692));
#48795=CARTESIAN_POINT('Ctrl Pts',(-4.19097151819241,1.,0.252860861572565));
#48796=CARTESIAN_POINT('Ctrl Pts',(-4.1923339003649,1.,0.253646344052521));
#48797=CARTESIAN_POINT('Origin',(-4.1923339003649,0.,0.253646344052521));
#48798=CARTESIAN_POINT('',(-4.18039834341342,1.,0.405301974318349));
#48799=CARTESIAN_POINT('Origin',(0.,0.,0.));
#48800=CARTESIAN_POINT('',(-3.74888939116259,1.,-0.0912596999148852));
#48801=CARTESIAN_POINT('Origin',(0.,1.,0.));
#48802=CARTESIAN_POINT('Ctrl Pts',(-3.74888939116259,1.,-0.091259699914886));
#48803=CARTESIAN_POINT('Ctrl Pts',(-3.74888939116259,0.666666666666667,
-0.091259699914886));
#48804=CARTESIAN_POINT('Ctrl Pts',(-3.74888939116259,0.333333333333333,
-0.091259699914886));
#48805=CARTESIAN_POINT('Ctrl Pts',(-3.74888939116259,-0.333333333333333,
-0.091259699914886));
#48806=CARTESIAN_POINT('Ctrl Pts',(-3.74888939116259,-0.666666666666667,
-0.0912596999148857));
#48807=CARTESIAN_POINT('Ctrl Pts',(-3.74888939116259,-1.,-0.0912596999148857));
#48808=CARTESIAN_POINT('Ctrl Pts',(-4.1923339003649,-1.,-0.253646344052522));
#48809=CARTESIAN_POINT('Ctrl Pts',(-4.1923339003649,1.,-0.253646344052522));
#48810=CARTESIAN_POINT('Ctrl Pts',(-4.19097151819684,-1.,-0.25286086157284));
#48811=CARTESIAN_POINT('Ctrl Pts',(-4.19097151819684,1.,-0.25286086157284));
#48812=CARTESIAN_POINT('Ctrl Pts',(-4.18824585245272,-1.,-0.251293239838441));
#48813=CARTESIAN_POINT('Ctrl Pts',(-4.18824585245272,1.,-0.251293239838441));
#48814=CARTESIAN_POINT('Ctrl Pts',(-4.18415464961466,-1.,-0.248951836912189));
#48815=CARTESIAN_POINT('Ctrl Pts',(-4.18415464961466,1.,-0.248951836912189));
#48816=CARTESIAN_POINT('Ctrl Pts',(-4.1786943019518,-1.,-0.245850033420019));
#48817=CARTESIAN_POINT('Ctrl Pts',(-4.1786943019518,1.,-0.245850033420019));
#48818=CARTESIAN_POINT('Ctrl Pts',(-4.17185984411426,-1.,-0.242006283925088));
#48819=CARTESIAN_POINT('Ctrl Pts',(-4.17185984411426,1.,-0.242006283925088));
#48820=CARTESIAN_POINT('Ctrl Pts',(-4.16501636654877,-1.,-0.238196140934616));
#48821=CARTESIAN_POINT('Ctrl Pts',(-4.16501636654877,1.,-0.238196140934616));
#48822=CARTESIAN_POINT('Ctrl Pts',(-4.15816389265352,-1.,-0.234419749543208));
#48823=CARTESIAN_POINT('Ctrl Pts',(-4.15816389265352,1.,-0.234419749543208));
#48824=CARTESIAN_POINT('Ctrl Pts',(-4.15130247434459,-1.,-0.230677299028383));
#48825=CARTESIAN_POINT('Ctrl Pts',(-4.15130247434459,1.,-0.230677299028383));
#48826=CARTESIAN_POINT('Ctrl Pts',(-4.14443220606869,-1.,-0.226969025060705));
#48827=CARTESIAN_POINT('Ctrl Pts',(-4.14443220606869,1.,-0.226969025060705));
#48828=CARTESIAN_POINT('Ctrl Pts',(-4.13755320552764,-1.,-0.223295201037886));
#48829=CARTESIAN_POINT('Ctrl Pts',(-4.13755320552764,1.,-0.223295201037886));
#48830=CARTESIAN_POINT('Ctrl Pts',(-4.13066558697658,-1.,-0.219656126701541));
#48831=CARTESIAN_POINT('Ctrl Pts',(-4.13066558697658,1.,-0.219656126701541));
#48832=CARTESIAN_POINT('Ctrl Pts',(-4.12376943492132,-1.,-0.216052116898352));
#48833=CARTESIAN_POINT('Ctrl Pts',(-4.12376943492132,1.,-0.216052116898352));
#48834=CARTESIAN_POINT('Ctrl Pts',(-4.11686478264739,-1.,-0.21248349108719));
#48835=CARTESIAN_POINT('Ctrl Pts',(-4.11686478264739,1.,-0.21248349108719));
#48836=CARTESIAN_POINT('Ctrl Pts',(-4.10995157639377,-1.,-0.208950559400392));
#48837=CARTESIAN_POINT('Ctrl Pts',(-4.10995157639377,1.,-0.208950559400392));
#48838=CARTESIAN_POINT('Ctrl Pts',(-4.10302969965728,-1.,-0.205453622198455));
#48839=CARTESIAN_POINT('Ctrl Pts',(-4.10302969965728,1.,-0.205453622198455));
#48840=CARTESIAN_POINT('Ctrl Pts',(-4.09609903752152,-1.,-0.201992979050136));
#48841=CARTESIAN_POINT('Ctrl Pts',(-4.09609903752152,1.,-0.201992979050136));
#48842=CARTESIAN_POINT('Ctrl Pts',(-4.08915953359833,-1.,-0.198568934800862));
#48843=CARTESIAN_POINT('Ctrl Pts',(-4.08915953359833,1.,-0.198568934800862));
#48844=CARTESIAN_POINT('Ctrl Pts',(-4.08221124060322,-1.,-0.195181806054676));
#48845=CARTESIAN_POINT('Ctrl Pts',(-4.08221124060322,1.,-0.195181806054676));
#48846=CARTESIAN_POINT('Ctrl Pts',(-4.07525439702992,-1.,-0.191831928180991));
#48847=CARTESIAN_POINT('Ctrl Pts',(-4.07525439702992,1.,-0.191831928180991));
#48848=CARTESIAN_POINT('Ctrl Pts',(-4.06828941192148,-1.,-0.188519658060155));
#48849=CARTESIAN_POINT('Ctrl Pts',(-4.06828941192148,1.,-0.188519658060155));
#48850=CARTESIAN_POINT('Ctrl Pts',(-4.06131670998469,-1.,-0.185245370038874));
#48851=CARTESIAN_POINT('Ctrl Pts',(-4.06131670998469,1.,-0.185245370038874));
#48852=CARTESIAN_POINT('Ctrl Pts',(-4.05433660358353,-1.,-0.18200945304852));
#48853=CARTESIAN_POINT('Ctrl Pts',(-4.05433660358353,1.,-0.18200945304852));
#48854=CARTESIAN_POINT('Ctrl Pts',(-4.04734916719741,-1.,-0.178812307240728));
#48855=CARTESIAN_POINT('Ctrl Pts',(-4.04734916719741,1.,-0.178812307240728));
#48856=CARTESIAN_POINT('Ctrl Pts',(-4.04035407891222,-1.,-0.175654339673797));
#48857=CARTESIAN_POINT('Ctrl Pts',(-4.04035407891222,1.,-0.175654339673797));
#48858=CARTESIAN_POINT('Ctrl Pts',(-4.03335057326163,-1.,-0.172535962484514));
#48859=CARTESIAN_POINT('Ctrl Pts',(-4.03335057326163,1.,-0.172535962484514));
#48860=CARTESIAN_POINT('Ctrl Pts',(-4.02633779703764,-1.,-0.169457601001691));
#48861=CARTESIAN_POINT('Ctrl Pts',(-4.02633779703764,1.,-0.169457601001691));
#48862=CARTESIAN_POINT('Ctrl Pts',(-4.01931510507167,-1.,-0.166419700015866));
#48863=CARTESIAN_POINT('Ctrl Pts',(-4.01931510507167,1.,-0.166419700015866));
#48864=CARTESIAN_POINT('Ctrl Pts',(-4.01228237022296,-1.,-0.163422730287456));
#48865=CARTESIAN_POINT('Ctrl Pts',(-4.01228237022296,1.,-0.163422730287456));
#48866=CARTESIAN_POINT('Ctrl Pts',(-4.00524031064487,-1.,-0.160467194882203));
#48867=CARTESIAN_POINT('Ctrl Pts',(-4.00524031064487,1.,-0.160467194882203));
#48868=CARTESIAN_POINT('Ctrl Pts',(-3.9981907463185,-1.,-0.15755363438379));
#48869=CARTESIAN_POINT('Ctrl Pts',(-3.9981907463185,1.,-0.15755363438379));
#48870=CARTESIAN_POINT('Ctrl Pts',(-3.99113582086043,-1.,-0.154682618338547));
#48871=CARTESIAN_POINT('Ctrl Pts',(-3.99113582086043,1.,-0.154682618338547));
#48872=CARTESIAN_POINT('Ctrl Pts',(-3.98407729850975,-1.,-0.151854737441398));
#48873=CARTESIAN_POINT('Ctrl Pts',(-3.98407729850975,1.,-0.151854737441398));
#48874=CARTESIAN_POINT('Ctrl Pts',(-3.97701581473644,-1.,-0.149070594803545));
#48875=CARTESIAN_POINT('Ctrl Pts',(-3.97701581473644,1.,-0.149070594803545));
#48876=CARTESIAN_POINT('Ctrl Pts',(-3.96995018565893,-1.,-0.14633079781452));
#48877=CARTESIAN_POINT('Ctrl Pts',(-3.96995018565893,1.,-0.14633079781452));
#48878=CARTESIAN_POINT('Ctrl Pts',(-3.96287658098896,-1.,-0.143635947692799));
#48879=CARTESIAN_POINT('Ctrl Pts',(-3.96287658098896,1.,-0.143635947692799));
#48880=CARTESIAN_POINT('Ctrl Pts',(-3.95579014116894,-1.,-0.140986665829942));
#48881=CARTESIAN_POINT('Ctrl Pts',(-3.95579014116894,1.,-0.140986665829942));
#48882=CARTESIAN_POINT('Ctrl Pts',(-3.94868667844347,-1.,-0.138383621255161));
#48883=CARTESIAN_POINT('Ctrl Pts',(-3.94868667844347,1.,-0.138383621255161));
#48884=CARTESIAN_POINT('Ctrl Pts',(-3.94156445130741,-1.,-0.135827558661188));
#48885=CARTESIAN_POINT('Ctrl Pts',(-3.94156445130741,1.,-0.135827558661188));
#48886=CARTESIAN_POINT('Ctrl Pts',(-3.93442567551042,-1.,-0.133319322794191));
#48887=CARTESIAN_POINT('Ctrl Pts',(-3.93442567551042,1.,-0.133319322794191));
#48888=CARTESIAN_POINT('Ctrl Pts',(-3.92727876795977,-1.,-0.130859892027801));
#48889=CARTESIAN_POINT('Ctrl Pts',(-3.92727876795977,1.,-0.130859892027801));
#48890=CARTESIAN_POINT('Ctrl Pts',(-3.92013513251664,-1.,-0.128450341339532));
#48891=CARTESIAN_POINT('Ctrl Pts',(-3.92013513251664,1.,-0.128450341339532));
#48892=CARTESIAN_POINT('Ctrl Pts',(-3.91300501605411,-1.,-0.126091793324141));
#48893=CARTESIAN_POINT('Ctrl Pts',(-3.91300501605411,1.,-0.126091793324141));
#48894=CARTESIAN_POINT('Ctrl Pts',(-3.90589336320515,-1.,-0.12378536827238));
#48895=CARTESIAN_POINT('Ctrl Pts',(-3.90589336320515,1.,-0.12378536827238));
#48896=CARTESIAN_POINT('Ctrl Pts',(-3.89879639336939,-1.,-0.121532144765721));
#48897=CARTESIAN_POINT('Ctrl Pts',(-3.89879639336939,1.,-0.121532144765721));
#48898=CARTESIAN_POINT('Ctrl Pts',(-3.8916960010517,-1.,-0.11933308819041));
#48899=CARTESIAN_POINT('Ctrl Pts',(-3.8916960010517,1.,-0.11933308819041));
#48900=CARTESIAN_POINT('Ctrl Pts',(-3.88456590045726,-1.,-0.117189150373134));
#48901=CARTESIAN_POINT('Ctrl Pts',(-3.88456590045726,1.,-0.117189150373134));
#48902=CARTESIAN_POINT('Ctrl Pts',(-3.87738168405308,-1.,-0.115101426649461));
#48903=CARTESIAN_POINT('Ctrl Pts',(-3.87738168405308,1.,-0.115101426649461));
#48904=CARTESIAN_POINT('Ctrl Pts',(-3.87013043445001,-1.,-0.113071304914559));
#48905=CARTESIAN_POINT('Ctrl Pts',(-3.87013043445001,1.,-0.113071304914559));
#48906=CARTESIAN_POINT('Ctrl Pts',(-3.86281867282984,-1.,-0.111100593036267));
#48907=CARTESIAN_POINT('Ctrl Pts',(-3.86281867282984,1.,-0.111100593036267));
#48908=CARTESIAN_POINT('Ctrl Pts',(-3.85548571496953,-1.,-0.109191717634961));
#48909=CARTESIAN_POINT('Ctrl Pts',(-3.85548571496953,1.,-0.109191717634961));
#48910=CARTESIAN_POINT('Ctrl Pts',(-3.84819233070391,-1.,-0.107347597812208));
#48911=CARTESIAN_POINT('Ctrl Pts',(-3.84819233070391,1.,-0.107347597812208));
#48912=CARTESIAN_POINT('Ctrl Pts',(-3.84099658324873,-1.,-0.105571360916593));
#48913=CARTESIAN_POINT('Ctrl Pts',(-3.84099658324873,1.,-0.105571360916593));
#48914=CARTESIAN_POINT('Ctrl Pts',(-3.83393171228034,-1.,-0.103866063811634));
#48915=CARTESIAN_POINT('Ctrl Pts',(-3.83393171228034,1.,-0.103866063811634));
#48916=CARTESIAN_POINT('Ctrl Pts',(-3.8269873714322,-1.,-0.102234506488445));
#48917=CARTESIAN_POINT('Ctrl Pts',(-3.8269873714322,1.,-0.102234506488445));
#48918=CARTESIAN_POINT('Ctrl Pts',(-3.82007889742512,-1.,-0.100678769650594));
#48919=CARTESIAN_POINT('Ctrl Pts',(-3.82007889742512,1.,-0.100678769650594));
#48920=CARTESIAN_POINT('Ctrl Pts',(-3.81306649386293,-1.,-0.0992008728095943));
#48921=CARTESIAN_POINT('Ctrl Pts',(-3.81306649386293,1.,-0.0992008728095943));
#48922=CARTESIAN_POINT('Ctrl Pts',(-3.80581088847642,-1.,-0.0978042222906075));
#48923=CARTESIAN_POINT('Ctrl Pts',(-3.80581088847642,1.,-0.0978042222906075));
#48924=CARTESIAN_POINT('Ctrl Pts',(-3.7982212851376,-1.,-0.0964949352872844));
#48925=CARTESIAN_POINT('Ctrl Pts',(-3.7982212851376,1.,-0.0964949352872844));
#48926=CARTESIAN_POINT('Ctrl Pts',(-3.79030016353186,-1.,-0.0952829885101068));
#48927=CARTESIAN_POINT('Ctrl Pts',(-3.79030016353186,1.,-0.0952829885101068));
#48928=CARTESIAN_POINT('Ctrl Pts',(-3.78220521899366,-1.,-0.0941840095091744));
#48929=CARTESIAN_POINT('Ctrl Pts',(-3.78220521899366,1.,-0.0941840095091744));
#48930=CARTESIAN_POINT('Ctrl Pts',(-3.77424159971456,-1.,-0.0932185546204574));
#48931=CARTESIAN_POINT('Ctrl Pts',(-3.77424159971456,1.,-0.0932185546204574));
#48932=CARTESIAN_POINT('Ctrl Pts',(-3.76678860032228,-1.,-0.0924090589604056));
#48933=CARTESIAN_POINT('Ctrl Pts',(-3.76678860032228,1.,-0.0924090589604056));
#48934=CARTESIAN_POINT('Ctrl Pts',(-3.76024199359493,-1.,-0.0917773084999007));
#48935=CARTESIAN_POINT('Ctrl Pts',(-3.76024199359493,1.,-0.0917773084999007));
#48936=CARTESIAN_POINT('Ctrl Pts',(-3.75495560118053,-1.,-0.0913419622735852));
#48937=CARTESIAN_POINT('Ctrl Pts',(-3.75495560118053,1.,-0.0913419622735852));
#48938=CARTESIAN_POINT('Ctrl Pts',(-3.75116949194125,-1.,-0.0911154000996406));
#48939=CARTESIAN_POINT('Ctrl Pts',(-3.75116949194125,1.,-0.0911154000996406));
#48940=CARTESIAN_POINT('Ctrl Pts',(-3.74943097853257,-1.,-0.091105754750466));
#48941=CARTESIAN_POINT('Ctrl Pts',(-3.74943097853257,1.,-0.091105754750466));
#48942=CARTESIAN_POINT('Ctrl Pts',(-3.7488701717383,-1.,-0.0911958743733925));
#48943=CARTESIAN_POINT('Ctrl Pts',(-3.7488701717383,1.,-0.0911958743733925));
#48944=CARTESIAN_POINT('Ctrl Pts',(-3.74882632118923,-1.,-0.0912992005792091));
#48945=CARTESIAN_POINT('Ctrl Pts',(-3.74882632118923,1.,-0.0912992005792091));
#48946=CARTESIAN_POINT('Ctrl Pts',(-3.74888690736767,-1.,-0.0913616755937429));
#48947=CARTESIAN_POINT('Ctrl Pts',(-3.74888690736767,1.,-0.0913616755937429));
#48948=CARTESIAN_POINT('',(-4.1923339003649,1.,-0.253646344052522));
#48949=CARTESIAN_POINT('Ctrl Pts',(-4.1923339003649,1.,-0.253646344052522));
#48950=CARTESIAN_POINT('Ctrl Pts',(-4.19097151819684,1.,-0.25286086157284));
#48951=CARTESIAN_POINT('Ctrl Pts',(-4.18824585245272,1.,-0.251293239838441));
#48952=CARTESIAN_POINT('Ctrl Pts',(-4.18415464961466,1.,-0.248951836912189));
#48953=CARTESIAN_POINT('Ctrl Pts',(-4.1786943019518,1.,-0.245850033420019));
#48954=CARTESIAN_POINT('Ctrl Pts',(-4.17185984411426,1.,-0.242006283925088));
#48955=CARTESIAN_POINT('Ctrl Pts',(-4.16501636654877,1.,-0.238196140934616));
#48956=CARTESIAN_POINT('Ctrl Pts',(-4.15816389265352,1.,-0.234419749543208));
#48957=CARTESIAN_POINT('Ctrl Pts',(-4.15130247434459,1.,-0.230677299028383));
#48958=CARTESIAN_POINT('Ctrl Pts',(-4.14443220606869,1.,-0.226969025060705));
#48959=CARTESIAN_POINT('Ctrl Pts',(-4.13755320552764,1.,-0.223295201037886));
#48960=CARTESIAN_POINT('Ctrl Pts',(-4.13066558697658,1.,-0.219656126701541));
#48961=CARTESIAN_POINT('Ctrl Pts',(-4.12376943492132,1.,-0.216052116898352));
#48962=CARTESIAN_POINT('Ctrl Pts',(-4.11686478264739,1.,-0.21248349108719));
#48963=CARTESIAN_POINT('Ctrl Pts',(-4.10995157639377,1.,-0.208950559400392));
#48964=CARTESIAN_POINT('Ctrl Pts',(-4.10302969965728,1.,-0.205453622198455));
#48965=CARTESIAN_POINT('Ctrl Pts',(-4.09609903752152,1.,-0.201992979050136));
#48966=CARTESIAN_POINT('Ctrl Pts',(-4.08915953359833,1.,-0.198568934800862));
#48967=CARTESIAN_POINT('Ctrl Pts',(-4.08221124060322,1.,-0.195181806054676));
#48968=CARTESIAN_POINT('Ctrl Pts',(-4.07525439702992,1.,-0.191831928180991));
#48969=CARTESIAN_POINT('Ctrl Pts',(-4.06828941192148,1.,-0.188519658060155));
#48970=CARTESIAN_POINT('Ctrl Pts',(-4.06131670998469,1.,-0.185245370038874));
#48971=CARTESIAN_POINT('Ctrl Pts',(-4.05433660358353,1.,-0.18200945304852));
#48972=CARTESIAN_POINT('Ctrl Pts',(-4.04734916719741,1.,-0.178812307240728));
#48973=CARTESIAN_POINT('Ctrl Pts',(-4.04035407891222,1.,-0.175654339673797));
#48974=CARTESIAN_POINT('Ctrl Pts',(-4.03335057326163,1.,-0.172535962484514));
#48975=CARTESIAN_POINT('Ctrl Pts',(-4.02633779703764,1.,-0.169457601001691));
#48976=CARTESIAN_POINT('Ctrl Pts',(-4.01931510507167,1.,-0.166419700015866));
#48977=CARTESIAN_POINT('Ctrl Pts',(-4.01228237022296,1.,-0.163422730287456));
#48978=CARTESIAN_POINT('Ctrl Pts',(-4.00524031064487,1.,-0.160467194882203));
#48979=CARTESIAN_POINT('Ctrl Pts',(-3.9981907463185,1.,-0.15755363438379));
#48980=CARTESIAN_POINT('Ctrl Pts',(-3.99113582086043,1.,-0.154682618338547));
#48981=CARTESIAN_POINT('Ctrl Pts',(-3.98407729850975,1.,-0.151854737441398));
#48982=CARTESIAN_POINT('Ctrl Pts',(-3.97701581473644,1.,-0.149070594803545));
#48983=CARTESIAN_POINT('Ctrl Pts',(-3.96995018565893,1.,-0.14633079781452));
#48984=CARTESIAN_POINT('Ctrl Pts',(-3.96287658098896,1.,-0.143635947692799));
#48985=CARTESIAN_POINT('Ctrl Pts',(-3.95579014116894,1.,-0.140986665829942));
#48986=CARTESIAN_POINT('Ctrl Pts',(-3.94868667844347,1.,-0.138383621255161));
#48987=CARTESIAN_POINT('Ctrl Pts',(-3.94156445130741,1.,-0.135827558661188));
#48988=CARTESIAN_POINT('Ctrl Pts',(-3.93442567551042,1.,-0.133319322794191));
#48989=CARTESIAN_POINT('Ctrl Pts',(-3.92727876795977,1.,-0.130859892027801));
#48990=CARTESIAN_POINT('Ctrl Pts',(-3.92013513251664,1.,-0.128450341339532));
#48991=CARTESIAN_POINT('Ctrl Pts',(-3.91300501605411,1.,-0.126091793324141));
#48992=CARTESIAN_POINT('Ctrl Pts',(-3.90589336320515,1.,-0.12378536827238));
#48993=CARTESIAN_POINT('Ctrl Pts',(-3.89879639336939,1.,-0.121532144765721));
#48994=CARTESIAN_POINT('Ctrl Pts',(-3.8916960010517,1.,-0.11933308819041));
#48995=CARTESIAN_POINT('Ctrl Pts',(-3.88456590045726,1.,-0.117189150373134));
#48996=CARTESIAN_POINT('Ctrl Pts',(-3.87738168405308,1.,-0.115101426649461));
#48997=CARTESIAN_POINT('Ctrl Pts',(-3.87013043445001,1.,-0.113071304914559));
#48998=CARTESIAN_POINT('Ctrl Pts',(-3.86281867282984,1.,-0.111100593036267));
#48999=CARTESIAN_POINT('Ctrl Pts',(-3.85548571496953,1.,-0.109191717634961));
#49000=CARTESIAN_POINT('Ctrl Pts',(-3.84819233070391,1.,-0.107347597812208));
#49001=CARTESIAN_POINT('Ctrl Pts',(-3.84099658324873,1.,-0.105571360916593));
#49002=CARTESIAN_POINT('Ctrl Pts',(-3.83393171228034,1.,-0.103866063811634));
#49003=CARTESIAN_POINT('Ctrl Pts',(-3.8269873714322,1.,-0.102234506488445));
#49004=CARTESIAN_POINT('Ctrl Pts',(-3.82007889742512,1.,-0.100678769650594));
#49005=CARTESIAN_POINT('Ctrl Pts',(-3.81306649386293,1.,-0.0992008728095943));
#49006=CARTESIAN_POINT('Ctrl Pts',(-3.80581088847642,1.,-0.0978042222906075));
#49007=CARTESIAN_POINT('Ctrl Pts',(-3.7982212851376,1.,-0.0964949352872844));
#49008=CARTESIAN_POINT('Ctrl Pts',(-3.79030016353186,1.,-0.0952829885101068));
#49009=CARTESIAN_POINT('Ctrl Pts',(-3.78220521899366,1.,-0.0941840095091744));
#49010=CARTESIAN_POINT('Ctrl Pts',(-3.77424159971456,1.,-0.0932185546204574));
#49011=CARTESIAN_POINT('Ctrl Pts',(-3.76678860032228,1.,-0.0924090589604056));
#49012=CARTESIAN_POINT('Ctrl Pts',(-3.76024199359493,1.,-0.0917773084999007));
#49013=CARTESIAN_POINT('Ctrl Pts',(-3.75495560118053,1.,-0.0913419622735852));
#49014=CARTESIAN_POINT('Ctrl Pts',(-3.75145357872511,1.,-0.0911323999576144));
#49015=CARTESIAN_POINT('Ctrl Pts',(-3.74976844886495,1.,-0.0911090736804571));
#49016=CARTESIAN_POINT('Ctrl Pts',(-3.74911539914664,1.,-0.0911666301806425));
#49017=CARTESIAN_POINT('Ctrl Pts',(-3.74892890041021,1.,-0.0912308016409232));
#49018=CARTESIAN_POINT('Ctrl Pts',(-3.74888939116259,1.,-0.0912596999148857));
#49019=CARTESIAN_POINT('',(-4.1923339003649,0.,-0.253646344052522));
#49020=CARTESIAN_POINT('Ctrl Pts',(-3.71702400346349,-1.,-0.496218256089212));
#49021=CARTESIAN_POINT('Ctrl Pts',(-3.71702400346349,1.,-0.496218256089212));
#49022=CARTESIAN_POINT('Ctrl Pts',(-3.7169543899574,-1.,-0.496270484166409));
#49023=CARTESIAN_POINT('Ctrl Pts',(-3.7169543899574,1.,-0.496270484166409));
#49024=CARTESIAN_POINT('Ctrl Pts',(-3.71698153685602,-1.,-0.49637939799264));
#49025=CARTESIAN_POINT('Ctrl Pts',(-3.71698153685602,1.,-0.49637939799264));
#49026=CARTESIAN_POINT('Ctrl Pts',(-3.71752134137482,-1.,-0.496556137604532));
#49027=CARTESIAN_POINT('Ctrl Pts',(-3.71752134137482,1.,-0.496556137604532));
#49028=CARTESIAN_POINT('Ctrl Pts',(-3.71923995966302,-1.,-0.496818574420596));
#49029=CARTESIAN_POINT('Ctrl Pts',(-3.71923995966302,1.,-0.496818574420596));
#49030=CARTESIAN_POINT('Ctrl Pts',(-3.72301489774398,-1.,-0.497187079575988));
#49031=CARTESIAN_POINT('Ctrl Pts',(-3.72301489774398,1.,-0.497187079575988));
#49032=CARTESIAN_POINT('Ctrl Pts',(-3.72830430904606,-1.,-0.497584067153049));
#49033=CARTESIAN_POINT('Ctrl Pts',(-3.72830430904606,1.,-0.497584067153049));
#49034=CARTESIAN_POINT('Ctrl Pts',(-3.73486914372449,-1.,-0.497984209510024));
#49035=CARTESIAN_POINT('Ctrl Pts',(-3.73486914372449,1.,-0.497984209510024));
#49036=CARTESIAN_POINT('Ctrl Pts',(-3.74235701734714,-1.,-0.498350586057692));
#49037=CARTESIAN_POINT('Ctrl Pts',(-3.74235701734714,1.,-0.498350586057692));
#49038=CARTESIAN_POINT('Ctrl Pts',(-3.75037362167839,-1.,-0.498642802042606));
#49039=CARTESIAN_POINT('Ctrl Pts',(-3.75037362167839,1.,-0.498642802042606));
#49040=CARTESIAN_POINT('Ctrl Pts',(-3.75854082221053,-1.,-0.498823681615422));
#49041=CARTESIAN_POINT('Ctrl Pts',(-3.75854082221053,1.,-0.498823681615422));
#49042=CARTESIAN_POINT('Ctrl Pts',(-3.76655401191229,-1.,-0.49886579233529));
#49043=CARTESIAN_POINT('Ctrl Pts',(-3.76655401191229,1.,-0.49886579233529));
#49044=CARTESIAN_POINT('Ctrl Pts',(-3.77425499225255,-1.,-0.498759900365892));
#49045=CARTESIAN_POINT('Ctrl Pts',(-3.77425499225255,1.,-0.498759900365892));
#49046=CARTESIAN_POINT('Ctrl Pts',(-3.78163975337356,-1.,-0.498515471679585));
#49047=CARTESIAN_POINT('Ctrl Pts',(-3.78163975337356,1.,-0.498515471679585));
#49048=CARTESIAN_POINT('Ctrl Pts',(-3.78879701661264,-1.,-0.498152751800958));
#49049=CARTESIAN_POINT('Ctrl Pts',(-3.78879701661264,1.,-0.498152751800958));
#49050=CARTESIAN_POINT('Ctrl Pts',(-3.79586380669994,-1.,-0.497696892100625));
#49051=CARTESIAN_POINT('Ctrl Pts',(-3.79586380669994,1.,-0.497696892100625));
#49052=CARTESIAN_POINT('Ctrl Pts',(-3.80297788298514,-1.,-0.497171756201052));
#49053=CARTESIAN_POINT('Ctrl Pts',(-3.80297788298514,1.,-0.497171756201052));
#49054=CARTESIAN_POINT('Ctrl Pts',(-3.81022254090839,-1.,-0.496592643443704));
#49055=CARTESIAN_POINT('Ctrl Pts',(-3.81022254090839,1.,-0.496592643443704));
#49056=CARTESIAN_POINT('Ctrl Pts',(-3.81760756144025,-1.,-0.49596393787548));
#49057=CARTESIAN_POINT('Ctrl Pts',(-3.81760756144025,1.,-0.49596393787548));
#49058=CARTESIAN_POINT('Ctrl Pts',(-3.82509963594103,-1.,-0.495283458893837));
#49059=CARTESIAN_POINT('Ctrl Pts',(-3.82509963594103,1.,-0.495283458893837));
#49060=CARTESIAN_POINT('Ctrl Pts',(-3.83264092682431,-1.,-0.494545212256401));
#49061=CARTESIAN_POINT('Ctrl Pts',(-3.83264092682431,1.,-0.494545212256401));
#49062=CARTESIAN_POINT('Ctrl Pts',(-3.84017095578451,-1.,-0.493742574629134));
#49063=CARTESIAN_POINT('Ctrl Pts',(-3.84017095578451,1.,-0.493742574629134));
#49064=CARTESIAN_POINT('Ctrl Pts',(-3.84765051147999,-1.,-0.492871792414141));
#49065=CARTESIAN_POINT('Ctrl Pts',(-3.84765051147999,1.,-0.492871792414141));
#49066=CARTESIAN_POINT('Ctrl Pts',(-3.85507287020263,-1.,-0.491933631083813));
#49067=CARTESIAN_POINT('Ctrl Pts',(-3.85507287020263,1.,-0.491933631083813));
#49068=CARTESIAN_POINT('Ctrl Pts',(-3.86245057319246,-1.,-0.490931482170891));
#49069=CARTESIAN_POINT('Ctrl Pts',(-3.86245057319246,1.,-0.490931482170891));
#49070=CARTESIAN_POINT('Ctrl Pts',(-3.86980755613707,-1.,-0.489870245704918));
#49071=CARTESIAN_POINT('Ctrl Pts',(-3.86980755613707,1.,-0.489870245704918));
#49072=CARTESIAN_POINT('Ctrl Pts',(-3.87716963231109,-1.,-0.488754973798274));
#49073=CARTESIAN_POINT('Ctrl Pts',(-3.87716963231109,1.,-0.488754973798274));
#49074=CARTESIAN_POINT('Ctrl Pts',(-3.88455453328138,-1.,-0.487589452275154));
#49075=CARTESIAN_POINT('Ctrl Pts',(-3.88455453328138,1.,-0.487589452275154));
#49076=CARTESIAN_POINT('Ctrl Pts',(-3.89196582437552,-1.,-0.486375337854103));
#49077=CARTESIAN_POINT('Ctrl Pts',(-3.89196582437552,1.,-0.486375337854103));
#49078=CARTESIAN_POINT('Ctrl Pts',(-3.89939844658513,-1.,-0.485112963522222));
#49079=CARTESIAN_POINT('Ctrl Pts',(-3.89939844658513,1.,-0.485112963522222));
#49080=CARTESIAN_POINT('Ctrl Pts',(-3.90684210358056,-1.,-0.48380183508915));
#49081=CARTESIAN_POINT('Ctrl Pts',(-3.90684210358056,1.,-0.48380183508915));
#49082=CARTESIAN_POINT('Ctrl Pts',(-3.91428536373751,-1.,-0.482441230340713));
#49083=CARTESIAN_POINT('Ctrl Pts',(-3.91428536373751,1.,-0.482441230340713));
#49084=CARTESIAN_POINT('Ctrl Pts',(-3.92171976072341,-1.,-0.481030798910748));
#49085=CARTESIAN_POINT('Ctrl Pts',(-3.92171976072341,1.,-0.481030798910748));
#49086=CARTESIAN_POINT('Ctrl Pts',(-3.92914297392071,-1.,-0.479571028525579));
#49087=CARTESIAN_POINT('Ctrl Pts',(-3.92914297392071,1.,-0.479571028525579));
#49088=CARTESIAN_POINT('Ctrl Pts',(-3.93655660689819,-1.,-0.478062927140964));
#49089=CARTESIAN_POINT('Ctrl Pts',(-3.93655660689819,1.,-0.478062927140964));
#49090=CARTESIAN_POINT('Ctrl Pts',(-3.94396469119383,-1.,-0.476507810658537));
#49091=CARTESIAN_POINT('Ctrl Pts',(-3.94396469119383,1.,-0.476507810658537));
#49092=CARTESIAN_POINT('Ctrl Pts',(-3.95137192932897,-1.,-0.47490705302179));
#49093=CARTESIAN_POINT('Ctrl Pts',(-3.95137192932897,1.,-0.47490705302179));
#49094=CARTESIAN_POINT('Ctrl Pts',(-3.95878201038338,-1.,-0.473261847236297));
#49095=CARTESIAN_POINT('Ctrl Pts',(-3.95878201038338,1.,-0.473261847236297));
#49096=CARTESIAN_POINT('Ctrl Pts',(-3.96619600864643,-1.,-0.471572978413503));
#49097=CARTESIAN_POINT('Ctrl Pts',(-3.96619600864643,1.,-0.471572978413503));
#49098=CARTESIAN_POINT('Ctrl Pts',(-3.97361320212436,-1.,-0.469840942829895));
#49099=CARTESIAN_POINT('Ctrl Pts',(-3.97361320212436,1.,-0.469840942829895));
#49100=CARTESIAN_POINT('Ctrl Pts',(-3.98103175589371,-1.,-0.468066047920157));
#49101=CARTESIAN_POINT('Ctrl Pts',(-3.98103175589371,1.,-0.468066047920157));
#49102=CARTESIAN_POINT('Ctrl Pts',(-3.98844946363262,-1.,-0.46624852088304));
#49103=CARTESIAN_POINT('Ctrl Pts',(-3.98844946363262,1.,-0.46624852088304));
#49104=CARTESIAN_POINT('Ctrl Pts',(-3.9958644432011,-1.,-0.464388610938975));
#49105=CARTESIAN_POINT('Ctrl Pts',(-3.9958644432011,1.,-0.464388610938975));
#49106=CARTESIAN_POINT('Ctrl Pts',(-4.00327590659075,-1.,-0.462486702616205));
#49107=CARTESIAN_POINT('Ctrl Pts',(-4.00327590659075,1.,-0.462486702616205));
#49108=CARTESIAN_POINT('Ctrl Pts',(-4.01068390573399,-1.,-0.460543280768515));
#49109=CARTESIAN_POINT('Ctrl Pts',(-4.01068390573399,1.,-0.460543280768515));
#49110=CARTESIAN_POINT('Ctrl Pts',(-4.01808900827587,-1.,-0.458558885636945));
#49111=CARTESIAN_POINT('Ctrl Pts',(-4.01808900827587,1.,-0.458558885636945));
#49112=CARTESIAN_POINT('Ctrl Pts',(-4.02549199038394,-1.,-0.456534070784951));
#49113=CARTESIAN_POINT('Ctrl Pts',(-4.02549199038394,1.,-0.456534070784951));
#49114=CARTESIAN_POINT('Ctrl Pts',(-4.03289354362794,-1.,-0.454469363020542));
#49115=CARTESIAN_POINT('Ctrl Pts',(-4.03289354362794,1.,-0.454469363020542));
#49116=CARTESIAN_POINT('Ctrl Pts',(-4.04029392228049,-1.,-0.452365214748892));
#49117=CARTESIAN_POINT('Ctrl Pts',(-4.04029392228049,1.,-0.452365214748892));
#49118=CARTESIAN_POINT('Ctrl Pts',(-4.0476929901813,-1.,-0.450222009543926));
#49119=CARTESIAN_POINT('Ctrl Pts',(-4.0476929901813,1.,-0.450222009543926));
#49120=CARTESIAN_POINT('Ctrl Pts',(-4.0550903779696,-1.,-0.448040082684114));
#49121=CARTESIAN_POINT('Ctrl Pts',(-4.0550903779696,1.,-0.448040082684114));
#49122=CARTESIAN_POINT('Ctrl Pts',(-4.06248560760659,-1.,-0.445819737468538));
#49123=CARTESIAN_POINT('Ctrl Pts',(-4.06248560760659,1.,-0.445819737468538));
#49124=CARTESIAN_POINT('Ctrl Pts',(-4.0698782192569,-1.,-0.443561262395333));
#49125=CARTESIAN_POINT('Ctrl Pts',(-4.0698782192569,1.,-0.443561262395333));
#49126=CARTESIAN_POINT('Ctrl Pts',(-4.07726792490016,-1.,-0.44126495139636));
#49127=CARTESIAN_POINT('Ctrl Pts',(-4.07726792490016,1.,-0.44126495139636));
#49128=CARTESIAN_POINT('Ctrl Pts',(-4.08465462294273,-1.,-0.438931108931279));
#49129=CARTESIAN_POINT('Ctrl Pts',(-4.08465462294273,1.,-0.438931108931279));
#49130=CARTESIAN_POINT('Ctrl Pts',(-4.09203832139089,-1.,-0.436560044913482));
#49131=CARTESIAN_POINT('Ctrl Pts',(-4.09203832139089,1.,-0.436560044913482));
#49132=CARTESIAN_POINT('Ctrl Pts',(-4.09941908688373,-1.,-0.43415207320046));
#49133=CARTESIAN_POINT('Ctrl Pts',(-4.09941908688373,1.,-0.43415207320046));
#49134=CARTESIAN_POINT('Ctrl Pts',(-4.10679698750336,-1.,-0.431707508679884));
#49135=CARTESIAN_POINT('Ctrl Pts',(-4.10679698750336,1.,-0.431707508679884));
#49136=CARTESIAN_POINT('Ctrl Pts',(-4.11417202783267,-1.,-0.429226666075845));
#49137=CARTESIAN_POINT('Ctrl Pts',(-4.11417202783267,1.,-0.429226666075845));
#49138=CARTESIAN_POINT('Ctrl Pts',(-4.12154412502007,-1.,-0.426709855707));
#49139=CARTESIAN_POINT('Ctrl Pts',(-4.12154412502007,1.,-0.426709855707));
#49140=CARTESIAN_POINT('Ctrl Pts',(-4.12891314634572,-1.,-0.424157375323975));
#49141=CARTESIAN_POINT('Ctrl Pts',(-4.12891314634572,1.,-0.424157375323975));
#49142=CARTESIAN_POINT('Ctrl Pts',(-4.13627893207002,-1.,-0.421569503104513));
#49143=CARTESIAN_POINT('Ctrl Pts',(-4.13627893207002,1.,-0.421569503104513));
#49144=CARTESIAN_POINT('Ctrl Pts',(-4.14364132317121,-1.,-0.418946490667703));
#49145=CARTESIAN_POINT('Ctrl Pts',(-4.14364132317121,1.,-0.418946490667703));
#49146=CARTESIAN_POINT('Ctrl Pts',(-4.15100018949965,-1.,-0.416288556008012));
#49147=CARTESIAN_POINT('Ctrl Pts',(-4.15100018949965,1.,-0.416288556008012));
#49148=CARTESIAN_POINT('Ctrl Pts',(-4.15835545017202,-1.,-0.41359587795147));
#49149=CARTESIAN_POINT('Ctrl Pts',(-4.15835545017202,1.,-0.41359587795147));
#49150=CARTESIAN_POINT('Ctrl Pts',(-4.16570705938425,-1.,-0.410868596146414));
#49151=CARTESIAN_POINT('Ctrl Pts',(-4.16570705938425,1.,-0.410868596146414));
#49152=CARTESIAN_POINT('Ctrl Pts',(-4.17158541007977,-1.,-0.408659167568273));
#49153=CARTESIAN_POINT('Ctrl Pts',(-4.17158541007977,1.,-0.408659167568273));
#49154=CARTESIAN_POINT('Ctrl Pts',(-4.17599251954382,-1.,-0.406986596325455));
#49155=CARTESIAN_POINT('Ctrl Pts',(-4.17599251954382,1.,-0.406986596325455));
#49156=CARTESIAN_POINT('Ctrl Pts',(-4.17892985789466,-1.,-0.40586466267921));
#49157=CARTESIAN_POINT('Ctrl Pts',(-4.17892985789466,1.,-0.40586466267921));
#49158=CARTESIAN_POINT('Ctrl Pts',(-4.18039834341342,-1.,-0.40530197431835));
#49159=CARTESIAN_POINT('Ctrl Pts',(-4.18039834341342,1.,-0.40530197431835));
#49160=CARTESIAN_POINT('',(-3.71701050416825,1.,-0.496319364827592));
#49161=CARTESIAN_POINT('Ctrl Pts',(-3.71701050416825,-1.,-0.496319364827592));
#49162=CARTESIAN_POINT('Ctrl Pts',(-3.71701050416825,-0.666666666666667,
-0.496319364827592));
#49163=CARTESIAN_POINT('Ctrl Pts',(-3.71701050416825,-0.333333333333333,
-0.496319364827592));
#49164=CARTESIAN_POINT('Ctrl Pts',(-3.71701050416825,0.333333333333333,
-0.496319364827592));
#49165=CARTESIAN_POINT('Ctrl Pts',(-3.71701050416825,0.666666666666667,
-0.496319364827592));
#49166=CARTESIAN_POINT('Ctrl Pts',(-3.71701050416825,1.,-0.496319364827592));
#49167=CARTESIAN_POINT('',(-4.18039834341342,1.,-0.40530197431835));
#49168=CARTESIAN_POINT('',(-4.18039834341342,0.,-0.40530197431835));
#49169=CARTESIAN_POINT('Ctrl Pts',(-3.71701050416825,1.,-0.496319364827592));
#49170=CARTESIAN_POINT('Ctrl Pts',(-3.71704500630495,1.,-0.496354087924312));
#49171=CARTESIAN_POINT('Ctrl Pts',(-3.71721917030355,1.,-0.496446644158005));
#49172=CARTESIAN_POINT('Ctrl Pts',(-3.71785517607549,1.,-0.496605651525989));
#49173=CARTESIAN_POINT('Ctrl Pts',(-3.71952320822499,1.,-0.496846224822563));
#49174=CARTESIAN_POINT('Ctrl Pts',(-3.72301489774398,1.,-0.497187079575988));
#49175=CARTESIAN_POINT('Ctrl Pts',(-3.72830430904606,1.,-0.497584067153049));
#49176=CARTESIAN_POINT('Ctrl Pts',(-3.73486914372449,1.,-0.497984209510024));
#49177=CARTESIAN_POINT('Ctrl Pts',(-3.74235701734714,1.,-0.498350586057692));
#49178=CARTESIAN_POINT('Ctrl Pts',(-3.75037362167839,1.,-0.498642802042606));
#49179=CARTESIAN_POINT('Ctrl Pts',(-3.75854082221053,1.,-0.498823681615422));
#49180=CARTESIAN_POINT('Ctrl Pts',(-3.76655401191229,1.,-0.49886579233529));
#49181=CARTESIAN_POINT('Ctrl Pts',(-3.77425499225255,1.,-0.498759900365892));
#49182=CARTESIAN_POINT('Ctrl Pts',(-3.78163975337356,1.,-0.498515471679585));
#49183=CARTESIAN_POINT('Ctrl Pts',(-3.78879701661264,1.,-0.498152751800958));
#49184=CARTESIAN_POINT('Ctrl Pts',(-3.79586380669994,1.,-0.497696892100625));
#49185=CARTESIAN_POINT('Ctrl Pts',(-3.80297788298514,1.,-0.497171756201052));
#49186=CARTESIAN_POINT('Ctrl Pts',(-3.81022254090839,1.,-0.496592643443704));
#49187=CARTESIAN_POINT('Ctrl Pts',(-3.81760756144025,1.,-0.49596393787548));
#49188=CARTESIAN_POINT('Ctrl Pts',(-3.82509963594103,1.,-0.495283458893837));
#49189=CARTESIAN_POINT('Ctrl Pts',(-3.83264092682431,1.,-0.494545212256401));
#49190=CARTESIAN_POINT('Ctrl Pts',(-3.84017095578451,1.,-0.493742574629134));
#49191=CARTESIAN_POINT('Ctrl Pts',(-3.84765051147999,1.,-0.492871792414141));
#49192=CARTESIAN_POINT('Ctrl Pts',(-3.85507287020263,1.,-0.491933631083813));
#49193=CARTESIAN_POINT('Ctrl Pts',(-3.86245057319246,1.,-0.490931482170891));
#49194=CARTESIAN_POINT('Ctrl Pts',(-3.86980755613707,1.,-0.489870245704918));
#49195=CARTESIAN_POINT('Ctrl Pts',(-3.87716963231109,1.,-0.488754973798274));
#49196=CARTESIAN_POINT('Ctrl Pts',(-3.88455453328138,1.,-0.487589452275154));
#49197=CARTESIAN_POINT('Ctrl Pts',(-3.89196582437552,1.,-0.486375337854103));
#49198=CARTESIAN_POINT('Ctrl Pts',(-3.89939844658513,1.,-0.485112963522222));
#49199=CARTESIAN_POINT('Ctrl Pts',(-3.90684210358056,1.,-0.48380183508915));
#49200=CARTESIAN_POINT('Ctrl Pts',(-3.91428536373751,1.,-0.482441230340713));
#49201=CARTESIAN_POINT('Ctrl Pts',(-3.92171976072341,1.,-0.481030798910748));
#49202=CARTESIAN_POINT('Ctrl Pts',(-3.92914297392071,1.,-0.479571028525579));
#49203=CARTESIAN_POINT('Ctrl Pts',(-3.93655660689819,1.,-0.478062927140964));
#49204=CARTESIAN_POINT('Ctrl Pts',(-3.94396469119383,1.,-0.476507810658537));
#49205=CARTESIAN_POINT('Ctrl Pts',(-3.95137192932897,1.,-0.47490705302179));
#49206=CARTESIAN_POINT('Ctrl Pts',(-3.95878201038338,1.,-0.473261847236297));
#49207=CARTESIAN_POINT('Ctrl Pts',(-3.96619600864643,1.,-0.471572978413503));
#49208=CARTESIAN_POINT('Ctrl Pts',(-3.97361320212436,1.,-0.469840942829895));
#49209=CARTESIAN_POINT('Ctrl Pts',(-3.98103175589371,1.,-0.468066047920157));
#49210=CARTESIAN_POINT('Ctrl Pts',(-3.98844946363262,1.,-0.46624852088304));
#49211=CARTESIAN_POINT('Ctrl Pts',(-3.9958644432011,1.,-0.464388610938975));
#49212=CARTESIAN_POINT('Ctrl Pts',(-4.00327590659075,1.,-0.462486702616205));
#49213=CARTESIAN_POINT('Ctrl Pts',(-4.01068390573399,1.,-0.460543280768515));
#49214=CARTESIAN_POINT('Ctrl Pts',(-4.01808900827587,1.,-0.458558885636945));
#49215=CARTESIAN_POINT('Ctrl Pts',(-4.02549199038394,1.,-0.456534070784951));
#49216=CARTESIAN_POINT('Ctrl Pts',(-4.03289354362794,1.,-0.454469363020542));
#49217=CARTESIAN_POINT('Ctrl Pts',(-4.04029392228049,1.,-0.452365214748892));
#49218=CARTESIAN_POINT('Ctrl Pts',(-4.0476929901813,1.,-0.450222009543926));
#49219=CARTESIAN_POINT('Ctrl Pts',(-4.0550903779696,1.,-0.448040082684114));
#49220=CARTESIAN_POINT('Ctrl Pts',(-4.06248560760659,1.,-0.445819737468538));
#49221=CARTESIAN_POINT('Ctrl Pts',(-4.0698782192569,1.,-0.443561262395333));
#49222=CARTESIAN_POINT('Ctrl Pts',(-4.07726792490016,1.,-0.44126495139636));
#49223=CARTESIAN_POINT('Ctrl Pts',(-4.08465462294273,1.,-0.438931108931279));
#49224=CARTESIAN_POINT('Ctrl Pts',(-4.09203832139089,1.,-0.436560044913482));
#49225=CARTESIAN_POINT('Ctrl Pts',(-4.09941908688373,1.,-0.43415207320046));
#49226=CARTESIAN_POINT('Ctrl Pts',(-4.10679698750336,1.,-0.431707508679884));
#49227=CARTESIAN_POINT('Ctrl Pts',(-4.11417202783267,1.,-0.429226666075845));
#49228=CARTESIAN_POINT('Ctrl Pts',(-4.12154412502007,1.,-0.426709855707));
#49229=CARTESIAN_POINT('Ctrl Pts',(-4.12891314634572,1.,-0.424157375323975));
#49230=CARTESIAN_POINT('Ctrl Pts',(-4.13627893207002,1.,-0.421569503104513));
#49231=CARTESIAN_POINT('Ctrl Pts',(-4.14364132317121,1.,-0.418946490667703));
#49232=CARTESIAN_POINT('Ctrl Pts',(-4.15100018949965,1.,-0.416288556008012));
#49233=CARTESIAN_POINT('Ctrl Pts',(-4.15835545017202,1.,-0.41359587795147));
#49234=CARTESIAN_POINT('Ctrl Pts',(-4.16570705938425,1.,-0.410868596146414));
#49235=CARTESIAN_POINT('Ctrl Pts',(-4.17158541007977,1.,-0.408659167568273));
#49236=CARTESIAN_POINT('Ctrl Pts',(-4.17599251954382,1.,-0.406986596325455));
#49237=CARTESIAN_POINT('Ctrl Pts',(-4.17892985789466,1.,-0.40586466267921));
#49238=CARTESIAN_POINT('Ctrl Pts',(-4.18039834341342,1.,-0.40530197431835));
#49239=CARTESIAN_POINT('Origin',(-4.18039834341342,0.,-0.40530197431835));
#49240=CARTESIAN_POINT('',(-4.1923339003649,1.,-0.253646344052522));
#49241=CARTESIAN_POINT('Origin',(0.,0.,0.));
#49242=CARTESIAN_POINT('',(-3.68845817949618,1.,-0.67659164797366));
#49243=CARTESIAN_POINT('Origin',(0.,1.,0.));
#49244=CARTESIAN_POINT('Ctrl Pts',(-3.68845817949618,1.,-0.676591647973661));
#49245=CARTESIAN_POINT('Ctrl Pts',(-3.68845817949618,0.666666666666667,
-0.676591647973661));
#49246=CARTESIAN_POINT('Ctrl Pts',(-3.68845817949618,0.333333333333333,
-0.676591647973661));
#49247=CARTESIAN_POINT('Ctrl Pts',(-3.68845817949618,-0.333333333333333,
-0.676591647973661));
#49248=CARTESIAN_POINT('Ctrl Pts',(-3.68845817949618,-0.666666666666667,
-0.676591647973661));
#49249=CARTESIAN_POINT('Ctrl Pts',(-3.68845817949618,-1.,-0.676591647973661));
#49250=CARTESIAN_POINT('Ctrl Pts',(-4.10104028313088,-1.,-0.906349047628866));
#49251=CARTESIAN_POINT('Ctrl Pts',(-4.10104028313088,1.,-0.906349047628866));
#49252=CARTESIAN_POINT('Ctrl Pts',(-4.09981755067956,-1.,-0.905360112216302));
#49253=CARTESIAN_POINT('Ctrl Pts',(-4.09981755067956,1.,-0.905360112216302));
#49254=CARTESIAN_POINT('Ctrl Pts',(-4.09737067247114,-1.,-0.903385402444212));
#49255=CARTESIAN_POINT('Ctrl Pts',(-4.09737067247114,1.,-0.903385402444212));
#49256=CARTESIAN_POINT('Ctrl Pts',(-4.09369611524319,-1.,-0.900432820945975));
#49257=CARTESIAN_POINT('Ctrl Pts',(-4.09369611524319,1.,-0.900432820945975));
#49258=CARTESIAN_POINT('Ctrl Pts',(-4.08878822249095,-1.,-0.896515019236368));
#49259=CARTESIAN_POINT('Ctrl Pts',(-4.08878822249095,1.,-0.896515019236368));
#49260=CARTESIAN_POINT('Ctrl Pts',(-4.08263920306651,-1.,-0.891649447920401));
#49261=CARTESIAN_POINT('Ctrl Pts',(-4.08263920306651,1.,-0.891649447920401));
#49262=CARTESIAN_POINT('Ctrl Pts',(-4.07647601774639,-1.,-0.886815658360739));
#49263=CARTESIAN_POINT('Ctrl Pts',(-4.07647601774639,1.,-0.886815658360739));
#49264=CARTESIAN_POINT('Ctrl Pts',(-4.07029866694292,-1.,-0.882013797525916));
#49265=CARTESIAN_POINT('Ctrl Pts',(-4.07029866694292,1.,-0.882013797525916));
#49266=CARTESIAN_POINT('Ctrl Pts',(-4.06410717232347,-1.,-0.877244060484595));
#49267=CARTESIAN_POINT('Ctrl Pts',(-4.06410717232347,1.,-0.877244060484595));
#49268=CARTESIAN_POINT('Ctrl Pts',(-4.05790159030495,-1.,-0.872506694780563));
#49269=CARTESIAN_POINT('Ctrl Pts',(-4.05790159030495,1.,-0.872506694780563));
#49270=CARTESIAN_POINT('Ctrl Pts',(-4.05168199437128,-1.,-0.867801988858176));
#49271=CARTESIAN_POINT('Ctrl Pts',(-4.05168199437128,1.,-0.867801988858176));
#49272=CARTESIAN_POINT('Ctrl Pts',(-4.04544845048097,-1.,-0.863130256642173));
#49273=CARTESIAN_POINT('Ctrl Pts',(-4.04544845048097,1.,-0.863130256642173));
#49274=CARTESIAN_POINT('Ctrl Pts',(-4.03920099284658,-1.,-0.858491822322571));
#49275=CARTESIAN_POINT('Ctrl Pts',(-4.03920099284658,1.,-0.858491822322571));
#49276=CARTESIAN_POINT('Ctrl Pts',(-4.03293960436945,-1.,-0.853887006632178));
#49277=CARTESIAN_POINT('Ctrl Pts',(-4.03293960436945,1.,-0.853887006632178));
#49278=CARTESIAN_POINT('Ctrl Pts',(-4.02666418343508,-1.,-0.849316107475012));
#49279=CARTESIAN_POINT('Ctrl Pts',(-4.02666418343508,1.,-0.849316107475012));
#49280=CARTESIAN_POINT('Ctrl Pts',(-4.02037456798787,-1.,-0.844779403288517));
#49281=CARTESIAN_POINT('Ctrl Pts',(-4.02037456798787,1.,-0.844779403288517));
#49282=CARTESIAN_POINT('Ctrl Pts',(-4.01407059766338,-1.,-0.84027717197638));
#49283=CARTESIAN_POINT('Ctrl Pts',(-4.01407059766338,1.,-0.84027717197638));
#49284=CARTESIAN_POINT('Ctrl Pts',(-4.00775216907934,-1.,-0.835809705809821));
#49285=CARTESIAN_POINT('Ctrl Pts',(-4.00775216907934,1.,-0.835809705809821));
#49286=CARTESIAN_POINT('Ctrl Pts',(-4.00141928477447,-1.,-0.831377325741487));
#49287=CARTESIAN_POINT('Ctrl Pts',(-4.00141928477447,1.,-0.831377325741487));
#49288=CARTESIAN_POINT('Ctrl Pts',(-3.99507212784289,-1.,-0.826980400320473));
#49289=CARTESIAN_POINT('Ctrl Pts',(-3.99507212784289,1.,-0.826980400320473));
#49290=CARTESIAN_POINT('Ctrl Pts',(-3.98871104646328,-1.,-0.822619346021769));
#49291=CARTESIAN_POINT('Ctrl Pts',(-3.98871104646328,1.,-0.822619346021769));
#49292=CARTESIAN_POINT('Ctrl Pts',(-3.98233640155287,-1.,-0.818294599022033));
#49293=CARTESIAN_POINT('Ctrl Pts',(-3.98233640155287,1.,-0.818294599022033));
#49294=CARTESIAN_POINT('Ctrl Pts',(-3.97594844078763,-1.,-0.814006592328737));
#49295=CARTESIAN_POINT('Ctrl Pts',(-3.97594844078763,1.,-0.814006592328737));
#49296=CARTESIAN_POINT('Ctrl Pts',(-3.96954717513251,-1.,-0.809755732818134));
#49297=CARTESIAN_POINT('Ctrl Pts',(-3.96954717513251,1.,-0.809755732818134));
#49298=CARTESIAN_POINT('Ctrl Pts',(-3.96313222295874,-1.,-0.805542372178496));
#49299=CARTESIAN_POINT('Ctrl Pts',(-3.96313222295874,1.,-0.805542372178496));
#49300=CARTESIAN_POINT('Ctrl Pts',(-3.95670276375176,-1.,-0.801366797727206));
#49301=CARTESIAN_POINT('Ctrl Pts',(-3.95670276375176,1.,-0.801366797727206));
#49302=CARTESIAN_POINT('Ctrl Pts',(-3.95025788827189,-1.,-0.797229296085438));
#49303=CARTESIAN_POINT('Ctrl Pts',(-3.95025788827189,1.,-0.797229296085438));
#49304=CARTESIAN_POINT('Ctrl Pts',(-3.94379688971307,-1.,-0.793130205641017));
#49305=CARTESIAN_POINT('Ctrl Pts',(-3.94379688971307,1.,-0.793130205641017));
#49306=CARTESIAN_POINT('Ctrl Pts',(-3.93731956885671,-1.,-0.789069971469323));
#49307=CARTESIAN_POINT('Ctrl Pts',(-3.93731956885671,1.,-0.789069971469323));
#49308=CARTESIAN_POINT('Ctrl Pts',(-3.93082655631768,-1.,-0.785049202786458));
#49309=CARTESIAN_POINT('Ctrl Pts',(-3.93082655631768,1.,-0.785049202786458));
#49310=CARTESIAN_POINT('Ctrl Pts',(-3.92431956510418,-1.,-0.781068718228395));
#49311=CARTESIAN_POINT('Ctrl Pts',(-3.92431956510418,1.,-0.781068718228395));
#49312=CARTESIAN_POINT('Ctrl Pts',(-3.91780062334464,-1.,-0.777129415664915));
#49313=CARTESIAN_POINT('Ctrl Pts',(-3.91780062334464,1.,-0.777129415664915));
#49314=CARTESIAN_POINT('Ctrl Pts',(-3.91127138115238,-1.,-0.773232154506305));
#49315=CARTESIAN_POINT('Ctrl Pts',(-3.91127138115238,1.,-0.773232154506305));
#49316=CARTESIAN_POINT('Ctrl Pts',(-3.90473237182634,-1.,-0.769377629847876));
#49317=CARTESIAN_POINT('Ctrl Pts',(-3.90473237182634,1.,-0.769377629847876));
#49318=CARTESIAN_POINT('Ctrl Pts',(-3.89818233104381,-1.,-0.765566256401306));
#49319=CARTESIAN_POINT('Ctrl Pts',(-3.89818233104381,1.,-0.765566256401306));
#49320=CARTESIAN_POINT('Ctrl Pts',(-3.89161738162245,-1.,-0.761798028793978));
#49321=CARTESIAN_POINT('Ctrl Pts',(-3.89161738162245,1.,-0.761798028793978));
#49322=CARTESIAN_POINT('Ctrl Pts',(-3.88503262662684,-1.,-0.758072800564798));
#49323=CARTESIAN_POINT('Ctrl Pts',(-3.88503262662684,1.,-0.758072800564798));
#49324=CARTESIAN_POINT('Ctrl Pts',(-3.87842382520058,-1.,-0.754390577396846));
#49325=CARTESIAN_POINT('Ctrl Pts',(-3.87842382520058,1.,-0.754390577396846));
#49326=CARTESIAN_POINT('Ctrl Pts',(-3.87178914078372,-1.,-0.750751822383023));
#49327=CARTESIAN_POINT('Ctrl Pts',(-3.87178914078372,1.,-0.750751822383023));
#49328=CARTESIAN_POINT('Ctrl Pts',(-3.86513062969896,-1.,-0.747157716488884));
#49329=CARTESIAN_POINT('Ctrl Pts',(-3.86513062969896,1.,-0.747157716488884));
#49330=CARTESIAN_POINT('Ctrl Pts',(-3.85845645217611,-1.,-0.743610542737042));
#49331=CARTESIAN_POINT('Ctrl Pts',(-3.85845645217611,1.,-0.743610542737042));
#49332=CARTESIAN_POINT('Ctrl Pts',(-3.85177770351237,-1.,-0.740113146827176));
#49333=CARTESIAN_POINT('Ctrl Pts',(-3.85177770351237,1.,-0.740113146827176));
#49334=CARTESIAN_POINT('Ctrl Pts',(-3.84510432881231,-1.,-0.736668240497151));
#49335=CARTESIAN_POINT('Ctrl Pts',(-3.84510432881231,1.,-0.736668240497151));
#49336=CARTESIAN_POINT('Ctrl Pts',(-3.83844103658016,-1.,-0.73327770375609));
#49337=CARTESIAN_POINT('Ctrl Pts',(-3.83844103658016,1.,-0.73327770375609));
#49338=CARTESIAN_POINT('Ctrl Pts',(-3.8317839240337,-1.,-0.729942010490145));
#49339=CARTESIAN_POINT('Ctrl Pts',(-3.8317839240337,1.,-0.729942010490145));
#49340=CARTESIAN_POINT('Ctrl Pts',(-3.82511495756682,-1.,-0.726659281876608));
#49341=CARTESIAN_POINT('Ctrl Pts',(-3.82511495756682,1.,-0.726659281876608));
#49342=CARTESIAN_POINT('Ctrl Pts',(-3.81840802610795,-1.,-0.723426346019349));
#49343=CARTESIAN_POINT('Ctrl Pts',(-3.81840802610795,1.,-0.723426346019349));
#49344=CARTESIAN_POINT('Ctrl Pts',(-3.81163885127309,-1.,-0.720240466589172));
#49345=CARTESIAN_POINT('Ctrl Pts',(-3.81163885127309,1.,-0.720240466589172));
#49346=CARTESIAN_POINT('Ctrl Pts',(-3.80479445759296,-1.,-0.717100993669091));
#49347=CARTESIAN_POINT('Ctrl Pts',(-3.80479445759296,1.,-0.717100993669091));
#49348=CARTESIAN_POINT('Ctrl Pts',(-3.79788100314994,-1.,-0.714010733006677));
#49349=CARTESIAN_POINT('Ctrl Pts',(-3.79788100314994,1.,-0.714010733006677));
#49350=CARTESIAN_POINT('Ctrl Pts',(-3.79093694007146,-1.,-0.710978231689117));
#49351=CARTESIAN_POINT('Ctrl Pts',(-3.79093694007146,1.,-0.710978231689117));
#49352=CARTESIAN_POINT('Ctrl Pts',(-3.78402183336678,-1.,-0.7080158793756));
#49353=CARTESIAN_POINT('Ctrl Pts',(-3.78402183336678,1.,-0.7080158793756));
#49354=CARTESIAN_POINT('Ctrl Pts',(-3.77719254217197,-1.,-0.705135847999949));
#49355=CARTESIAN_POINT('Ctrl Pts',(-3.77719254217197,1.,-0.705135847999949));
#49356=CARTESIAN_POINT('Ctrl Pts',(-3.77048141872904,-1.,-0.702346356621613));
#49357=CARTESIAN_POINT('Ctrl Pts',(-3.77048141872904,1.,-0.702346356621613));
#49358=CARTESIAN_POINT('Ctrl Pts',(-3.76387780603725,-1.,-0.699648552230851));
#49359=CARTESIAN_POINT('Ctrl Pts',(-3.76387780603725,1.,-0.699648552230851));
#49360=CARTESIAN_POINT('Ctrl Pts',(-3.75729775766913,-1.,-0.69703124565953));
#49361=CARTESIAN_POINT('Ctrl Pts',(-3.75729775766913,1.,-0.69703124565953));
#49362=CARTESIAN_POINT('Ctrl Pts',(-3.7506028824329,-1.,-0.694474562581173));
#49363=CARTESIAN_POINT('Ctrl Pts',(-3.7506028824329,1.,-0.694474562581173));
#49364=CARTESIAN_POINT('Ctrl Pts',(-3.74365508986548,-1.,-0.691960080400503));
#49365=CARTESIAN_POINT('Ctrl Pts',(-3.74365508986548,1.,-0.691960080400503));
#49366=CARTESIAN_POINT('Ctrl Pts',(-3.73636374474993,-1.,-0.689479637354651));
#49367=CARTESIAN_POINT('Ctrl Pts',(-3.73636374474993,1.,-0.689479637354651));
#49368=CARTESIAN_POINT('Ctrl Pts',(-3.72872973554125,-1.,-0.687043475232499));
#49369=CARTESIAN_POINT('Ctrl Pts',(-3.72872973554125,1.,-0.687043475232499));
#49370=CARTESIAN_POINT('Ctrl Pts',(-3.7209063713952,-1.,-0.684691698168355));
#49371=CARTESIAN_POINT('Ctrl Pts',(-3.7209063713952,1.,-0.684691698168355));
#49372=CARTESIAN_POINT('Ctrl Pts',(-3.71319182790334,-1.,-0.682492345109689));
#49373=CARTESIAN_POINT('Ctrl Pts',(-3.71319182790334,1.,-0.682492345109689));
#49374=CARTESIAN_POINT('Ctrl Pts',(-3.70595722032165,-1.,-0.680526909711617));
#49375=CARTESIAN_POINT('Ctrl Pts',(-3.70595722032165,1.,-0.680526909711617));
#49376=CARTESIAN_POINT('Ctrl Pts',(-3.69959004073192,-1.,-0.678878822226389));
#49377=CARTESIAN_POINT('Ctrl Pts',(-3.69959004073192,1.,-0.678878822226389));
#49378=CARTESIAN_POINT('Ctrl Pts',(-3.69443683573443,-1.,-0.677621861865196));
#49379=CARTESIAN_POINT('Ctrl Pts',(-3.69443683573443,1.,-0.677621861865196));
#49380=CARTESIAN_POINT('Ctrl Pts',(-3.69073278191505,-1.,-0.67680581107414));
#49381=CARTESIAN_POINT('Ctrl Pts',(-3.69073278191505,1.,-0.67680581107414));
#49382=CARTESIAN_POINT('Ctrl Pts',(-3.68901718135636,-1.,-0.676524321060167));
#49383=CARTESIAN_POINT('Ctrl Pts',(-3.68901718135636,1.,-0.676524321060167));
#49384=CARTESIAN_POINT('Ctrl Pts',(-3.68844918120934,-1.,-0.676525601650139));
#49385=CARTESIAN_POINT('Ctrl Pts',(-3.68844918120934,1.,-0.676525601650139));
#49386=CARTESIAN_POINT('Ctrl Pts',(-3.68838970675356,-1.,-0.676620796001716));
#49387=CARTESIAN_POINT('Ctrl Pts',(-3.68838970675356,1.,-0.676620796001716));
#49388=CARTESIAN_POINT('Ctrl Pts',(-3.68843977377012,-1.,-0.676691979611562));
#49389=CARTESIAN_POINT('Ctrl Pts',(-3.68843977377012,1.,-0.676691979611562));
#49390=CARTESIAN_POINT('',(-4.10104028313088,1.,-0.906349047628866));
#49391=CARTESIAN_POINT('Ctrl Pts',(-4.10104028313088,1.,-0.906349047628866));
#49392=CARTESIAN_POINT('Ctrl Pts',(-4.09981755067956,1.,-0.905360112216302));
#49393=CARTESIAN_POINT('Ctrl Pts',(-4.09737067247114,1.,-0.903385402444212));
#49394=CARTESIAN_POINT('Ctrl Pts',(-4.09369611524319,1.,-0.900432820945975));
#49395=CARTESIAN_POINT('Ctrl Pts',(-4.08878822249095,1.,-0.896515019236368));
#49396=CARTESIAN_POINT('Ctrl Pts',(-4.08263920306651,1.,-0.891649447920401));
#49397=CARTESIAN_POINT('Ctrl Pts',(-4.07647601774639,1.,-0.886815658360739));
#49398=CARTESIAN_POINT('Ctrl Pts',(-4.07029866694292,1.,-0.882013797525916));
#49399=CARTESIAN_POINT('Ctrl Pts',(-4.06410717232347,1.,-0.877244060484595));
#49400=CARTESIAN_POINT('Ctrl Pts',(-4.05790159030495,1.,-0.872506694780563));
#49401=CARTESIAN_POINT('Ctrl Pts',(-4.05168199437128,1.,-0.867801988858176));
#49402=CARTESIAN_POINT('Ctrl Pts',(-4.04544845048097,1.,-0.863130256642173));
#49403=CARTESIAN_POINT('Ctrl Pts',(-4.03920099284658,1.,-0.858491822322571));
#49404=CARTESIAN_POINT('Ctrl Pts',(-4.03293960436945,1.,-0.853887006632178));
#49405=CARTESIAN_POINT('Ctrl Pts',(-4.02666418343508,1.,-0.849316107475012));
#49406=CARTESIAN_POINT('Ctrl Pts',(-4.02037456798787,1.,-0.844779403288517));
#49407=CARTESIAN_POINT('Ctrl Pts',(-4.01407059766338,1.,-0.84027717197638));
#49408=CARTESIAN_POINT('Ctrl Pts',(-4.00775216907934,1.,-0.835809705809821));
#49409=CARTESIAN_POINT('Ctrl Pts',(-4.00141928477447,1.,-0.831377325741487));
#49410=CARTESIAN_POINT('Ctrl Pts',(-3.99507212784289,1.,-0.826980400320473));
#49411=CARTESIAN_POINT('Ctrl Pts',(-3.98871104646328,1.,-0.822619346021769));
#49412=CARTESIAN_POINT('Ctrl Pts',(-3.98233640155287,1.,-0.818294599022033));
#49413=CARTESIAN_POINT('Ctrl Pts',(-3.97594844078763,1.,-0.814006592328737));
#49414=CARTESIAN_POINT('Ctrl Pts',(-3.96954717513251,1.,-0.809755732818134));
#49415=CARTESIAN_POINT('Ctrl Pts',(-3.96313222295874,1.,-0.805542372178496));
#49416=CARTESIAN_POINT('Ctrl Pts',(-3.95670276375176,1.,-0.801366797727206));
#49417=CARTESIAN_POINT('Ctrl Pts',(-3.95025788827189,1.,-0.797229296085438));
#49418=CARTESIAN_POINT('Ctrl Pts',(-3.94379688971307,1.,-0.793130205641017));
#49419=CARTESIAN_POINT('Ctrl Pts',(-3.93731956885671,1.,-0.789069971469323));
#49420=CARTESIAN_POINT('Ctrl Pts',(-3.93082655631768,1.,-0.785049202786458));
#49421=CARTESIAN_POINT('Ctrl Pts',(-3.92431956510418,1.,-0.781068718228395));
#49422=CARTESIAN_POINT('Ctrl Pts',(-3.91780062334464,1.,-0.777129415664915));
#49423=CARTESIAN_POINT('Ctrl Pts',(-3.91127138115238,1.,-0.773232154506305));
#49424=CARTESIAN_POINT('Ctrl Pts',(-3.90473237182634,1.,-0.769377629847876));
#49425=CARTESIAN_POINT('Ctrl Pts',(-3.89818233104381,1.,-0.765566256401306));
#49426=CARTESIAN_POINT('Ctrl Pts',(-3.89161738162245,1.,-0.761798028793978));
#49427=CARTESIAN_POINT('Ctrl Pts',(-3.88503262662684,1.,-0.758072800564798));
#49428=CARTESIAN_POINT('Ctrl Pts',(-3.87842382520058,1.,-0.754390577396846));
#49429=CARTESIAN_POINT('Ctrl Pts',(-3.87178914078372,1.,-0.750751822383023));
#49430=CARTESIAN_POINT('Ctrl Pts',(-3.86513062969896,1.,-0.747157716488884));
#49431=CARTESIAN_POINT('Ctrl Pts',(-3.85845645217611,1.,-0.743610542737042));
#49432=CARTESIAN_POINT('Ctrl Pts',(-3.85177770351237,1.,-0.740113146827176));
#49433=CARTESIAN_POINT('Ctrl Pts',(-3.84510432881231,1.,-0.736668240497151));
#49434=CARTESIAN_POINT('Ctrl Pts',(-3.83844103658016,1.,-0.73327770375609));
#49435=CARTESIAN_POINT('Ctrl Pts',(-3.8317839240337,1.,-0.729942010490145));
#49436=CARTESIAN_POINT('Ctrl Pts',(-3.82511495756682,1.,-0.726659281876608));
#49437=CARTESIAN_POINT('Ctrl Pts',(-3.81840802610795,1.,-0.723426346019349));
#49438=CARTESIAN_POINT('Ctrl Pts',(-3.81163885127309,1.,-0.720240466589172));
#49439=CARTESIAN_POINT('Ctrl Pts',(-3.80479445759296,1.,-0.717100993669091));
#49440=CARTESIAN_POINT('Ctrl Pts',(-3.79788100314994,1.,-0.714010733006677));
#49441=CARTESIAN_POINT('Ctrl Pts',(-3.79093694007146,1.,-0.710978231689117));
#49442=CARTESIAN_POINT('Ctrl Pts',(-3.78402183336678,1.,-0.7080158793756));
#49443=CARTESIAN_POINT('Ctrl Pts',(-3.77719254217197,1.,-0.705135847999949));
#49444=CARTESIAN_POINT('Ctrl Pts',(-3.77048141872904,1.,-0.702346356621613));
#49445=CARTESIAN_POINT('Ctrl Pts',(-3.76387780603725,1.,-0.699648552230851));
#49446=CARTESIAN_POINT('Ctrl Pts',(-3.75729775766913,1.,-0.69703124565953));
#49447=CARTESIAN_POINT('Ctrl Pts',(-3.7506028824329,1.,-0.694474562581173));
#49448=CARTESIAN_POINT('Ctrl Pts',(-3.74365508986548,1.,-0.691960080400503));
#49449=CARTESIAN_POINT('Ctrl Pts',(-3.73636374474993,1.,-0.689479637354651));
#49450=CARTESIAN_POINT('Ctrl Pts',(-3.72872973554125,1.,-0.687043475232499));
#49451=CARTESIAN_POINT('Ctrl Pts',(-3.7209063713952,1.,-0.684691698168355));
#49452=CARTESIAN_POINT('Ctrl Pts',(-3.71319182790334,1.,-0.682492345109689));
#49453=CARTESIAN_POINT('Ctrl Pts',(-3.70595722032165,1.,-0.680526909711617));
#49454=CARTESIAN_POINT('Ctrl Pts',(-3.69959004073192,1.,-0.678878822226389));
#49455=CARTESIAN_POINT('Ctrl Pts',(-3.69443683573443,1.,-0.677621861865196));
#49456=CARTESIAN_POINT('Ctrl Pts',(-3.6910107117555,1.,-0.676867042599711));
#49457=CARTESIAN_POINT('Ctrl Pts',(-3.68934997767391,1.,-0.676580391119535));
#49458=CARTESIAN_POINT('Ctrl Pts',(-3.68869596426099,1.,-0.676535079520365));
#49459=CARTESIAN_POINT('Ctrl Pts',(-3.68850172300543,1.,-0.67656928609342));
#49460=CARTESIAN_POINT('Ctrl Pts',(-3.68845817949618,1.,-0.676591647973661));
#49461=CARTESIAN_POINT('',(-4.10104028313088,0.,-0.906349047628866));
#49462=CARTESIAN_POINT('Ctrl Pts',(-3.59363563249864,-1.,-1.07157964745328));
#49463=CARTESIAN_POINT('Ctrl Pts',(-3.59363563249864,1.,-1.07157964745328));
#49464=CARTESIAN_POINT('Ctrl Pts',(-3.59355870577901,-1.,-1.07162034256459));
#49465=CARTESIAN_POINT('Ctrl Pts',(-3.59355870577901,1.,-1.07162034256459));
#49466=CARTESIAN_POINT('Ctrl Pts',(-3.59356848057812,-1.,-1.07173216219145));
#49467=CARTESIAN_POINT('Ctrl Pts',(-3.59356848057812,1.,-1.07173216219145));
#49468=CARTESIAN_POINT('Ctrl Pts',(-3.5940739910409,-1.,-1.07199116987656));
#49469=CARTESIAN_POINT('Ctrl Pts',(-3.5940739910409,1.,-1.07199116987656));
#49470=CARTESIAN_POINT('Ctrl Pts',(-3.59573039612316,-1.,-1.07251922679245));
#49471=CARTESIAN_POINT('Ctrl Pts',(-3.59573039612316,1.,-1.07251922679245));
#49472=CARTESIAN_POINT('Ctrl Pts',(-3.59940121154535,-1.,-1.07347372545714));
#49473=CARTESIAN_POINT('Ctrl Pts',(-3.59940121154535,1.,-1.07347372545714));
#49474=CARTESIAN_POINT('Ctrl Pts',(-3.60456339887778,-1.,-1.07469327168578));
#49475=CARTESIAN_POINT('Ctrl Pts',(-3.60456339887778,1.,-1.07469327168578));
#49476=CARTESIAN_POINT('Ctrl Pts',(-3.61098481349204,-1.,-1.07611545402734));
#49477=CARTESIAN_POINT('Ctrl Pts',(-3.61098481349204,1.,-1.07611545402734));
#49478=CARTESIAN_POINT('Ctrl Pts',(-3.61832318504574,-1.,-1.07764868137619));
#49479=CARTESIAN_POINT('Ctrl Pts',(-3.61832318504574,1.,-1.07764868137619));
#49480=CARTESIAN_POINT('Ctrl Pts',(-3.62619537902361,-1.,-1.07919137290742));
#49481=CARTESIAN_POINT('Ctrl Pts',(-3.62619537902361,1.,-1.07919137290742));
#49482=CARTESIAN_POINT('Ctrl Pts',(-3.63423373196529,-1.,-1.08064765719867));
#49483=CARTESIAN_POINT('Ctrl Pts',(-3.63423373196529,1.,-1.08064765719867));
#49484=CARTESIAN_POINT('Ctrl Pts',(-3.64214167843677,-1.,-1.08194278850996));
#49485=CARTESIAN_POINT('Ctrl Pts',(-3.64214167843677,1.,-1.08194278850996));
#49486=CARTESIAN_POINT('Ctrl Pts',(-3.64976441208358,-1.,-1.08304289898623));
#49487=CARTESIAN_POINT('Ctrl Pts',(-3.64976441208358,1.,-1.08304289898623));
#49488=CARTESIAN_POINT('Ctrl Pts',(-3.65709649161166,-1.,-1.08395671077807));
#49489=CARTESIAN_POINT('Ctrl Pts',(-3.65709649161166,1.,-1.08395671077807));
#49490=CARTESIAN_POINT('Ctrl Pts',(-3.66422237895365,-1.,-1.08471809922901));
#49491=CARTESIAN_POINT('Ctrl Pts',(-3.66422237895365,1.,-1.08471809922901));
#49492=CARTESIAN_POINT('Ctrl Pts',(-3.67127347729666,-1.,-1.0853733414449));
#49493=CARTESIAN_POINT('Ctrl Pts',(-3.67127347729666,1.,-1.0853733414449));
#49494=CARTESIAN_POINT('Ctrl Pts',(-3.67838211685117,-1.,-1.0859675575576));
#49495=CARTESIAN_POINT('Ctrl Pts',(-3.67838211685117,1.,-1.0859675575576));
#49496=CARTESIAN_POINT('Ctrl Pts',(-3.68562817420797,-1.,-1.0865288888259));
#49497=CARTESIAN_POINT('Ctrl Pts',(-3.68562817420797,1.,-1.0865288888259));
#49498=CARTESIAN_POINT('Ctrl Pts',(-3.69302062410157,-1.,-1.08706319540271));
#49499=CARTESIAN_POINT('Ctrl Pts',(-3.69302062410157,1.,-1.08706319540271));
#49500=CARTESIAN_POINT('Ctrl Pts',(-3.70052690909833,-1.,-1.08756311291309));
#49501=CARTESIAN_POINT('Ctrl Pts',(-3.70052690909833,1.,-1.08756311291309));
#49502=CARTESIAN_POINT('Ctrl Pts',(-3.70809084139457,-1.,-1.08801367312185));
#49503=CARTESIAN_POINT('Ctrl Pts',(-3.70809084139457,1.,-1.08801367312185));
#49504=CARTESIAN_POINT('Ctrl Pts',(-3.71565372339075,-1.,-1.0883988733478));
#49505=CARTESIAN_POINT('Ctrl Pts',(-3.71565372339075,1.,-1.0883988733478));
#49506=CARTESIAN_POINT('Ctrl Pts',(-3.72317741369398,-1.,-1.08870887220082));
#49507=CARTESIAN_POINT('Ctrl Pts',(-3.72317741369398,1.,-1.08870887220082));
#49508=CARTESIAN_POINT('Ctrl Pts',(-3.73065515162988,-1.,-1.08894337390937));
#49509=CARTESIAN_POINT('Ctrl Pts',(-3.73065515162988,1.,-1.08894337390937));
#49510=CARTESIAN_POINT('Ctrl Pts',(-3.73809879348239,-1.,-1.08910769013297));
#49511=CARTESIAN_POINT('Ctrl Pts',(-3.73809879348239,1.,-1.08910769013297));
#49512=CARTESIAN_POINT('Ctrl Pts',(-3.74553121371757,-1.,-1.08921040494017));
#49513=CARTESIAN_POINT('Ctrl Pts',(-3.74553121371757,1.,-1.08921040494017));
#49514=CARTESIAN_POINT('Ctrl Pts',(-3.75297711748132,-1.,-1.08926054632925));
#49515=CARTESIAN_POINT('Ctrl Pts',(-3.75297711748132,1.,-1.08926054632925));
#49516=CARTESIAN_POINT('Ctrl Pts',(-3.76045342580208,-1.,-1.08926462734281));
#49517=CARTESIAN_POINT('Ctrl Pts',(-3.76045342580208,1.,-1.08926462734281));
#49518=CARTESIAN_POINT('Ctrl Pts',(-3.76796340094448,-1.,-1.08922484204256));
#49519=CARTESIAN_POINT('Ctrl Pts',(-3.76796340094448,1.,-1.08922484204256));
#49520=CARTESIAN_POINT('Ctrl Pts',(-3.77550199409424,-1.,-1.0891407279127));
#49521=CARTESIAN_POINT('Ctrl Pts',(-3.77550199409424,1.,-1.0891407279127));
#49522=CARTESIAN_POINT('Ctrl Pts',(-3.78305911299504,-1.,-1.08901018614636));
#49523=CARTESIAN_POINT('Ctrl Pts',(-3.78305911299504,1.,-1.08901018614636));
#49524=CARTESIAN_POINT('Ctrl Pts',(-3.79062357974404,-1.,-1.08883071512098));
#49525=CARTESIAN_POINT('Ctrl Pts',(-3.79062357974404,1.,-1.08883071512098));
#49526=CARTESIAN_POINT('Ctrl Pts',(-3.79818708705259,-1.,-1.08860064435778));
#49527=CARTESIAN_POINT('Ctrl Pts',(-3.79818708705259,1.,-1.08860064435778));
#49528=CARTESIAN_POINT('Ctrl Pts',(-3.8057472665766,-1.,-1.0883200925538));
#49529=CARTESIAN_POINT('Ctrl Pts',(-3.8057472665766,1.,-1.0883200925538));
#49530=CARTESIAN_POINT('Ctrl Pts',(-3.81330554446323,-1.,-1.08799030610862));
#49531=CARTESIAN_POINT('Ctrl Pts',(-3.81330554446323,1.,-1.08799030610862));
#49532=CARTESIAN_POINT('Ctrl Pts',(-3.82086569676319,-1.,-1.08761321539442));
#49533=CARTESIAN_POINT('Ctrl Pts',(-3.82086569676319,1.,-1.08761321539442));
#49534=CARTESIAN_POINT('Ctrl Pts',(-3.82843215316984,-1.,-1.08719091307558));
#49535=CARTESIAN_POINT('Ctrl Pts',(-3.82843215316984,1.,-1.08719091307558));
#49536=CARTESIAN_POINT('Ctrl Pts',(-3.83600837071708,-1.,-1.08672515456902));
#49537=CARTESIAN_POINT('Ctrl Pts',(-3.83600837071708,1.,-1.08672515456902));
#49538=CARTESIAN_POINT('Ctrl Pts',(-3.8435952876495,-1.,-1.08621688337604));
#49539=CARTESIAN_POINT('Ctrl Pts',(-3.8435952876495,1.,-1.08621688337604));
#49540=CARTESIAN_POINT('Ctrl Pts',(-3.85119211322755,-1.,-1.08566647671844));
#49541=CARTESIAN_POINT('Ctrl Pts',(-3.85119211322755,1.,-1.08566647671844));
#49542=CARTESIAN_POINT('Ctrl Pts',(-3.85879698702532,-1.,-1.08507395120059));
#49543=CARTESIAN_POINT('Ctrl Pts',(-3.85879698702532,1.,-1.08507395120059));
#49544=CARTESIAN_POINT('Ctrl Pts',(-3.86640769434274,-1.,-1.08443918607927));
#49545=CARTESIAN_POINT('Ctrl Pts',(-3.86640769434274,1.,-1.08443918607927));
#49546=CARTESIAN_POINT('Ctrl Pts',(-3.8740223372254,-1.,-1.08376213307504));
#49547=CARTESIAN_POINT('Ctrl Pts',(-3.8740223372254,1.,-1.08376213307504));
#49548=CARTESIAN_POINT('Ctrl Pts',(-3.88164007721312,-1.,-1.08304304871028));
#49549=CARTESIAN_POINT('Ctrl Pts',(-3.88164007721312,1.,-1.08304304871028));
#49550=CARTESIAN_POINT('Ctrl Pts',(-3.88926088975114,-1.,-1.08228241999346));
#49551=CARTESIAN_POINT('Ctrl Pts',(-3.88926088975114,1.,-1.08228241999346));
#49552=CARTESIAN_POINT('Ctrl Pts',(-3.8968852509835,-1.,-1.08148086931358));
#49553=CARTESIAN_POINT('Ctrl Pts',(-3.8968852509835,1.,-1.08148086931358));
#49554=CARTESIAN_POINT('Ctrl Pts',(-3.90451384092545,-1.,-1.08063906483818));
#49555=CARTESIAN_POINT('Ctrl Pts',(-3.90451384092545,1.,-1.08063906483818));
#49556=CARTESIAN_POINT('Ctrl Pts',(-3.91214726022143,-1.,-1.07975763507473));
#49557=CARTESIAN_POINT('Ctrl Pts',(-3.91214726022143,1.,-1.07975763507473));
#49558=CARTESIAN_POINT('Ctrl Pts',(-3.91978568924178,-1.,-1.07883706663554));
#49559=CARTESIAN_POINT('Ctrl Pts',(-3.91978568924178,1.,-1.07883706663554));
#49560=CARTESIAN_POINT('Ctrl Pts',(-3.9274289334984,-1.,-1.07787771707195));
#49561=CARTESIAN_POINT('Ctrl Pts',(-3.9274289334984,1.,-1.07787771707195));
#49562=CARTESIAN_POINT('Ctrl Pts',(-3.93507657572883,-1.,-1.07687985975384));
#49563=CARTESIAN_POINT('Ctrl Pts',(-3.93507657572883,1.,-1.07687985975384));
#49564=CARTESIAN_POINT('Ctrl Pts',(-3.94272809633331,-1.,-1.07584371946443));
#49565=CARTESIAN_POINT('Ctrl Pts',(-3.94272809633331,1.,-1.07584371946443));
#49566=CARTESIAN_POINT('Ctrl Pts',(-3.95038299600676,-1.,-1.07476950921587));
#49567=CARTESIAN_POINT('Ctrl Pts',(-3.95038299600676,1.,-1.07476950921587));
#49568=CARTESIAN_POINT('Ctrl Pts',(-3.95804094429373,-1.,-1.07365747426491));
#49569=CARTESIAN_POINT('Ctrl Pts',(-3.95804094429373,1.,-1.07365747426491));
#49570=CARTESIAN_POINT('Ctrl Pts',(-3.96570179322338,-1.,-1.07250789943007));
#49571=CARTESIAN_POINT('Ctrl Pts',(-3.96570179322338,1.,-1.07250789943007));
#49572=CARTESIAN_POINT('Ctrl Pts',(-3.9733655022223,-1.,-1.07132109206164));
#49573=CARTESIAN_POINT('Ctrl Pts',(-3.9733655022223,1.,-1.07132109206164));
#49574=CARTESIAN_POINT('Ctrl Pts',(-3.98103208801101,-1.,-1.07009737257767));
#49575=CARTESIAN_POINT('Ctrl Pts',(-3.98103208801101,1.,-1.07009737257767));
#49576=CARTESIAN_POINT('Ctrl Pts',(-3.98870156857412,-1.,-1.06883706263941));
#49577=CARTESIAN_POINT('Ctrl Pts',(-3.98870156857412,1.,-1.06883706263941));
#49578=CARTESIAN_POINT('Ctrl Pts',(-3.99637389920441,-1.,-1.06754047381312));
#49579=CARTESIAN_POINT('Ctrl Pts',(-3.99637389920441,1.,-1.06754047381312));
#49580=CARTESIAN_POINT('Ctrl Pts',(-4.00404894952579,-1.,-1.06620789963606));
#49581=CARTESIAN_POINT('Ctrl Pts',(-4.00404894952579,1.,-1.06620789963606));
#49582=CARTESIAN_POINT('Ctrl Pts',(-4.01172654187398,-1.,-1.06483961343109));
#49583=CARTESIAN_POINT('Ctrl Pts',(-4.01172654187398,1.,-1.06483961343109));
#49584=CARTESIAN_POINT('Ctrl Pts',(-4.01940647495943,-1.,-1.06343586496236));
#49585=CARTESIAN_POINT('Ctrl Pts',(-4.01940647495943,1.,-1.06343586496236));
#49586=CARTESIAN_POINT('Ctrl Pts',(-4.02708855235633,-1.,-1.06199687787462));
#49587=CARTESIAN_POINT('Ctrl Pts',(-4.02708855235633,1.,-1.06199687787462));
#49588=CARTESIAN_POINT('Ctrl Pts',(-4.03477261141553,-1.,-1.06052284711857));
#49589=CARTESIAN_POINT('Ctrl Pts',(-4.03477261141553,1.,-1.06052284711857));
#49590=CARTESIAN_POINT('Ctrl Pts',(-4.04245854427496,-1.,-1.05901393666566));
#49591=CARTESIAN_POINT('Ctrl Pts',(-4.04245854427496,1.,-1.05901393666566));
#49592=CARTESIAN_POINT('Ctrl Pts',(-4.05014628384869,-1.,-1.05747027727959));
#49593=CARTESIAN_POINT('Ctrl Pts',(-4.05014628384869,1.,-1.05747027727959));
#49594=CARTESIAN_POINT('Ctrl Pts',(-4.05629789307025,-1.,-1.05620762707996));
#49595=CARTESIAN_POINT('Ctrl Pts',(-4.05629789307025,1.,-1.05620762707996));
#49596=CARTESIAN_POINT('Ctrl Pts',(-4.06091239149123,-1.,-1.05524507177599));
#49597=CARTESIAN_POINT('Ctrl Pts',(-4.06091239149123,1.,-1.05524507177599));
#49598=CARTESIAN_POINT('Ctrl Pts',(-4.06398907542249,-1.,-1.05459645194823));
#49599=CARTESIAN_POINT('Ctrl Pts',(-4.06398907542249,1.,-1.05459645194823));
#49600=CARTESIAN_POINT('Ctrl Pts',(-4.06552750530042,-1.,-1.05427041296137));
#49601=CARTESIAN_POINT('Ctrl Pts',(-4.06552750530042,1.,-1.05427041296137));
#49602=CARTESIAN_POINT('',(-3.59360648251073,1.,-1.07167739962028));
#49603=CARTESIAN_POINT('Ctrl Pts',(-3.59360648251073,-1.,-1.07167739962028));
#49604=CARTESIAN_POINT('Ctrl Pts',(-3.59360648251073,-0.666666666666667,
-1.07167739962028));
#49605=CARTESIAN_POINT('Ctrl Pts',(-3.59360648251073,-0.333333333333333,
-1.07167739962028));
#49606=CARTESIAN_POINT('Ctrl Pts',(-3.59360648251073,0.333333333333333,
-1.07167739962028));
#49607=CARTESIAN_POINT('Ctrl Pts',(-3.59360648251073,0.666666666666667,
-1.07167739962028));
#49608=CARTESIAN_POINT('Ctrl Pts',(-3.59360648251073,1.,-1.07167739962028));
#49609=CARTESIAN_POINT('',(-4.06552750530042,1.,-1.05427041296137));
#49610=CARTESIAN_POINT('',(-4.06552750530042,0.,-1.05427041296137));
#49611=CARTESIAN_POINT('Ctrl Pts',(-3.59360648251073,1.,-1.07167739962028));
#49612=CARTESIAN_POINT('Ctrl Pts',(-3.5936351279798,1.,-1.07171709254135));
#49613=CARTESIAN_POINT('Ctrl Pts',(-3.59379266874567,1.,-1.07183575450617));
#49614=CARTESIAN_POINT('Ctrl Pts',(-3.59439596999862,1.,-1.07209229745229));
#49615=CARTESIAN_POINT('Ctrl Pts',(-3.59600583194946,1.,-1.07259084660936));
#49616=CARTESIAN_POINT('Ctrl Pts',(-3.59940121154535,1.,-1.07347372545714));
#49617=CARTESIAN_POINT('Ctrl Pts',(-3.60456339887778,1.,-1.07469327168578));
#49618=CARTESIAN_POINT('Ctrl Pts',(-3.61098481349204,1.,-1.07611545402734));
#49619=CARTESIAN_POINT('Ctrl Pts',(-3.61832318504574,1.,-1.07764868137619));
#49620=CARTESIAN_POINT('Ctrl Pts',(-3.62619537902361,1.,-1.07919137290742));
#49621=CARTESIAN_POINT('Ctrl Pts',(-3.63423373196529,1.,-1.08064765719867));
#49622=CARTESIAN_POINT('Ctrl Pts',(-3.64214167843677,1.,-1.08194278850996));
#49623=CARTESIAN_POINT('Ctrl Pts',(-3.64976441208358,1.,-1.08304289898623));
#49624=CARTESIAN_POINT('Ctrl Pts',(-3.65709649161166,1.,-1.08395671077807));
#49625=CARTESIAN_POINT('Ctrl Pts',(-3.66422237895365,1.,-1.08471809922901));
#49626=CARTESIAN_POINT('Ctrl Pts',(-3.67127347729666,1.,-1.0853733414449));
#49627=CARTESIAN_POINT('Ctrl Pts',(-3.67838211685117,1.,-1.0859675575576));
#49628=CARTESIAN_POINT('Ctrl Pts',(-3.68562817420797,1.,-1.0865288888259));
#49629=CARTESIAN_POINT('Ctrl Pts',(-3.69302062410157,1.,-1.08706319540271));
#49630=CARTESIAN_POINT('Ctrl Pts',(-3.70052690909833,1.,-1.08756311291309));
#49631=CARTESIAN_POINT('Ctrl Pts',(-3.70809084139457,1.,-1.08801367312185));
#49632=CARTESIAN_POINT('Ctrl Pts',(-3.71565372339075,1.,-1.0883988733478));
#49633=CARTESIAN_POINT('Ctrl Pts',(-3.72317741369398,1.,-1.08870887220082));
#49634=CARTESIAN_POINT('Ctrl Pts',(-3.73065515162988,1.,-1.08894337390937));
#49635=CARTESIAN_POINT('Ctrl Pts',(-3.73809879348239,1.,-1.08910769013297));
#49636=CARTESIAN_POINT('Ctrl Pts',(-3.74553121371757,1.,-1.08921040494017));
#49637=CARTESIAN_POINT('Ctrl Pts',(-3.75297711748132,1.,-1.08926054632925));
#49638=CARTESIAN_POINT('Ctrl Pts',(-3.76045342580208,1.,-1.08926462734281));
#49639=CARTESIAN_POINT('Ctrl Pts',(-3.76796340094448,1.,-1.08922484204256));
#49640=CARTESIAN_POINT('Ctrl Pts',(-3.77550199409424,1.,-1.0891407279127));
#49641=CARTESIAN_POINT('Ctrl Pts',(-3.78305911299504,1.,-1.08901018614636));
#49642=CARTESIAN_POINT('Ctrl Pts',(-3.79062357974404,1.,-1.08883071512098));
#49643=CARTESIAN_POINT('Ctrl Pts',(-3.79818708705259,1.,-1.08860064435778));
#49644=CARTESIAN_POINT('Ctrl Pts',(-3.8057472665766,1.,-1.0883200925538));
#49645=CARTESIAN_POINT('Ctrl Pts',(-3.81330554446323,1.,-1.08799030610862));
#49646=CARTESIAN_POINT('Ctrl Pts',(-3.82086569676319,1.,-1.08761321539442));
#49647=CARTESIAN_POINT('Ctrl Pts',(-3.82843215316984,1.,-1.08719091307558));
#49648=CARTESIAN_POINT('Ctrl Pts',(-3.83600837071708,1.,-1.08672515456902));
#49649=CARTESIAN_POINT('Ctrl Pts',(-3.8435952876495,1.,-1.08621688337604));
#49650=CARTESIAN_POINT('Ctrl Pts',(-3.85119211322755,1.,-1.08566647671844));
#49651=CARTESIAN_POINT('Ctrl Pts',(-3.85879698702532,1.,-1.08507395120059));
#49652=CARTESIAN_POINT('Ctrl Pts',(-3.86640769434274,1.,-1.08443918607927));
#49653=CARTESIAN_POINT('Ctrl Pts',(-3.8740223372254,1.,-1.08376213307504));
#49654=CARTESIAN_POINT('Ctrl Pts',(-3.88164007721312,1.,-1.08304304871028));
#49655=CARTESIAN_POINT('Ctrl Pts',(-3.88926088975114,1.,-1.08228241999346));
#49656=CARTESIAN_POINT('Ctrl Pts',(-3.8968852509835,1.,-1.08148086931358));
#49657=CARTESIAN_POINT('Ctrl Pts',(-3.90451384092545,1.,-1.08063906483818));
#49658=CARTESIAN_POINT('Ctrl Pts',(-3.91214726022143,1.,-1.07975763507473));
#49659=CARTESIAN_POINT('Ctrl Pts',(-3.91978568924178,1.,-1.07883706663554));
#49660=CARTESIAN_POINT('Ctrl Pts',(-3.9274289334984,1.,-1.07787771707195));
#49661=CARTESIAN_POINT('Ctrl Pts',(-3.93507657572883,1.,-1.07687985975384));
#49662=CARTESIAN_POINT('Ctrl Pts',(-3.94272809633331,1.,-1.07584371946443));
#49663=CARTESIAN_POINT('Ctrl Pts',(-3.95038299600676,1.,-1.07476950921587));
#49664=CARTESIAN_POINT('Ctrl Pts',(-3.95804094429373,1.,-1.07365747426491));
#49665=CARTESIAN_POINT('Ctrl Pts',(-3.96570179322338,1.,-1.07250789943007));
#49666=CARTESIAN_POINT('Ctrl Pts',(-3.9733655022223,1.,-1.07132109206164));
#49667=CARTESIAN_POINT('Ctrl Pts',(-3.98103208801101,1.,-1.07009737257767));
#49668=CARTESIAN_POINT('Ctrl Pts',(-3.98870156857412,1.,-1.06883706263941));
#49669=CARTESIAN_POINT('Ctrl Pts',(-3.99637389920441,1.,-1.06754047381312));
#49670=CARTESIAN_POINT('Ctrl Pts',(-4.00404894952579,1.,-1.06620789963606));
#49671=CARTESIAN_POINT('Ctrl Pts',(-4.01172654187398,1.,-1.06483961343109));
#49672=CARTESIAN_POINT('Ctrl Pts',(-4.01940647495943,1.,-1.06343586496236));
#49673=CARTESIAN_POINT('Ctrl Pts',(-4.02708855235633,1.,-1.06199687787462));
#49674=CARTESIAN_POINT('Ctrl Pts',(-4.03477261141553,1.,-1.06052284711857));
#49675=CARTESIAN_POINT('Ctrl Pts',(-4.04245854427496,1.,-1.05901393666566));
#49676=CARTESIAN_POINT('Ctrl Pts',(-4.05014628384869,1.,-1.05747027727959));
#49677=CARTESIAN_POINT('Ctrl Pts',(-4.05629789307025,1.,-1.05620762707996));
#49678=CARTESIAN_POINT('Ctrl Pts',(-4.06091239149123,1.,-1.05524507177599));
#49679=CARTESIAN_POINT('Ctrl Pts',(-4.06398907542249,1.,-1.05459645194823));
#49680=CARTESIAN_POINT('Ctrl Pts',(-4.06552750530042,1.,-1.05427041296137));
#49681=CARTESIAN_POINT('Origin',(-4.06552750530042,0.,-1.05427041296137));
#49682=CARTESIAN_POINT('',(-4.10104028313088,1.,-0.906349047628866));
#49683=CARTESIAN_POINT('Origin',(0.,0.,0.));
#49684=CARTESIAN_POINT('',(-3.5372048861597,1.,-1.24526366418038));
#49685=CARTESIAN_POINT('Origin',(0.,1.,0.));
#49686=CARTESIAN_POINT('Ctrl Pts',(-3.5372048861597,1.,-1.24526366418038));
#49687=CARTESIAN_POINT('Ctrl Pts',(-3.5372048861597,0.666666666666667,-1.24526366418038));
#49688=CARTESIAN_POINT('Ctrl Pts',(-3.5372048861597,0.333333333333333,-1.24526366418038));
#49689=CARTESIAN_POINT('Ctrl Pts',(-3.5372048861597,-0.333333333333333,
-1.24526366418038));
#49690=CARTESIAN_POINT('Ctrl Pts',(-3.5372048861597,-0.666666666666667,
-1.24526366418038));
#49691=CARTESIAN_POINT('Ctrl Pts',(-3.5372048861597,-1.,-1.24526366418038));
#49692=CARTESIAN_POINT('Ctrl Pts',(-3.90876544355381,-1.,-1.53673442965256));
#49693=CARTESIAN_POINT('Ctrl Pts',(-3.90876544355381,1.,-1.53673442965256));
#49694=CARTESIAN_POINT('Ctrl Pts',(-3.90771246855019,-1.,-1.53556639217905));
#49695=CARTESIAN_POINT('Ctrl Pts',(-3.90771246855019,1.,-1.53556639217905));
#49696=CARTESIAN_POINT('Ctrl Pts',(-3.90560462813969,-1.,-1.53323321827755));
#49697=CARTESIAN_POINT('Ctrl Pts',(-3.90560462813969,1.,-1.53323321827755));
#49698=CARTESIAN_POINT('Ctrl Pts',(-3.90243719631596,-1.,-1.52974216056287));
#49699=CARTESIAN_POINT('Ctrl Pts',(-3.90243719631596,1.,-1.52974216056287));
#49700=CARTESIAN_POINT('Ctrl Pts',(-3.89820260708225,-1.,-1.52510482991635));
#49701=CARTESIAN_POINT('Ctrl Pts',(-3.89820260708225,1.,-1.52510482991635));
#49702=CARTESIAN_POINT('Ctrl Pts',(-3.89289043533657,-1.,-1.51933724329305));
#49703=CARTESIAN_POINT('Ctrl Pts',(-3.89289043533657,1.,-1.51933724329305));
#49704=CARTESIAN_POINT('Ctrl Pts',(-3.88755930033884,-1.,-1.51359883110559));
#49705=CARTESIAN_POINT('Ctrl Pts',(-3.88755930033884,1.,-1.51359883110559));
#49706=CARTESIAN_POINT('Ctrl Pts',(-3.88220917950538,-1.,-1.50788973857757));
#49707=CARTESIAN_POINT('Ctrl Pts',(-3.88220917950538,1.,-1.50788973857757));
#49708=CARTESIAN_POINT('Ctrl Pts',(-3.87684006372134,-1.,-1.50221016176556));
#49709=CARTESIAN_POINT('Ctrl Pts',(-3.87684006372134,1.,-1.50221016176556));
#49710=CARTESIAN_POINT('Ctrl Pts',(-3.87145196998465,-1.,-1.49656035399122));
#49711=CARTESIAN_POINT('Ctrl Pts',(-3.87145196998465,1.,-1.49656035399122));
#49712=CARTESIAN_POINT('Ctrl Pts',(-3.86604492575189,-1.,-1.4909406116431));
#49713=CARTESIAN_POINT('Ctrl Pts',(-3.86604492575189,1.,-1.4909406116431));
#49714=CARTESIAN_POINT('Ctrl Pts',(-3.86061894706087,-1.,-1.48535125509919));
#49715=CARTESIAN_POINT('Ctrl Pts',(-3.86061894706087,1.,-1.48535125509919));
#49716=CARTESIAN_POINT('Ctrl Pts',(-3.85517401698843,-1.,-1.4797926099102));
#49717=CARTESIAN_POINT('Ctrl Pts',(-3.85517401698843,1.,-1.4797926099102));
#49718=CARTESIAN_POINT('Ctrl Pts',(-3.84971006847277,-1.,-1.47426499018538));
#49719=CARTESIAN_POINT('Ctrl Pts',(-3.84971006847277,1.,-1.47426499018538));
#49720=CARTESIAN_POINT('Ctrl Pts',(-3.84422695454796,-1.,-1.46876867426504));
#49721=CARTESIAN_POINT('Ctrl Pts',(-3.84422695454796,1.,-1.46876867426504));
#49722=CARTESIAN_POINT('Ctrl Pts',(-3.83872447159639,-1.,-1.46330391180752));
#49723=CARTESIAN_POINT('Ctrl Pts',(-3.83872447159639,1.,-1.46330391180752));
#49724=CARTESIAN_POINT('Ctrl Pts',(-3.83320241775423,-1.,-1.45787095220852));
#49725=CARTESIAN_POINT('Ctrl Pts',(-3.83320241775423,1.,-1.45787095220852));
#49726=CARTESIAN_POINT('Ctrl Pts',(-3.82766064519074,-1.,-1.45247006796836));
#49727=CARTESIAN_POINT('Ctrl Pts',(-3.82766064519074,1.,-1.45247006796836));
#49728=CARTESIAN_POINT('Ctrl Pts',(-3.82209910620533,-1.,-1.44710157648539));
#49729=CARTESIAN_POINT('Ctrl Pts',(-3.82209910620533,1.,-1.44710157648539));
#49730=CARTESIAN_POINT('Ctrl Pts',(-3.81651792398414,-1.,-1.44176587041347));
#49731=CARTESIAN_POINT('Ctrl Pts',(-3.81651792398414,1.,-1.44176587041347));
#49732=CARTESIAN_POINT('Ctrl Pts',(-3.81091737726815,-1.,-1.43646341556724));
#49733=CARTESIAN_POINT('Ctrl Pts',(-3.81091737726815,1.,-1.43646341556724));
#49734=CARTESIAN_POINT('Ctrl Pts',(-3.80529775429805,-1.,-1.4311946992132));
#49735=CARTESIAN_POINT('Ctrl Pts',(-3.80529775429805,1.,-1.4311946992132));
#49736=CARTESIAN_POINT('Ctrl Pts',(-3.7996592319632,-1.,-1.42596018777283));
#49737=CARTESIAN_POINT('Ctrl Pts',(-3.7996592319632,1.,-1.42596018777283));
#49738=CARTESIAN_POINT('Ctrl Pts',(-3.79400175744408,-1.,-1.42076028482836));
#49739=CARTESIAN_POINT('Ctrl Pts',(-3.79400175744408,1.,-1.42076028482836));
#49740=CARTESIAN_POINT('Ctrl Pts',(-3.78832489879426,-1.,-1.4155952780383));
#49741=CARTESIAN_POINT('Ctrl Pts',(-3.78832489879426,1.,-1.4155952780383));
#49742=CARTESIAN_POINT('Ctrl Pts',(-3.78262780065471,-1.,-1.41046532282593));
#49743=CARTESIAN_POINT('Ctrl Pts',(-3.78262780065471,1.,-1.41046532282593));
#49744=CARTESIAN_POINT('Ctrl Pts',(-3.77690952014259,-1.,-1.40537056004722));
#49745=CARTESIAN_POINT('Ctrl Pts',(-3.77690952014259,1.,-1.40537056004722));
#49746=CARTESIAN_POINT('Ctrl Pts',(-3.77116930621827,-1.,-1.40031121335505));
#49747=CARTESIAN_POINT('Ctrl Pts',(-3.77116930621827,1.,-1.40031121335505));
#49748=CARTESIAN_POINT('Ctrl Pts',(-3.76540689249074,-1.,-1.39528769118052));
#49749=CARTESIAN_POINT('Ctrl Pts',(-3.76540689249074,1.,-1.39528769118052));
#49750=CARTESIAN_POINT('Ctrl Pts',(-3.75962280650855,-1.,-1.39030069388918));
#49751=CARTESIAN_POINT('Ctrl Pts',(-3.75962280650855,1.,-1.39030069388918));
#49752=CARTESIAN_POINT('Ctrl Pts',(-3.75381861212707,-1.,-1.38535129801176));
#49753=CARTESIAN_POINT('Ctrl Pts',(-3.75381861212707,1.,-1.38535129801176));
#49754=CARTESIAN_POINT('Ctrl Pts',(-3.74799617204729,-1.,-1.38044070763295));
#49755=CARTESIAN_POINT('Ctrl Pts',(-3.74799617204729,1.,-1.38044070763295));
#49756=CARTESIAN_POINT('Ctrl Pts',(-3.74215698162555,-1.,-1.37557002971687));
#49757=CARTESIAN_POINT('Ctrl Pts',(-3.74215698162555,1.,-1.37557002971687));
#49758=CARTESIAN_POINT('Ctrl Pts',(-3.7363014588581,-1.,-1.37074003422739));
#49759=CARTESIAN_POINT('Ctrl Pts',(-3.7363014588581,1.,-1.37074003422739));
#49760=CARTESIAN_POINT('Ctrl Pts',(-3.73042829011295,-1.,-1.36595093298676));
#49761=CARTESIAN_POINT('Ctrl Pts',(-3.73042829011295,1.,-1.36595093298676));
#49762=CARTESIAN_POINT('Ctrl Pts',(-3.72453364678279,-1.,-1.36120211416354));
#49763=CARTESIAN_POINT('Ctrl Pts',(-3.72453364678279,1.,-1.36120211416354));
#49764=CARTESIAN_POINT('Ctrl Pts',(-3.71861271513313,-1.,-1.35649266705037));
#49765=CARTESIAN_POINT('Ctrl Pts',(-3.71861271513313,1.,-1.35649266705037));
#49766=CARTESIAN_POINT('Ctrl Pts',(-3.71266130563054,-1.,-1.35182193384424));
#49767=CARTESIAN_POINT('Ctrl Pts',(-3.71266130563054,1.,-1.35182193384424));
#49768=CARTESIAN_POINT('Ctrl Pts',(-3.70667753188248,-1.,-1.34719008463534));
#49769=CARTESIAN_POINT('Ctrl Pts',(-3.70667753188248,1.,-1.34719008463534));
#49770=CARTESIAN_POINT('Ctrl Pts',(-3.70066324015119,-1.,-1.34259860752933));
#49771=CARTESIAN_POINT('Ctrl Pts',(-3.70066324015119,1.,-1.34259860752933));
#49772=CARTESIAN_POINT('Ctrl Pts',(-3.69462613305708,-1.,-1.33805103398219));
#49773=CARTESIAN_POINT('Ctrl Pts',(-3.69462613305708,1.,-1.33805103398219));
#49774=CARTESIAN_POINT('Ctrl Pts',(-3.68857672413033,-1.,-1.33355191034523));
#49775=CARTESIAN_POINT('Ctrl Pts',(-3.68857672413033,1.,-1.33355191034523));
#49776=CARTESIAN_POINT('Ctrl Pts',(-3.68252441182551,-1.,-1.3291054707274));
#49777=CARTESIAN_POINT('Ctrl Pts',(-3.68252441182551,1.,-1.3291054707274));
#49778=CARTESIAN_POINT('Ctrl Pts',(-3.67647355257912,-1.,-1.32471430856415));
#49779=CARTESIAN_POINT('Ctrl Pts',(-3.67647355257912,1.,-1.32471430856415));
#49780=CARTESIAN_POINT('Ctrl Pts',(-3.67042021752656,-1.,-1.32037828137766));
#49781=CARTESIAN_POINT('Ctrl Pts',(-3.67042021752656,1.,-1.32037828137766));
#49782=CARTESIAN_POINT('Ctrl Pts',(-3.66434688899793,-1.,-1.31609271239911));
#49783=CARTESIAN_POINT('Ctrl Pts',(-3.66434688899793,1.,-1.31609271239911));
#49784=CARTESIAN_POINT('Ctrl Pts',(-3.65822827358617,-1.,-1.31185038411218));
#49785=CARTESIAN_POINT('Ctrl Pts',(-3.65822827358617,1.,-1.31185038411218));
#49786=CARTESIAN_POINT('Ctrl Pts',(-3.65204081987068,-1.,-1.30764479590039));
#49787=CARTESIAN_POINT('Ctrl Pts',(-3.65204081987068,1.,-1.30764479590039));
#49788=CARTESIAN_POINT('Ctrl Pts',(-3.64577181380113,-1.,-1.30347327603774));
#49789=CARTESIAN_POINT('Ctrl Pts',(-3.64577181380113,1.,-1.30347327603774));
#49790=CARTESIAN_POINT('Ctrl Pts',(-3.63942689872808,-1.,-1.2993395590647));
#49791=CARTESIAN_POINT('Ctrl Pts',(-3.63942689872808,1.,-1.2993395590647));
#49792=CARTESIAN_POINT('Ctrl Pts',(-3.63304271631046,-1.,-1.29525810207762));
#49793=CARTESIAN_POINT('Ctrl Pts',(-3.63304271631046,1.,-1.29525810207762));
#49794=CARTESIAN_POINT('Ctrl Pts',(-3.62667616004369,-1.,-1.29125046021878));
#49795=CARTESIAN_POINT('Ctrl Pts',(-3.62667616004369,1.,-1.29125046021878));
#49796=CARTESIAN_POINT('Ctrl Pts',(-3.6203814849236,-1.,-1.28733755029384));
#49797=CARTESIAN_POINT('Ctrl Pts',(-3.6203814849236,1.,-1.28733755029384));
#49798=CARTESIAN_POINT('Ctrl Pts',(-3.61418935913823,-1.,-1.28353255117765));
#49799=CARTESIAN_POINT('Ctrl Pts',(-3.61418935913823,1.,-1.28353255117765));
#49800=CARTESIAN_POINT('Ctrl Pts',(-3.60808907746339,-1.,-1.27983492861691));
#49801=CARTESIAN_POINT('Ctrl Pts',(-3.60808907746339,1.,-1.27983492861691));
#49802=CARTESIAN_POINT('Ctrl Pts',(-3.60199947736298,-1.,-1.27622049908625));
#49803=CARTESIAN_POINT('Ctrl Pts',(-3.60199947736298,1.,-1.27622049908625));
#49804=CARTESIAN_POINT('Ctrl Pts',(-3.59578698050006,-1.,-1.27264798379307));
#49805=CARTESIAN_POINT('Ctrl Pts',(-3.59578698050006,1.,-1.27264798379307));
#49806=CARTESIAN_POINT('Ctrl Pts',(-3.58931807846313,-1.,-1.26907758484709));
#49807=CARTESIAN_POINT('Ctrl Pts',(-3.58931807846313,1.,-1.26907758484709));
#49808=CARTESIAN_POINT('Ctrl Pts',(-3.58250452868618,-1.,-1.26548706249862));
#49809=CARTESIAN_POINT('Ctrl Pts',(-3.58250452868618,1.,-1.26548706249862));
#49810=CARTESIAN_POINT('Ctrl Pts',(-3.5753456065171,-1.,-1.2618866714281));
#49811=CARTESIAN_POINT('Ctrl Pts',(-3.5753456065171,1.,-1.2618866714281));
#49812=CARTESIAN_POINT('Ctrl Pts',(-3.56798645995275,-1.,-1.25834000485716));
#49813=CARTESIAN_POINT('Ctrl Pts',(-3.56798645995275,1.,-1.25834000485716));
#49814=CARTESIAN_POINT('Ctrl Pts',(-3.56071094991199,-1.,-1.25496090900009));
#49815=CARTESIAN_POINT('Ctrl Pts',(-3.56071094991199,1.,-1.25496090900009));
#49816=CARTESIAN_POINT('Ctrl Pts',(-3.55387287418985,-1.,-1.2518879294064));
#49817=CARTESIAN_POINT('Ctrl Pts',(-3.55387287418985,1.,-1.2518879294064));
#49818=CARTESIAN_POINT('Ctrl Pts',(-3.54784190283068,-1.,-1.24926408628003));
#49819=CARTESIAN_POINT('Ctrl Pts',(-3.54784190283068,1.,-1.24926408628003));
#49820=CARTESIAN_POINT('Ctrl Pts',(-3.54294877425964,-1.,-1.24721646231966));
#49821=CARTESIAN_POINT('Ctrl Pts',(-3.54294877425964,1.,-1.24721646231966));
#49822=CARTESIAN_POINT('Ctrl Pts',(-3.53941798195825,-1.,-1.24583101679029));
#49823=CARTESIAN_POINT('Ctrl Pts',(-3.53941798195825,1.,-1.24583101679029));
#49824=CARTESIAN_POINT('Ctrl Pts',(-3.53776753802906,-1.,-1.24528461332987));
#49825=CARTESIAN_POINT('Ctrl Pts',(-3.53776753802906,1.,-1.24528461332987));
#49826=CARTESIAN_POINT('Ctrl Pts',(-3.53720633057798,-1.,-1.24519702335451));
#49827=CARTESIAN_POINT('Ctrl Pts',(-3.53720633057798,1.,-1.24519702335451));
#49828=CARTESIAN_POINT('Ctrl Pts',(-3.53713269667399,-1.,-1.24528174185098));
#49829=CARTESIAN_POINT('Ctrl Pts',(-3.53713269667399,1.,-1.24528174185098));
#49830=CARTESIAN_POINT('Ctrl Pts',(-3.53717101171257,-1.,-1.24535988127942));
#49831=CARTESIAN_POINT('Ctrl Pts',(-3.53717101171257,1.,-1.24535988127942));
#49832=CARTESIAN_POINT('',(-3.90876544355381,1.,-1.53673442965256));
#49833=CARTESIAN_POINT('Ctrl Pts',(-3.90876544355381,1.,-1.53673442965256));
#49834=CARTESIAN_POINT('Ctrl Pts',(-3.90771246855019,1.,-1.53556639217905));
#49835=CARTESIAN_POINT('Ctrl Pts',(-3.90560462813969,1.,-1.53323321827755));
#49836=CARTESIAN_POINT('Ctrl Pts',(-3.90243719631596,1.,-1.52974216056287));
#49837=CARTESIAN_POINT('Ctrl Pts',(-3.89820260708225,1.,-1.52510482991635));
#49838=CARTESIAN_POINT('Ctrl Pts',(-3.89289043533657,1.,-1.51933724329305));
#49839=CARTESIAN_POINT('Ctrl Pts',(-3.88755930033884,1.,-1.51359883110559));
#49840=CARTESIAN_POINT('Ctrl Pts',(-3.88220917950538,1.,-1.50788973857757));
#49841=CARTESIAN_POINT('Ctrl Pts',(-3.87684006372134,1.,-1.50221016176556));
#49842=CARTESIAN_POINT('Ctrl Pts',(-3.87145196998465,1.,-1.49656035399122));
#49843=CARTESIAN_POINT('Ctrl Pts',(-3.86604492575189,1.,-1.4909406116431));
#49844=CARTESIAN_POINT('Ctrl Pts',(-3.86061894706087,1.,-1.48535125509919));
#49845=CARTESIAN_POINT('Ctrl Pts',(-3.85517401698843,1.,-1.4797926099102));
#49846=CARTESIAN_POINT('Ctrl Pts',(-3.84971006847277,1.,-1.47426499018538));
#49847=CARTESIAN_POINT('Ctrl Pts',(-3.84422695454796,1.,-1.46876867426504));
#49848=CARTESIAN_POINT('Ctrl Pts',(-3.83872447159639,1.,-1.46330391180752));
#49849=CARTESIAN_POINT('Ctrl Pts',(-3.83320241775423,1.,-1.45787095220852));
#49850=CARTESIAN_POINT('Ctrl Pts',(-3.82766064519074,1.,-1.45247006796836));
#49851=CARTESIAN_POINT('Ctrl Pts',(-3.82209910620533,1.,-1.44710157648539));
#49852=CARTESIAN_POINT('Ctrl Pts',(-3.81651792398414,1.,-1.44176587041347));
#49853=CARTESIAN_POINT('Ctrl Pts',(-3.81091737726815,1.,-1.43646341556724));
#49854=CARTESIAN_POINT('Ctrl Pts',(-3.80529775429805,1.,-1.4311946992132));
#49855=CARTESIAN_POINT('Ctrl Pts',(-3.7996592319632,1.,-1.42596018777283));
#49856=CARTESIAN_POINT('Ctrl Pts',(-3.79400175744408,1.,-1.42076028482836));
#49857=CARTESIAN_POINT('Ctrl Pts',(-3.78832489879426,1.,-1.4155952780383));
#49858=CARTESIAN_POINT('Ctrl Pts',(-3.78262780065471,1.,-1.41046532282593));
#49859=CARTESIAN_POINT('Ctrl Pts',(-3.77690952014259,1.,-1.40537056004722));
#49860=CARTESIAN_POINT('Ctrl Pts',(-3.77116930621827,1.,-1.40031121335505));
#49861=CARTESIAN_POINT('Ctrl Pts',(-3.76540689249074,1.,-1.39528769118052));
#49862=CARTESIAN_POINT('Ctrl Pts',(-3.75962280650855,1.,-1.39030069388918));
#49863=CARTESIAN_POINT('Ctrl Pts',(-3.75381861212707,1.,-1.38535129801176));
#49864=CARTESIAN_POINT('Ctrl Pts',(-3.74799617204729,1.,-1.38044070763295));
#49865=CARTESIAN_POINT('Ctrl Pts',(-3.74215698162555,1.,-1.37557002971687));
#49866=CARTESIAN_POINT('Ctrl Pts',(-3.7363014588581,1.,-1.37074003422739));
#49867=CARTESIAN_POINT('Ctrl Pts',(-3.73042829011295,1.,-1.36595093298676));
#49868=CARTESIAN_POINT('Ctrl Pts',(-3.72453364678279,1.,-1.36120211416354));
#49869=CARTESIAN_POINT('Ctrl Pts',(-3.71861271513313,1.,-1.35649266705037));
#49870=CARTESIAN_POINT('Ctrl Pts',(-3.71266130563054,1.,-1.35182193384424));
#49871=CARTESIAN_POINT('Ctrl Pts',(-3.70667753188248,1.,-1.34719008463534));
#49872=CARTESIAN_POINT('Ctrl Pts',(-3.70066324015119,1.,-1.34259860752933));
#49873=CARTESIAN_POINT('Ctrl Pts',(-3.69462613305708,1.,-1.33805103398219));
#49874=CARTESIAN_POINT('Ctrl Pts',(-3.68857672413033,1.,-1.33355191034523));
#49875=CARTESIAN_POINT('Ctrl Pts',(-3.68252441182551,1.,-1.3291054707274));
#49876=CARTESIAN_POINT('Ctrl Pts',(-3.67647355257912,1.,-1.32471430856415));
#49877=CARTESIAN_POINT('Ctrl Pts',(-3.67042021752656,1.,-1.32037828137766));
#49878=CARTESIAN_POINT('Ctrl Pts',(-3.66434688899793,1.,-1.31609271239911));
#49879=CARTESIAN_POINT('Ctrl Pts',(-3.65822827358617,1.,-1.31185038411218));
#49880=CARTESIAN_POINT('Ctrl Pts',(-3.65204081987068,1.,-1.30764479590039));
#49881=CARTESIAN_POINT('Ctrl Pts',(-3.64577181380113,1.,-1.30347327603774));
#49882=CARTESIAN_POINT('Ctrl Pts',(-3.63942689872808,1.,-1.2993395590647));
#49883=CARTESIAN_POINT('Ctrl Pts',(-3.63304271631046,1.,-1.29525810207762));
#49884=CARTESIAN_POINT('Ctrl Pts',(-3.62667616004369,1.,-1.29125046021878));
#49885=CARTESIAN_POINT('Ctrl Pts',(-3.6203814849236,1.,-1.28733755029384));
#49886=CARTESIAN_POINT('Ctrl Pts',(-3.61418935913823,1.,-1.28353255117765));
#49887=CARTESIAN_POINT('Ctrl Pts',(-3.60808907746339,1.,-1.27983492861691));
#49888=CARTESIAN_POINT('Ctrl Pts',(-3.60199947736298,1.,-1.27622049908625));
#49889=CARTESIAN_POINT('Ctrl Pts',(-3.59578698050006,1.,-1.27264798379307));
#49890=CARTESIAN_POINT('Ctrl Pts',(-3.58931807846313,1.,-1.26907758484709));
#49891=CARTESIAN_POINT('Ctrl Pts',(-3.58250452868618,1.,-1.26548706249862));
#49892=CARTESIAN_POINT('Ctrl Pts',(-3.5753456065171,1.,-1.2618866714281));
#49893=CARTESIAN_POINT('Ctrl Pts',(-3.56798645995275,1.,-1.25834000485716));
#49894=CARTESIAN_POINT('Ctrl Pts',(-3.56071094991199,1.,-1.25496090900009));
#49895=CARTESIAN_POINT('Ctrl Pts',(-3.55387287418985,1.,-1.2518879294064));
#49896=CARTESIAN_POINT('Ctrl Pts',(-3.54784190283068,1.,-1.24926408628003));
#49897=CARTESIAN_POINT('Ctrl Pts',(-3.54294877425964,1.,-1.24721646231966));
#49898=CARTESIAN_POINT('Ctrl Pts',(-3.53968291130022,1.,-1.24593497226008));
#49899=CARTESIAN_POINT('Ctrl Pts',(-3.53808746578196,1.,-1.24539205388767));
#49900=CARTESIAN_POINT('Ctrl Pts',(-3.5374485926552,1.,-1.2452449899111));
#49901=CARTESIAN_POINT('Ctrl Pts',(-3.53725139174486,1.,-1.24524838931757));
#49902=CARTESIAN_POINT('Ctrl Pts',(-3.5372048861597,1.,-1.24526366418038));
#49903=CARTESIAN_POINT('',(-3.90876544355381,0.,-1.53673442965256));
#49904=CARTESIAN_POINT('Ctrl Pts',(-3.38176002566879,-1.,-1.62055519152809));
#49905=CARTESIAN_POINT('Ctrl Pts',(-3.38176002566879,1.,-1.62055519152809));
#49906=CARTESIAN_POINT('Ctrl Pts',(-3.38167767992676,-1.,-1.62058335162482));
#49907=CARTESIAN_POINT('Ctrl Pts',(-3.38167767992676,1.,-1.62058335162482));
#49908=CARTESIAN_POINT('Ctrl Pts',(-3.38166984193836,-1.,-1.62069532368199));
#49909=CARTESIAN_POINT('Ctrl Pts',(-3.38166984193836,1.,-1.62069532368199));
#49910=CARTESIAN_POINT('Ctrl Pts',(-3.38212861099984,-1.,-1.62103022181151));
#49911=CARTESIAN_POINT('Ctrl Pts',(-3.38212861099984,1.,-1.62103022181151));
#49912=CARTESIAN_POINT('Ctrl Pts',(-3.38368201668574,-1.,-1.62181089631344));
#49913=CARTESIAN_POINT('Ctrl Pts',(-3.38368201668574,1.,-1.62181089631344));
#49914=CARTESIAN_POINT('Ctrl Pts',(-3.38715832179072,-1.,-1.6233278855625));
#49915=CARTESIAN_POINT('Ctrl Pts',(-3.38715832179072,1.,-1.6233278855625));
#49916=CARTESIAN_POINT('Ctrl Pts',(-3.39206617496906,-1.,-1.62533996116713));
#49917=CARTESIAN_POINT('Ctrl Pts',(-3.39206617496906,1.,-1.62533996116713));
#49918=CARTESIAN_POINT('Ctrl Pts',(-3.39818605297991,-1.,-1.62774916464408));
#49919=CARTESIAN_POINT('Ctrl Pts',(-3.39818605297991,1.,-1.62774916464408));
#49920=CARTESIAN_POINT('Ctrl Pts',(-3.40519422740235,-1.,-1.63041148964828));
#49921=CARTESIAN_POINT('Ctrl Pts',(-3.40519422740235,1.,-1.63041148964828));
#49922=CARTESIAN_POINT('Ctrl Pts',(-3.41272817148478,-1.,-1.63316667054044));
#49923=CARTESIAN_POINT('Ctrl Pts',(-3.41272817148478,1.,-1.63316667054044));
#49924=CARTESIAN_POINT('Ctrl Pts',(-3.42043974590882,-1.,-1.63586250099773));
#49925=CARTESIAN_POINT('Ctrl Pts',(-3.42043974590882,1.,-1.63586250099773));
#49926=CARTESIAN_POINT('Ctrl Pts',(-3.42804772926291,-1.,-1.63837876246926));
#49927=CARTESIAN_POINT('Ctrl Pts',(-3.42804772926291,1.,-1.63837876246926));
#49928=CARTESIAN_POINT('Ctrl Pts',(-3.43540451921548,-1.,-1.64065778702023));
#49929=CARTESIAN_POINT('Ctrl Pts',(-3.43540451921548,1.,-1.64065778702023));
#49930=CARTESIAN_POINT('Ctrl Pts',(-3.44250337701888,-1.,-1.64270733821113));
#49931=CARTESIAN_POINT('Ctrl Pts',(-3.44250337701888,1.,-1.64270733821113));
#49932=CARTESIAN_POINT('Ctrl Pts',(-3.44942242546795,-1.,-1.64457408708107));
#49933=CARTESIAN_POINT('Ctrl Pts',(-3.44942242546795,1.,-1.64457408708107));
#49934=CARTESIAN_POINT('Ctrl Pts',(-3.45628421062422,-1.,-1.64632429697521));
#49935=CARTESIAN_POINT('Ctrl Pts',(-3.45628421062422,1.,-1.64632429697521));
#49936=CARTESIAN_POINT('Ctrl Pts',(-3.46321237515,-1.,-1.64802323352738));
#49937=CARTESIAN_POINT('Ctrl Pts',(-3.46321237515,1.,-1.64802323352738));
#49938=CARTESIAN_POINT('Ctrl Pts',(-3.47028140995992,-1.,-1.64971118698256));
#49939=CARTESIAN_POINT('Ctrl Pts',(-3.47028140995992,1.,-1.64971118698256));
#49940=CARTESIAN_POINT('Ctrl Pts',(-3.47749926256476,-1.,-1.65139534930322));
#49941=CARTESIAN_POINT('Ctrl Pts',(-3.47749926256476,1.,-1.65139534930322));
#49942=CARTESIAN_POINT('Ctrl Pts',(-3.48483492840894,-1.,-1.65306335367739));
#49943=CARTESIAN_POINT('Ctrl Pts',(-3.48483492840894,1.,-1.65306335367739));
#49944=CARTESIAN_POINT('Ctrl Pts',(-3.49223525300176,-1.,-1.65469162644468));
#49945=CARTESIAN_POINT('Ctrl Pts',(-3.49223525300176,1.,-1.65469162644468));
#49946=CARTESIAN_POINT('Ctrl Pts',(-3.4996447647794,-1.,-1.65625517961588));
#49947=CARTESIAN_POINT('Ctrl Pts',(-3.4996447647794,1.,-1.65625517961588));
#49948=CARTESIAN_POINT('Ctrl Pts',(-3.50702733146542,-1.,-1.65773832633632));
#49949=CARTESIAN_POINT('Ctrl Pts',(-3.50702733146542,1.,-1.65773832633632));
#49950=CARTESIAN_POINT('Ctrl Pts',(-3.5143763218894,-1.,-1.65913971687342));
#49951=CARTESIAN_POINT('Ctrl Pts',(-3.5143763218894,1.,-1.65913971687342));
#49952=CARTESIAN_POINT('Ctrl Pts',(-3.52170261543815,-1.,-1.66046645222279));
#49953=CARTESIAN_POINT('Ctrl Pts',(-3.52170261543815,1.,-1.66046645222279));
#49954=CARTESIAN_POINT('Ctrl Pts',(-3.52902746211093,-1.,-1.66173058912371));
#49955=CARTESIAN_POINT('Ctrl Pts',(-3.52902746211093,1.,-1.66173058912371));
#49956=CARTESIAN_POINT('Ctrl Pts',(-3.5363738506022,-1.,-1.66294490916111));
#49957=CARTESIAN_POINT('Ctrl Pts',(-3.5363738506022,1.,-1.66294490916111));
#49958=CARTESIAN_POINT('Ctrl Pts',(-3.54375747475014,-1.,-1.66411849222326));
#49959=CARTESIAN_POINT('Ctrl Pts',(-3.54375747475014,1.,-1.66411849222326));
#49960=CARTESIAN_POINT('Ctrl Pts',(-3.55118121342861,-1.,-1.66525401568994));
#49961=CARTESIAN_POINT('Ctrl Pts',(-3.55118121342861,1.,-1.66525401568994));
#49962=CARTESIAN_POINT('Ctrl Pts',(-3.55864015233602,-1.,-1.66635023293114));
#49963=CARTESIAN_POINT('Ctrl Pts',(-3.55864015233602,1.,-1.66635023293114));
#49964=CARTESIAN_POINT('Ctrl Pts',(-3.56612465179422,-1.,-1.66740349220305));
#49965=CARTESIAN_POINT('Ctrl Pts',(-3.56612465179422,1.,-1.66740349220305));
#49966=CARTESIAN_POINT('Ctrl Pts',(-3.57362406285887,-1.,-1.668409574073));
#49967=CARTESIAN_POINT('Ctrl Pts',(-3.57362406285887,1.,-1.668409574073));
#49968=CARTESIAN_POINT('Ctrl Pts',(-3.58113044183829,-1.,-1.66936552908232));
#49969=CARTESIAN_POINT('Ctrl Pts',(-3.58113044183829,1.,-1.66936552908232));
#49970=CARTESIAN_POINT('Ctrl Pts',(-3.58864143097834,-1.,-1.67027110397604));
#49971=CARTESIAN_POINT('Ctrl Pts',(-3.58864143097834,1.,-1.67027110397604));
#49972=CARTESIAN_POINT('Ctrl Pts',(-3.59615824388807,-1.,-1.67112775290707));
#49973=CARTESIAN_POINT('Ctrl Pts',(-3.59615824388807,1.,-1.67112775290707));
#49974=CARTESIAN_POINT('Ctrl Pts',(-3.603684308152,-1.,-1.67193797318597));
#49975=CARTESIAN_POINT('Ctrl Pts',(-3.603684308152,1.,-1.67193797318597));
#49976=CARTESIAN_POINT('Ctrl Pts',(-3.61122367156181,-1.,-1.67270452466968));
#49977=CARTESIAN_POINT('Ctrl Pts',(-3.61122367156181,1.,-1.67270452466968));
#49978=CARTESIAN_POINT('Ctrl Pts',(-3.61877947398184,-1.,-1.67342968196224));
#49979=CARTESIAN_POINT('Ctrl Pts',(-3.61877947398184,1.,-1.67342968196224));
#49980=CARTESIAN_POINT('Ctrl Pts',(-3.62635249450923,-1.,-1.67411452372271));
#49981=CARTESIAN_POINT('Ctrl Pts',(-3.62635249450923,1.,-1.67411452372271));
#49982=CARTESIAN_POINT('Ctrl Pts',(-3.63394189312924,-1.,-1.67475929882971));
#49983=CARTESIAN_POINT('Ctrl Pts',(-3.63394189312924,1.,-1.67475929882971));
#49984=CARTESIAN_POINT('Ctrl Pts',(-3.6415458297234,-1.,-1.67536373264848));
#49985=CARTESIAN_POINT('Ctrl Pts',(-3.6415458297234,1.,-1.67536373264848));
#49986=CARTESIAN_POINT('Ctrl Pts',(-3.64916213574667,-1.,-1.67592735946692));
#49987=CARTESIAN_POINT('Ctrl Pts',(-3.64916213574667,1.,-1.67592735946692));
#49988=CARTESIAN_POINT('Ctrl Pts',(-3.6567889441642,-1.,-1.67644983469449));
#49989=CARTESIAN_POINT('Ctrl Pts',(-3.6567889441642,1.,-1.67644983469449));
#49990=CARTESIAN_POINT('Ctrl Pts',(-3.66442538670968,-1.,-1.67693128053132));
#49991=CARTESIAN_POINT('Ctrl Pts',(-3.66442538670968,1.,-1.67693128053132));
#49992=CARTESIAN_POINT('Ctrl Pts',(-3.67207136294575,-1.,-1.67737217414874));
#49993=CARTESIAN_POINT('Ctrl Pts',(-3.67207136294575,1.,-1.67737217414874));
#49994=CARTESIAN_POINT('Ctrl Pts',(-3.67972724579124,-1.,-1.67777320475848));
#49995=CARTESIAN_POINT('Ctrl Pts',(-3.67972724579124,1.,-1.67777320475848));
#49996=CARTESIAN_POINT('Ctrl Pts',(-3.68739360236487,-1.,-1.67813513867965));
#49997=CARTESIAN_POINT('Ctrl Pts',(-3.68739360236487,1.,-1.67813513867965));
#49998=CARTESIAN_POINT('Ctrl Pts',(-3.6950709275959,-1.,-1.67845869064323));
#49999=CARTESIAN_POINT('Ctrl Pts',(-3.6950709275959,1.,-1.67845869064323));
#50000=CARTESIAN_POINT('Ctrl Pts',(-3.70275932351108,-1.,-1.67874436948667));
#50001=CARTESIAN_POINT('Ctrl Pts',(-3.70275932351108,1.,-1.67874436948667));
#50002=CARTESIAN_POINT('Ctrl Pts',(-3.71045854208343,-1.,-1.67899249793462));
#50003=CARTESIAN_POINT('Ctrl Pts',(-3.71045854208343,1.,-1.67899249793462));
#50004=CARTESIAN_POINT('Ctrl Pts',(-3.71816812842322,-1.,-1.67920328071708));
#50005=CARTESIAN_POINT('Ctrl Pts',(-3.71816812842322,1.,-1.67920328071708));
#50006=CARTESIAN_POINT('Ctrl Pts',(-3.72588753416396,-1.,-1.67937685856652));
#50007=CARTESIAN_POINT('Ctrl Pts',(-3.72588753416396,1.,-1.67937685856652));
#50008=CARTESIAN_POINT('Ctrl Pts',(-3.73361623282543,-1.,-1.67951336376402));
#50009=CARTESIAN_POINT('Ctrl Pts',(-3.73361623282543,1.,-1.67951336376402));
#50010=CARTESIAN_POINT('Ctrl Pts',(-3.74135385965401,-1.,-1.6796129868522));
#50011=CARTESIAN_POINT('Ctrl Pts',(-3.74135385965401,1.,-1.6796129868522));
#50012=CARTESIAN_POINT('Ctrl Pts',(-3.7491002239452,-1.,-1.67967598599525));
#50013=CARTESIAN_POINT('Ctrl Pts',(-3.7491002239452,1.,-1.67967598599525));
#50014=CARTESIAN_POINT('Ctrl Pts',(-3.75685523754493,-1.,-1.67970265841239));
#50015=CARTESIAN_POINT('Ctrl Pts',(-3.75685523754493,1.,-1.67970265841239));
#50016=CARTESIAN_POINT('Ctrl Pts',(-3.76461886684344,-1.,-1.67969332319245));
#50017=CARTESIAN_POINT('Ctrl Pts',(-3.76461886684344,1.,-1.67969332319245));
#50018=CARTESIAN_POINT('Ctrl Pts',(-3.77239107928502,-1.,-1.67964830084993));
#50019=CARTESIAN_POINT('Ctrl Pts',(-3.77239107928502,1.,-1.67964830084993));
#50020=CARTESIAN_POINT('Ctrl Pts',(-3.78017178197317,-1.,-1.67956789212141));
#50021=CARTESIAN_POINT('Ctrl Pts',(-3.78017178197317,1.,-1.67956789212141));
#50022=CARTESIAN_POINT('Ctrl Pts',(-3.7879608002176,-1.,-1.67945236653493));
#50023=CARTESIAN_POINT('Ctrl Pts',(-3.7879608002176,1.,-1.67945236653493));
#50024=CARTESIAN_POINT('Ctrl Pts',(-3.79575791578424,-1.,-1.67930196625548));
#50025=CARTESIAN_POINT('Ctrl Pts',(-3.79575791578424,1.,-1.67930196625548));
#50026=CARTESIAN_POINT('Ctrl Pts',(-3.80356289079005,-1.,-1.67911690648355));
#50027=CARTESIAN_POINT('Ctrl Pts',(-3.80356289079005,1.,-1.67911690648355));
#50028=CARTESIAN_POINT('Ctrl Pts',(-3.81137549624178,-1.,-1.6788973773827));
#50029=CARTESIAN_POINT('Ctrl Pts',(-3.81137549624178,1.,-1.6788973773827));
#50030=CARTESIAN_POINT('Ctrl Pts',(-3.81919554099578,-1.,-1.67864354605954));
#50031=CARTESIAN_POINT('Ctrl Pts',(-3.81919554099578,1.,-1.67864354605954));
#50032=CARTESIAN_POINT('Ctrl Pts',(-3.82702289286713,-1.,-1.6783555575934));
#50033=CARTESIAN_POINT('Ctrl Pts',(-3.82702289286713,1.,-1.6783555575934));
#50034=CARTESIAN_POINT('Ctrl Pts',(-3.83485746513989,-1.,-1.67803353064351));
#50035=CARTESIAN_POINT('Ctrl Pts',(-3.83485746513989,1.,-1.67803353064351));
#50036=CARTESIAN_POINT('Ctrl Pts',(-3.84113085985244,-1.,-1.67774874946079));
#50037=CARTESIAN_POINT('Ctrl Pts',(-3.84113085985244,1.,-1.67774874946079));
#50038=CARTESIAN_POINT('Ctrl Pts',(-3.84583912296459,-1.,-1.6775199114018));
#50039=CARTESIAN_POINT('Ctrl Pts',(-3.84583912296459,1.,-1.6775199114018));
#50040=CARTESIAN_POINT('Ctrl Pts',(-3.84897939430696,-1.,-1.67736057656533));
#50041=CARTESIAN_POINT('Ctrl Pts',(-3.84897939430696,1.,-1.67736057656533));
#50042=CARTESIAN_POINT('Ctrl Pts',(-3.85054988729471,-1.,-1.67727921511438));
#50043=CARTESIAN_POINT('Ctrl Pts',(-3.85054988729471,1.,-1.67727921511438));
#50044=CARTESIAN_POINT('',(-3.38171594275765,1.,-1.62064718014094));
#50045=CARTESIAN_POINT('Ctrl Pts',(-3.38171594275765,-1.,-1.62064718014094));
#50046=CARTESIAN_POINT('Ctrl Pts',(-3.38171594275765,-0.666666666666667,
-1.62064718014094));
#50047=CARTESIAN_POINT('Ctrl Pts',(-3.38171594275765,-0.333333333333333,
-1.62064718014094));
#50048=CARTESIAN_POINT('Ctrl Pts',(-3.38171594275765,0.333333333333333,
-1.62064718014094));
#50049=CARTESIAN_POINT('Ctrl Pts',(-3.38171594275765,0.666666666666667,
-1.62064718014094));
#50050=CARTESIAN_POINT('Ctrl Pts',(-3.38171594275765,1.,-1.62064718014094));
#50051=CARTESIAN_POINT('',(-3.85054988729471,1.,-1.67727921511438));
#50052=CARTESIAN_POINT('',(-3.85054988729471,0.,-1.67727921511438));
#50053=CARTESIAN_POINT('Ctrl Pts',(-3.38171594275765,1.,-1.62064718014094));
#50054=CARTESIAN_POINT('Ctrl Pts',(-3.38173802621259,1.,-1.62069086551492));
#50055=CARTESIAN_POINT('Ctrl Pts',(-3.38187506456922,1.,-1.62083271135947));
#50056=CARTESIAN_POINT('Ctrl Pts',(-3.38243080602409,1.,-1.62118047294498));
#50057=CARTESIAN_POINT('Ctrl Pts',(-3.38394285763222,1.,-1.62192472202769));
#50058=CARTESIAN_POINT('Ctrl Pts',(-3.38715832179072,1.,-1.6233278855625));
#50059=CARTESIAN_POINT('Ctrl Pts',(-3.39206617496906,1.,-1.62533996116713));
#50060=CARTESIAN_POINT('Ctrl Pts',(-3.39818605297991,1.,-1.62774916464408));
#50061=CARTESIAN_POINT('Ctrl Pts',(-3.40519422740235,1.,-1.63041148964828));
#50062=CARTESIAN_POINT('Ctrl Pts',(-3.41272817148478,1.,-1.63316667054044));
#50063=CARTESIAN_POINT('Ctrl Pts',(-3.42043974590882,1.,-1.63586250099773));
#50064=CARTESIAN_POINT('Ctrl Pts',(-3.42804772926291,1.,-1.63837876246926));
#50065=CARTESIAN_POINT('Ctrl Pts',(-3.43540451921548,1.,-1.64065778702023));
#50066=CARTESIAN_POINT('Ctrl Pts',(-3.44250337701888,1.,-1.64270733821113));
#50067=CARTESIAN_POINT('Ctrl Pts',(-3.44942242546795,1.,-1.64457408708107));
#50068=CARTESIAN_POINT('Ctrl Pts',(-3.45628421062422,1.,-1.64632429697521));
#50069=CARTESIAN_POINT('Ctrl Pts',(-3.46321237515,1.,-1.64802323352738));
#50070=CARTESIAN_POINT('Ctrl Pts',(-3.47028140995992,1.,-1.64971118698256));
#50071=CARTESIAN_POINT('Ctrl Pts',(-3.47749926256476,1.,-1.65139534930322));
#50072=CARTESIAN_POINT('Ctrl Pts',(-3.48483492840894,1.,-1.65306335367739));
#50073=CARTESIAN_POINT('Ctrl Pts',(-3.49223525300176,1.,-1.65469162644468));
#50074=CARTESIAN_POINT('Ctrl Pts',(-3.4996447647794,1.,-1.65625517961588));
#50075=CARTESIAN_POINT('Ctrl Pts',(-3.50702733146542,1.,-1.65773832633632));
#50076=CARTESIAN_POINT('Ctrl Pts',(-3.5143763218894,1.,-1.65913971687342));
#50077=CARTESIAN_POINT('Ctrl Pts',(-3.52170261543815,1.,-1.66046645222279));
#50078=CARTESIAN_POINT('Ctrl Pts',(-3.52902746211093,1.,-1.66173058912371));
#50079=CARTESIAN_POINT('Ctrl Pts',(-3.5363738506022,1.,-1.66294490916111));
#50080=CARTESIAN_POINT('Ctrl Pts',(-3.54375747475014,1.,-1.66411849222326));
#50081=CARTESIAN_POINT('Ctrl Pts',(-3.55118121342861,1.,-1.66525401568994));
#50082=CARTESIAN_POINT('Ctrl Pts',(-3.55864015233602,1.,-1.66635023293114));
#50083=CARTESIAN_POINT('Ctrl Pts',(-3.56612465179422,1.,-1.66740349220305));
#50084=CARTESIAN_POINT('Ctrl Pts',(-3.57362406285887,1.,-1.668409574073));
#50085=CARTESIAN_POINT('Ctrl Pts',(-3.58113044183829,1.,-1.66936552908232));
#50086=CARTESIAN_POINT('Ctrl Pts',(-3.58864143097834,1.,-1.67027110397604));
#50087=CARTESIAN_POINT('Ctrl Pts',(-3.59615824388807,1.,-1.67112775290707));
#50088=CARTESIAN_POINT('Ctrl Pts',(-3.603684308152,1.,-1.67193797318597));
#50089=CARTESIAN_POINT('Ctrl Pts',(-3.61122367156181,1.,-1.67270452466968));
#50090=CARTESIAN_POINT('Ctrl Pts',(-3.61877947398184,1.,-1.67342968196224));
#50091=CARTESIAN_POINT('Ctrl Pts',(-3.62635249450923,1.,-1.67411452372271));
#50092=CARTESIAN_POINT('Ctrl Pts',(-3.63394189312924,1.,-1.67475929882971));
#50093=CARTESIAN_POINT('Ctrl Pts',(-3.6415458297234,1.,-1.67536373264848));
#50094=CARTESIAN_POINT('Ctrl Pts',(-3.64916213574667,1.,-1.67592735946692));
#50095=CARTESIAN_POINT('Ctrl Pts',(-3.6567889441642,1.,-1.67644983469449));
#50096=CARTESIAN_POINT('Ctrl Pts',(-3.66442538670968,1.,-1.67693128053132));
#50097=CARTESIAN_POINT('Ctrl Pts',(-3.67207136294575,1.,-1.67737217414874));
#50098=CARTESIAN_POINT('Ctrl Pts',(-3.67972724579124,1.,-1.67777320475848));
#50099=CARTESIAN_POINT('Ctrl Pts',(-3.68739360236487,1.,-1.67813513867965));
#50100=CARTESIAN_POINT('Ctrl Pts',(-3.6950709275959,1.,-1.67845869064323));
#50101=CARTESIAN_POINT('Ctrl Pts',(-3.70275932351108,1.,-1.67874436948667));
#50102=CARTESIAN_POINT('Ctrl Pts',(-3.71045854208343,1.,-1.67899249793462));
#50103=CARTESIAN_POINT('Ctrl Pts',(-3.71816812842322,1.,-1.67920328071708));
#50104=CARTESIAN_POINT('Ctrl Pts',(-3.72588753416396,1.,-1.67937685856652));
#50105=CARTESIAN_POINT('Ctrl Pts',(-3.73361623282543,1.,-1.67951336376402));
#50106=CARTESIAN_POINT('Ctrl Pts',(-3.74135385965401,1.,-1.6796129868522));
#50107=CARTESIAN_POINT('Ctrl Pts',(-3.7491002239452,1.,-1.67967598599525));
#50108=CARTESIAN_POINT('Ctrl Pts',(-3.75685523754493,1.,-1.67970265841239));
#50109=CARTESIAN_POINT('Ctrl Pts',(-3.76461886684344,1.,-1.67969332319245));
#50110=CARTESIAN_POINT('Ctrl Pts',(-3.77239107928502,1.,-1.67964830084993));
#50111=CARTESIAN_POINT('Ctrl Pts',(-3.78017178197317,1.,-1.67956789212141));
#50112=CARTESIAN_POINT('Ctrl Pts',(-3.7879608002176,1.,-1.67945236653493));
#50113=CARTESIAN_POINT('Ctrl Pts',(-3.79575791578424,1.,-1.67930196625548));
#50114=CARTESIAN_POINT('Ctrl Pts',(-3.80356289079005,1.,-1.67911690648355));
#50115=CARTESIAN_POINT('Ctrl Pts',(-3.81137549624178,1.,-1.6788973773827));
#50116=CARTESIAN_POINT('Ctrl Pts',(-3.81919554099578,1.,-1.67864354605954));
#50117=CARTESIAN_POINT('Ctrl Pts',(-3.82702289286713,1.,-1.6783555575934));
#50118=CARTESIAN_POINT('Ctrl Pts',(-3.83485746513989,1.,-1.67803353064351));
#50119=CARTESIAN_POINT('Ctrl Pts',(-3.84113085985244,1.,-1.67774874946079));
#50120=CARTESIAN_POINT('Ctrl Pts',(-3.84583912296459,1.,-1.6775199114018));
#50121=CARTESIAN_POINT('Ctrl Pts',(-3.84897939430696,1.,-1.67736057656533));
#50122=CARTESIAN_POINT('Ctrl Pts',(-3.85054988729471,1.,-1.67727921511438));
#50123=CARTESIAN_POINT('Origin',(-3.85054988729471,0.,-1.67727921511438));
#50124=CARTESIAN_POINT('',(-3.90876544355381,1.,-1.53673442965256));
#50125=CARTESIAN_POINT('Origin',(0.,0.,0.));
#50126=CARTESIAN_POINT('',(-3.29885386921599,1.,-1.78327315618183));
#50127=CARTESIAN_POINT('Origin',(0.,1.,0.));
#50128=CARTESIAN_POINT('Ctrl Pts',(-3.29885386921599,1.,-1.78327315618183));
#50129=CARTESIAN_POINT('Ctrl Pts',(-3.29885386921599,0.666666666666667,
-1.78327315618183));
#50130=CARTESIAN_POINT('Ctrl Pts',(-3.29885386921599,0.333333333333333,
-1.78327315618183));
#50131=CARTESIAN_POINT('Ctrl Pts',(-3.29885386921599,-0.333333333333333,
-1.78327315618183));
#50132=CARTESIAN_POINT('Ctrl Pts',(-3.29885386921599,-0.666666666666667,
-1.78327315618183));
#50133=CARTESIAN_POINT('Ctrl Pts',(-3.29885386921599,-1.,-1.78327315618183));
#50134=CARTESIAN_POINT('Ctrl Pts',(-3.62024382630768,-1.,-2.12928030988903));
#50135=CARTESIAN_POINT('Ctrl Pts',(-3.62024382630768,1.,-2.12928030988903));
#50136=CARTESIAN_POINT('Ctrl Pts',(-3.61938653649098,-1.,-2.12796193131368));
#50137=CARTESIAN_POINT('Ctrl Pts',(-3.61938653649098,1.,-2.12796193131368));
#50138=CARTESIAN_POINT('Ctrl Pts',(-3.61766963590482,-1.,-2.12532774376758));
#50139=CARTESIAN_POINT('Ctrl Pts',(-3.61766963590482,1.,-2.12532774376758));
#50140=CARTESIAN_POINT('Ctrl Pts',(-3.61508732216891,-1.,-2.12138417126355));
#50141=CARTESIAN_POINT('Ctrl Pts',(-3.61508732216891,1.,-2.12138417126355));
#50142=CARTESIAN_POINT('Ctrl Pts',(-3.61163030609447,-1.,-2.11614149815106));
#50143=CARTESIAN_POINT('Ctrl Pts',(-3.61163030609447,1.,-2.11614149815106));
#50144=CARTESIAN_POINT('Ctrl Pts',(-3.60728578532601,-1.,-2.10961391334462));
#50145=CARTESIAN_POINT('Ctrl Pts',(-3.60728578532601,1.,-2.10961391334462));
#50146=CARTESIAN_POINT('Ctrl Pts',(-3.60291797088734,-1.,-2.1031121772821));
#50147=CARTESIAN_POINT('Ctrl Pts',(-3.60291797088734,1.,-2.1031121772821));
#50148=CARTESIAN_POINT('Ctrl Pts',(-3.59852681775485,-1.,-2.09663642986631));
#50149=CARTESIAN_POINT('Ctrl Pts',(-3.59852681775485,1.,-2.09663642986631));
#50150=CARTESIAN_POINT('Ctrl Pts',(-3.59411228625588,-1.,-2.09018686331416));
#50151=CARTESIAN_POINT('Ctrl Pts',(-3.59411228625588,1.,-2.09018686331416));
#50152=CARTESIAN_POINT('Ctrl Pts',(-3.58967435355088,-1.,-2.08376373048756));
#50153=CARTESIAN_POINT('Ctrl Pts',(-3.58967435355088,1.,-2.08376373048756));
#50154=CARTESIAN_POINT('Ctrl Pts',(-3.58521300039299,-1.,-2.07736732842117));
#50155=CARTESIAN_POINT('Ctrl Pts',(-3.58521300039299,1.,-2.07736732842117));
#50156=CARTESIAN_POINT('Ctrl Pts',(-3.58072819250442,-1.,-2.07099797605747));
#50157=CARTESIAN_POINT('Ctrl Pts',(-3.58072819250442,1.,-2.07099797605747));
#50158=CARTESIAN_POINT('Ctrl Pts',(-3.576219862243,-1.,-2.06465599229174));
#50159=CARTESIAN_POINT('Ctrl Pts',(-3.576219862243,1.,-2.06465599229174));
#50160=CARTESIAN_POINT('Ctrl Pts',(-3.57168789423507,-1.,-2.05834167687523));
#50161=CARTESIAN_POINT('Ctrl Pts',(-3.57168789423507,1.,-2.05834167687523));
#50162=CARTESIAN_POINT('Ctrl Pts',(-3.56713209978207,-1.,-2.0520552817309));
#50163=CARTESIAN_POINT('Ctrl Pts',(-3.56713209978207,1.,-2.0520552817309));
#50164=CARTESIAN_POINT('Ctrl Pts',(-3.5625522387181,-1.,-2.04579702159056));
#50165=CARTESIAN_POINT('Ctrl Pts',(-3.5625522387181,1.,-2.04579702159056));
#50166=CARTESIAN_POINT('Ctrl Pts',(-3.55794807265052,-1.,-2.03956711120099));
#50167=CARTESIAN_POINT('Ctrl Pts',(-3.55794807265052,1.,-2.03956711120099));
#50168=CARTESIAN_POINT('Ctrl Pts',(-3.55331941294018,-1.,-2.03336579658174));
#50169=CARTESIAN_POINT('Ctrl Pts',(-3.55331941294018,1.,-2.03336579658174));
#50170=CARTESIAN_POINT('Ctrl Pts',(-3.54866616282173,-1.,-2.02719338376144));
#50171=CARTESIAN_POINT('Ctrl Pts',(-3.54866616282173,1.,-2.02719338376144));
#50172=CARTESIAN_POINT('Ctrl Pts',(-3.54398838254011,-1.,-2.0210502798303));
#50173=CARTESIAN_POINT('Ctrl Pts',(-3.54398838254011,1.,-2.0210502798303));
#50174=CARTESIAN_POINT('Ctrl Pts',(-3.53928627453503,-1.,-2.0149369884727));
#50175=CARTESIAN_POINT('Ctrl Pts',(-3.53928627453503,1.,-2.0149369884727));
#50176=CARTESIAN_POINT('Ctrl Pts',(-3.53456004727321,-1.,-2.00885403604685));
#50177=CARTESIAN_POINT('Ctrl Pts',(-3.53456004727321,1.,-2.00885403604685));
#50178=CARTESIAN_POINT('Ctrl Pts',(-3.52980980250181,-1.,-2.00280191090341));
#50179=CARTESIAN_POINT('Ctrl Pts',(-3.52980980250181,1.,-2.00280191090341));
#50180=CARTESIAN_POINT('Ctrl Pts',(-3.52503542491745,-1.,-1.99678100339305));
#50181=CARTESIAN_POINT('Ctrl Pts',(-3.52503542491745,1.,-1.99678100339305));
#50182=CARTESIAN_POINT('Ctrl Pts',(-3.52023644289195,-1.,-1.99079153006143));
#50183=CARTESIAN_POINT('Ctrl Pts',(-3.52023644289195,1.,-1.99079153006143));
#50184=CARTESIAN_POINT('Ctrl Pts',(-3.51541198728362,-1.,-1.98483351061066));
#50185=CARTESIAN_POINT('Ctrl Pts',(-3.51541198728362,1.,-1.98483351061066));
#50186=CARTESIAN_POINT('Ctrl Pts',(-3.51056110478334,-1.,-1.97890693666316));
#50187=CARTESIAN_POINT('Ctrl Pts',(-3.51056110478334,1.,-1.97890693666316));
#50188=CARTESIAN_POINT('Ctrl Pts',(-3.505683018611,-1.,-1.9730119116298));
#50189=CARTESIAN_POINT('Ctrl Pts',(-3.505683018611,1.,-1.9730119116298));
#50190=CARTESIAN_POINT('Ctrl Pts',(-3.50077740176262,-1.,-1.9671487972405));
#50191=CARTESIAN_POINT('Ctrl Pts',(-3.50077740176262,1.,-1.9671487972405));
#50192=CARTESIAN_POINT('Ctrl Pts',(-3.49584466573045,-1.,-1.96131836776489));
#50193=CARTESIAN_POINT('Ctrl Pts',(-3.49584466573045,1.,-1.96131836776489));
#50194=CARTESIAN_POINT('Ctrl Pts',(-3.49088618670967,-1.,-1.95552193112071));
#50195=CARTESIAN_POINT('Ctrl Pts',(-3.49088618670967,1.,-1.95552193112071));
#50196=CARTESIAN_POINT('Ctrl Pts',(-3.485903616108,-1.,-1.94976096795902));
#50197=CARTESIAN_POINT('Ctrl Pts',(-3.485903616108,1.,-1.94976096795902));
#50198=CARTESIAN_POINT('Ctrl Pts',(-3.48089825770411,-1.,-1.94403680554062));
#50199=CARTESIAN_POINT('Ctrl Pts',(-3.48089825770411,1.,-1.94403680554062));
#50200=CARTESIAN_POINT('Ctrl Pts',(-3.47587040389916,-1.,-1.93835026973888));
#50201=CARTESIAN_POINT('Ctrl Pts',(-3.47587040389916,1.,-1.93835026973888));
#50202=CARTESIAN_POINT('Ctrl Pts',(-3.47081872409783,-1.,-1.93270136427083));
#50203=CARTESIAN_POINT('Ctrl Pts',(-3.47081872409783,1.,-1.93270136427083));
#50204=CARTESIAN_POINT('Ctrl Pts',(-3.46573953254084,-1.,-1.92708888591159));
#50205=CARTESIAN_POINT('Ctrl Pts',(-3.46573953254084,1.,-1.92708888591159));
#50206=CARTESIAN_POINT('Ctrl Pts',(-3.4606282172248,-1.,-1.9215111821321));
#50207=CARTESIAN_POINT('Ctrl Pts',(-3.4606282172248,1.,-1.9215111821321));
#50208=CARTESIAN_POINT('Ctrl Pts',(-3.45548074309943,-1.,-1.9159669478406));
#50209=CARTESIAN_POINT('Ctrl Pts',(-3.45548074309943,1.,-1.9159669478406));
#50210=CARTESIAN_POINT('Ctrl Pts',(-3.45029522038885,-1.,-1.91045605593638));
#50211=CARTESIAN_POINT('Ctrl Pts',(-3.45029522038885,1.,-1.91045605593638));
#50212=CARTESIAN_POINT('Ctrl Pts',(-3.44507323983374,-1.,-1.90498026502308));
#50213=CARTESIAN_POINT('Ctrl Pts',(-3.44507323983374,1.,-1.90498026502308));
#50214=CARTESIAN_POINT('Ctrl Pts',(-3.43982185678105,-1.,-1.89954426803392));
#50215=CARTESIAN_POINT('Ctrl Pts',(-3.43982185678105,1.,-1.89954426803392));
#50216=CARTESIAN_POINT('Ctrl Pts',(-3.43455074411591,-1.,-1.89415420002553));
#50217=CARTESIAN_POINT('Ctrl Pts',(-3.43455074411591,1.,-1.89415420002553));
#50218=CARTESIAN_POINT('Ctrl Pts',(-3.42926852222174,-1.,-1.88881571322018));
#50219=CARTESIAN_POINT('Ctrl Pts',(-3.42926852222174,1.,-1.88881571322018));
#50220=CARTESIAN_POINT('Ctrl Pts',(-3.42397908819741,-1.,-1.88353205062063));
#50221=CARTESIAN_POINT('Ctrl Pts',(-3.42397908819741,1.,-1.88353205062063));
#50222=CARTESIAN_POINT('Ctrl Pts',(-3.4186785838376,-1.,-1.87830245689338));
#50223=CARTESIAN_POINT('Ctrl Pts',(-3.4186785838376,1.,-1.87830245689338));
#50224=CARTESIAN_POINT('Ctrl Pts',(-3.41335043875182,-1.,-1.87311957248106));
#50225=CARTESIAN_POINT('Ctrl Pts',(-3.41335043875182,1.,-1.87311957248106));
#50226=CARTESIAN_POINT('Ctrl Pts',(-3.40797080000513,-1.,-1.86797231196635));
#50227=CARTESIAN_POINT('Ctrl Pts',(-3.40797080000513,1.,-1.86797231196635));
#50228=CARTESIAN_POINT('Ctrl Pts',(-3.40251742305445,-1.,-1.86285057051228));
#50229=CARTESIAN_POINT('Ctrl Pts',(-3.40251742305445,1.,-1.86285057051228));
#50230=CARTESIAN_POINT('Ctrl Pts',(-3.39697816833056,-1.,-1.85774972037055));
#50231=CARTESIAN_POINT('Ctrl Pts',(-3.39697816833056,1.,-1.85774972037055));
#50232=CARTESIAN_POINT('Ctrl Pts',(-3.39135802549415,-1.,-1.85267433291778));
#50233=CARTESIAN_POINT('Ctrl Pts',(-3.39135802549415,1.,-1.85267433291778));
#50234=CARTESIAN_POINT('Ctrl Pts',(-3.38569092349639,-1.,-1.84764441927778));
#50235=CARTESIAN_POINT('Ctrl Pts',(-3.38569092349639,1.,-1.84764441927778));
#50236=CARTESIAN_POINT('Ctrl Pts',(-3.38002968341222,-1.,-1.84269016931679));
#50237=CARTESIAN_POINT('Ctrl Pts',(-3.38002968341222,1.,-1.84269016931679));
#50238=CARTESIAN_POINT('Ctrl Pts',(-3.37442462015914,-1.,-1.83784072967111));
#50239=CARTESIAN_POINT('Ctrl Pts',(-3.37442462015914,1.,-1.83784072967111));
#50240=CARTESIAN_POINT('Ctrl Pts',(-3.36890396271864,-1.,-1.83311391452338));
#50241=CARTESIAN_POINT('Ctrl Pts',(-3.36890396271864,1.,-1.83311391452338));
#50242=CARTESIAN_POINT('Ctrl Pts',(-3.36345722124127,-1.,-1.82850752153182));
#50243=CARTESIAN_POINT('Ctrl Pts',(-3.36345722124127,1.,-1.82850752153182));
#50244=CARTESIAN_POINT('Ctrl Pts',(-3.35800801557326,-1.,-1.82398496829247));
#50245=CARTESIAN_POINT('Ctrl Pts',(-3.35800801557326,1.,-1.82398496829247));
#50246=CARTESIAN_POINT('Ctrl Pts',(-3.35243086937451,-1.,-1.81948458796748));
#50247=CARTESIAN_POINT('Ctrl Pts',(-3.35243086937451,1.,-1.81948458796748));
#50248=CARTESIAN_POINT('Ctrl Pts',(-3.34660014370527,-1.,-1.81494618732772));
#50249=CARTESIAN_POINT('Ctrl Pts',(-3.34660014370527,1.,-1.81494618732772));
#50250=CARTESIAN_POINT('Ctrl Pts',(-3.34043216147532,-1.,-1.81033399625311));
#50251=CARTESIAN_POINT('Ctrl Pts',(-3.34043216147532,1.,-1.81033399625311));
#50252=CARTESIAN_POINT('Ctrl Pts',(-3.33392460276874,-1.,-1.80565802981138));
#50253=CARTESIAN_POINT('Ctrl Pts',(-3.33392460276874,1.,-1.80565802981138));
#50254=CARTESIAN_POINT('Ctrl Pts',(-3.3272108803981,-1.,-1.80100380443535));
#50255=CARTESIAN_POINT('Ctrl Pts',(-3.3272108803981,1.,-1.80100380443535));
#50256=CARTESIAN_POINT('Ctrl Pts',(-3.32055355101168,-1.,-1.79652817033444));
#50257=CARTESIAN_POINT('Ctrl Pts',(-3.32055355101168,1.,-1.79652817033444));
#50258=CARTESIAN_POINT('Ctrl Pts',(-3.31428038326763,-1.,-1.79242331350137));
#50259=CARTESIAN_POINT('Ctrl Pts',(-3.31428038326763,1.,-1.79242331350137));
#50260=CARTESIAN_POINT('Ctrl Pts',(-3.30873412266954,-1.,-1.78888832245965));
#50261=CARTESIAN_POINT('Ctrl Pts',(-3.30873412266954,1.,-1.78888832245965));
#50262=CARTESIAN_POINT('Ctrl Pts',(-3.30422155558973,-1.,-1.78610045419769));
#50263=CARTESIAN_POINT('Ctrl Pts',(-3.30422155558973,1.,-1.78610045419769));
#50264=CARTESIAN_POINT('Ctrl Pts',(-3.30095096463082,-1.,-1.78417972819696));
#50265=CARTESIAN_POINT('Ctrl Pts',(-3.30095096463082,1.,-1.78417972819696));
#50266=CARTESIAN_POINT('Ctrl Pts',(-3.29940631673818,-1.,-1.78338186555671));
#50267=CARTESIAN_POINT('Ctrl Pts',(-3.29940631673818,1.,-1.78338186555671));
#50268=CARTESIAN_POINT('Ctrl Pts',(-3.29886572077303,-1.,-1.78320756177191));
#50269=CARTESIAN_POINT('Ctrl Pts',(-3.29886572077303,1.,-1.78320756177191));
#50270=CARTESIAN_POINT('Ctrl Pts',(-3.29877974053191,-1.,-1.78327971836272));
#50271=CARTESIAN_POINT('Ctrl Pts',(-3.29877974053191,1.,-1.78327971836272));
#50272=CARTESIAN_POINT('Ctrl Pts',(-3.2988053601491,-1.,-1.7833628895577));
#50273=CARTESIAN_POINT('Ctrl Pts',(-3.2988053601491,1.,-1.7833628895577));
#50274=CARTESIAN_POINT('',(-3.62024382630768,1.,-2.12928030988903));
#50275=CARTESIAN_POINT('Ctrl Pts',(-3.62024382630768,1.,-2.12928030988903));
#50276=CARTESIAN_POINT('Ctrl Pts',(-3.61938653649098,1.,-2.12796193131368));
#50277=CARTESIAN_POINT('Ctrl Pts',(-3.61766963590482,1.,-2.12532774376758));
#50278=CARTESIAN_POINT('Ctrl Pts',(-3.61508732216891,1.,-2.12138417126355));
#50279=CARTESIAN_POINT('Ctrl Pts',(-3.61163030609447,1.,-2.11614149815106));
#50280=CARTESIAN_POINT('Ctrl Pts',(-3.60728578532601,1.,-2.10961391334462));
#50281=CARTESIAN_POINT('Ctrl Pts',(-3.60291797088734,1.,-2.1031121772821));
#50282=CARTESIAN_POINT('Ctrl Pts',(-3.59852681775485,1.,-2.09663642986631));
#50283=CARTESIAN_POINT('Ctrl Pts',(-3.59411228625588,1.,-2.09018686331416));
#50284=CARTESIAN_POINT('Ctrl Pts',(-3.58967435355088,1.,-2.08376373048756));
#50285=CARTESIAN_POINT('Ctrl Pts',(-3.58521300039299,1.,-2.07736732842117));
#50286=CARTESIAN_POINT('Ctrl Pts',(-3.58072819250442,1.,-2.07099797605747));
#50287=CARTESIAN_POINT('Ctrl Pts',(-3.576219862243,1.,-2.06465599229174));
#50288=CARTESIAN_POINT('Ctrl Pts',(-3.57168789423507,1.,-2.05834167687523));
#50289=CARTESIAN_POINT('Ctrl Pts',(-3.56713209978207,1.,-2.0520552817309));
#50290=CARTESIAN_POINT('Ctrl Pts',(-3.5625522387181,1.,-2.04579702159056));
#50291=CARTESIAN_POINT('Ctrl Pts',(-3.55794807265052,1.,-2.03956711120099));
#50292=CARTESIAN_POINT('Ctrl Pts',(-3.55331941294018,1.,-2.03336579658174));
#50293=CARTESIAN_POINT('Ctrl Pts',(-3.54866616282173,1.,-2.02719338376144));
#50294=CARTESIAN_POINT('Ctrl Pts',(-3.54398838254011,1.,-2.0210502798303));
#50295=CARTESIAN_POINT('Ctrl Pts',(-3.53928627453503,1.,-2.0149369884727));
#50296=CARTESIAN_POINT('Ctrl Pts',(-3.53456004727321,1.,-2.00885403604685));
#50297=CARTESIAN_POINT('Ctrl Pts',(-3.52980980250181,1.,-2.00280191090341));
#50298=CARTESIAN_POINT('Ctrl Pts',(-3.52503542491745,1.,-1.99678100339305));
#50299=CARTESIAN_POINT('Ctrl Pts',(-3.52023644289195,1.,-1.99079153006143));
#50300=CARTESIAN_POINT('Ctrl Pts',(-3.51541198728362,1.,-1.98483351061066));
#50301=CARTESIAN_POINT('Ctrl Pts',(-3.51056110478334,1.,-1.97890693666316));
#50302=CARTESIAN_POINT('Ctrl Pts',(-3.505683018611,1.,-1.9730119116298));
#50303=CARTESIAN_POINT('Ctrl Pts',(-3.50077740176262,1.,-1.9671487972405));
#50304=CARTESIAN_POINT('Ctrl Pts',(-3.49584466573045,1.,-1.96131836776489));
#50305=CARTESIAN_POINT('Ctrl Pts',(-3.49088618670967,1.,-1.95552193112071));
#50306=CARTESIAN_POINT('Ctrl Pts',(-3.485903616108,1.,-1.94976096795902));
#50307=CARTESIAN_POINT('Ctrl Pts',(-3.48089825770411,1.,-1.94403680554062));
#50308=CARTESIAN_POINT('Ctrl Pts',(-3.47587040389916,1.,-1.93835026973888));
#50309=CARTESIAN_POINT('Ctrl Pts',(-3.47081872409783,1.,-1.93270136427083));
#50310=CARTESIAN_POINT('Ctrl Pts',(-3.46573953254084,1.,-1.92708888591159));
#50311=CARTESIAN_POINT('Ctrl Pts',(-3.4606282172248,1.,-1.9215111821321));
#50312=CARTESIAN_POINT('Ctrl Pts',(-3.45548074309943,1.,-1.9159669478406));
#50313=CARTESIAN_POINT('Ctrl Pts',(-3.45029522038885,1.,-1.91045605593638));
#50314=CARTESIAN_POINT('Ctrl Pts',(-3.44507323983374,1.,-1.90498026502308));
#50315=CARTESIAN_POINT('Ctrl Pts',(-3.43982185678105,1.,-1.89954426803392));
#50316=CARTESIAN_POINT('Ctrl Pts',(-3.43455074411591,1.,-1.89415420002553));
#50317=CARTESIAN_POINT('Ctrl Pts',(-3.42926852222174,1.,-1.88881571322018));
#50318=CARTESIAN_POINT('Ctrl Pts',(-3.42397908819741,1.,-1.88353205062063));
#50319=CARTESIAN_POINT('Ctrl Pts',(-3.4186785838376,1.,-1.87830245689338));
#50320=CARTESIAN_POINT('Ctrl Pts',(-3.41335043875182,1.,-1.87311957248106));
#50321=CARTESIAN_POINT('Ctrl Pts',(-3.40797080000513,1.,-1.86797231196635));
#50322=CARTESIAN_POINT('Ctrl Pts',(-3.40251742305445,1.,-1.86285057051228));
#50323=CARTESIAN_POINT('Ctrl Pts',(-3.39697816833056,1.,-1.85774972037055));
#50324=CARTESIAN_POINT('Ctrl Pts',(-3.39135802549415,1.,-1.85267433291778));
#50325=CARTESIAN_POINT('Ctrl Pts',(-3.38569092349639,1.,-1.84764441927778));
#50326=CARTESIAN_POINT('Ctrl Pts',(-3.38002968341222,1.,-1.84269016931679));
#50327=CARTESIAN_POINT('Ctrl Pts',(-3.37442462015914,1.,-1.83784072967111));
#50328=CARTESIAN_POINT('Ctrl Pts',(-3.36890396271864,1.,-1.83311391452338));
#50329=CARTESIAN_POINT('Ctrl Pts',(-3.36345722124127,1.,-1.82850752153182));
#50330=CARTESIAN_POINT('Ctrl Pts',(-3.35800801557326,1.,-1.82398496829247));
#50331=CARTESIAN_POINT('Ctrl Pts',(-3.35243086937451,1.,-1.81948458796748));
#50332=CARTESIAN_POINT('Ctrl Pts',(-3.34660014370527,1.,-1.81494618732772));
#50333=CARTESIAN_POINT('Ctrl Pts',(-3.34043216147532,1.,-1.81033399625311));
#50334=CARTESIAN_POINT('Ctrl Pts',(-3.33392460276874,1.,-1.80565802981138));
#50335=CARTESIAN_POINT('Ctrl Pts',(-3.3272108803981,1.,-1.80100380443535));
#50336=CARTESIAN_POINT('Ctrl Pts',(-3.32055355101168,1.,-1.79652817033444));
#50337=CARTESIAN_POINT('Ctrl Pts',(-3.31428038326763,1.,-1.79242331350137));
#50338=CARTESIAN_POINT('Ctrl Pts',(-3.30873412266954,1.,-1.78888832245965));
#50339=CARTESIAN_POINT('Ctrl Pts',(-3.30422155558973,1.,-1.78610045419769));
#50340=CARTESIAN_POINT('Ctrl Pts',(-3.30119637003466,1.,-1.7843238478823));
#50341=CARTESIAN_POINT('Ctrl Pts',(-3.29970549824336,1.,-1.78353803106983));
#50342=CARTESIAN_POINT('Ctrl Pts',(-3.29909749657945,1.,-1.78329283591903));
#50343=CARTESIAN_POINT('Ctrl Pts',(-3.29890219175522,1.,-1.78326534445426));
#50344=CARTESIAN_POINT('Ctrl Pts',(-3.29885386921599,1.,-1.78327315618183));
#50345=CARTESIAN_POINT('',(-3.62024382630768,0.,-2.12928030988903));
#50346=CARTESIAN_POINT('Ctrl Pts',(-3.08661426358891,-1.,-2.12962728847315));
#50347=CARTESIAN_POINT('Ctrl Pts',(-3.08661426358891,1.,-2.12962728847315));
#50348=CARTESIAN_POINT('Ctrl Pts',(-3.08652852644995,-1.,-2.12964222016025));
#50349=CARTESIAN_POINT('Ctrl Pts',(-3.08652852644995,1.,-2.12964222016025));
#50350=CARTESIAN_POINT('Ctrl Pts',(-3.08650326867133,-1.,-2.12975158752407));
#50351=CARTESIAN_POINT('Ctrl Pts',(-3.08650326867133,1.,-2.12975158752407));
#50352=CARTESIAN_POINT('Ctrl Pts',(-3.08690399991463,-1.,-2.1301541297946));
#50353=CARTESIAN_POINT('Ctrl Pts',(-3.08690399991463,1.,-2.1301541297946));
#50354=CARTESIAN_POINT('Ctrl Pts',(-3.08831615620074,-1.,-2.13116819908542));
#50355=CARTESIAN_POINT('Ctrl Pts',(-3.08831615620074,1.,-2.13116819908542));
#50356=CARTESIAN_POINT('Ctrl Pts',(-3.09151235281963,-1.,-2.13321032560893));
#50357=CARTESIAN_POINT('Ctrl Pts',(-3.09151235281963,1.,-2.13321032560893));
#50358=CARTESIAN_POINT('Ctrl Pts',(-3.0960450242104,-1.,-2.13596538661048));
#50359=CARTESIAN_POINT('Ctrl Pts',(-3.0960450242104,1.,-2.13596538661048));
#50360=CARTESIAN_POINT('Ctrl Pts',(-3.10171267391049,-1.,-2.13930228863751));
#50361=CARTESIAN_POINT('Ctrl Pts',(-3.10171267391049,1.,-2.13930228863751));
#50362=CARTESIAN_POINT('Ctrl Pts',(-3.10821808668859,-1.,-2.14302815601973));
#50363=CARTESIAN_POINT('Ctrl Pts',(-3.10821808668859,1.,-2.14302815601973));
#50364=CARTESIAN_POINT('Ctrl Pts',(-3.11522827016855,-1.,-2.14692798457532));
#50365=CARTESIAN_POINT('Ctrl Pts',(-3.11522827016855,1.,-2.14692798457532));
#50366=CARTESIAN_POINT('Ctrl Pts',(-3.12242318151938,-1.,-2.15079698090585));
#50367=CARTESIAN_POINT('Ctrl Pts',(-3.12242318151938,1.,-2.15079698090585));
#50368=CARTESIAN_POINT('Ctrl Pts',(-3.12954386795646,-1.,-2.1544724138292));
#50369=CARTESIAN_POINT('Ctrl Pts',(-3.12954386795646,1.,-2.1544724138292));
#50370=CARTESIAN_POINT('Ctrl Pts',(-3.13645356563038,-1.,-2.15787423530676));
#50371=CARTESIAN_POINT('Ctrl Pts',(-3.13645356563038,1.,-2.15787423530676));
#50372=CARTESIAN_POINT('Ctrl Pts',(-3.14314440427022,-1.,-2.16100905914435));
#50373=CARTESIAN_POINT('Ctrl Pts',(-3.14314440427022,1.,-2.16100905914435));
#50374=CARTESIAN_POINT('Ctrl Pts',(-3.14968624389054,-1.,-2.16393520288072));
#50375=CARTESIAN_POINT('Ctrl Pts',(-3.14968624389054,1.,-2.16393520288072));
#50376=CARTESIAN_POINT('Ctrl Pts',(-3.15618975593656,-1.,-2.1667372844769));
#50377=CARTESIAN_POINT('Ctrl Pts',(-3.15618975593656,1.,-2.1667372844769));
#50378=CARTESIAN_POINT('Ctrl Pts',(-3.16276685102972,-1.,-2.16949910801219));
#50379=CARTESIAN_POINT('Ctrl Pts',(-3.16276685102972,1.,-2.16949910801219));
#50380=CARTESIAN_POINT('Ctrl Pts',(-3.16948480019497,-1.,-2.17227212063817));
#50381=CARTESIAN_POINT('Ctrl Pts',(-3.16948480019497,1.,-2.17227212063817));
#50382=CARTESIAN_POINT('Ctrl Pts',(-3.17635032802523,-1.,-2.17506466903694));
#50383=CARTESIAN_POINT('Ctrl Pts',(-3.17635032802523,1.,-2.17506466903694));
#50384=CARTESIAN_POINT('Ctrl Pts',(-3.18333474627807,-1.,-2.17785968847142));
#50385=CARTESIAN_POINT('Ctrl Pts',(-3.18333474627807,1.,-2.17785968847142));
#50386=CARTESIAN_POINT('Ctrl Pts',(-3.19038924261573,-1.,-2.18062558031778));
#50387=CARTESIAN_POINT('Ctrl Pts',(-3.19038924261573,1.,-2.18062558031778));
#50388=CARTESIAN_POINT('Ctrl Pts',(-3.19746293740411,-1.,-2.18332898656602));
#50389=CARTESIAN_POINT('Ctrl Pts',(-3.19746293740411,1.,-2.18332898656602));
#50390=CARTESIAN_POINT('Ctrl Pts',(-3.20452259717976,-1.,-2.18594876115934));
#50391=CARTESIAN_POINT('Ctrl Pts',(-3.20452259717976,1.,-2.18594876115934));
#50392=CARTESIAN_POINT('Ctrl Pts',(-3.21156188355769,-1.,-2.18848253363901));
#50393=CARTESIAN_POINT('Ctrl Pts',(-3.21156188355769,1.,-2.18848253363901));
#50394=CARTESIAN_POINT('Ctrl Pts',(-3.21859043114095,-1.,-2.19093901948667));
#50395=CARTESIAN_POINT('Ctrl Pts',(-3.21859043114095,1.,-2.19093901948667));
#50396=CARTESIAN_POINT('Ctrl Pts',(-3.22562734221646,-1.,-2.19333345123538));
#50397=CARTESIAN_POINT('Ctrl Pts',(-3.22562734221646,1.,-2.19333345123538));
#50398=CARTESIAN_POINT('Ctrl Pts',(-3.23269332296933,-1.,-2.19568204933168));
#50399=CARTESIAN_POINT('Ctrl Pts',(-3.23269332296933,1.,-2.19568204933168));
#50400=CARTESIAN_POINT('Ctrl Pts',(-3.23980245361308,-1.,-2.19799623693253));
#50401=CARTESIAN_POINT('Ctrl Pts',(-3.23980245361308,1.,-2.19799623693253));
#50402=CARTESIAN_POINT('Ctrl Pts',(-3.24695715874338,-1.,-2.20027910880981));
#50403=CARTESIAN_POINT('Ctrl Pts',(-3.24695715874338,1.,-2.20027910880981));
#50404=CARTESIAN_POINT('Ctrl Pts',(-3.25415277957775,-1.,-2.20252866491545));
#50405=CARTESIAN_POINT('Ctrl Pts',(-3.25415277957775,1.,-2.20252866491545));
#50406=CARTESIAN_POINT('Ctrl Pts',(-3.26138036637705,-1.,-2.20473979048678));
#50407=CARTESIAN_POINT('Ctrl Pts',(-3.26138036637705,1.,-2.20473979048678));
#50408=CARTESIAN_POINT('Ctrl Pts',(-3.26863006136782,-1.,-2.20690665217743));
#50409=CARTESIAN_POINT('Ctrl Pts',(-3.26863006136782,1.,-2.20690665217743));
#50410=CARTESIAN_POINT('Ctrl Pts',(-3.2758944800554,-1.,-2.2090250941743));
#50411=CARTESIAN_POINT('Ctrl Pts',(-3.2758944800554,1.,-2.2090250941743));
#50412=CARTESIAN_POINT('Ctrl Pts',(-3.28317133333131,-1.,-2.21109449750641));
#50413=CARTESIAN_POINT('Ctrl Pts',(-3.28317133333131,1.,-2.21109449750641));
#50414=CARTESIAN_POINT('Ctrl Pts',(-3.29046159238343,-1.,-2.21311648827391));
#50415=CARTESIAN_POINT('Ctrl Pts',(-3.29046159238343,1.,-2.21311648827391));
#50416=CARTESIAN_POINT('Ctrl Pts',(-3.29776825193159,-1.,-2.21509406923368));
#50417=CARTESIAN_POINT('Ctrl Pts',(-3.29776825193159,1.,-2.21509406923368));
#50418=CARTESIAN_POINT('Ctrl Pts',(-3.30509487819569,-1.,-2.21703059947836));
#50419=CARTESIAN_POINT('Ctrl Pts',(-3.30509487819569,1.,-2.21703059947836));
#50420=CARTESIAN_POINT('Ctrl Pts',(-3.31244421655666,-1.,-2.21892881679086));
#50421=CARTESIAN_POINT('Ctrl Pts',(-3.31244421655666,1.,-2.21892881679086));
#50422=CARTESIAN_POINT('Ctrl Pts',(-3.31981686778022,-1.,-2.22078990842776));
#50423=CARTESIAN_POINT('Ctrl Pts',(-3.31981686778022,1.,-2.22078990842776));
#50424=CARTESIAN_POINT('Ctrl Pts',(-3.3272119632604,-1.,-2.22261398879635));
#50425=CARTESIAN_POINT('Ctrl Pts',(-3.3272119632604,1.,-2.22261398879635));
#50426=CARTESIAN_POINT('Ctrl Pts',(-3.33462772849598,-1.,-2.22440049878511));
#50427=CARTESIAN_POINT('Ctrl Pts',(-3.33462772849598,1.,-2.22440049878511));
#50428=CARTESIAN_POINT('Ctrl Pts',(-3.34206209449375,-1.,-2.22614863918047));
#50429=CARTESIAN_POINT('Ctrl Pts',(-3.34206209449375,1.,-2.22614863918047));
#50430=CARTESIAN_POINT('Ctrl Pts',(-3.34951327111096,-1.,-2.22785777756576));
#50431=CARTESIAN_POINT('Ctrl Pts',(-3.34951327111096,1.,-2.22785777756576));
#50432=CARTESIAN_POINT('Ctrl Pts',(-3.35698038165483,-1.,-2.22952789880982));
#50433=CARTESIAN_POINT('Ctrl Pts',(-3.35698038165483,1.,-2.22952789880982));
#50434=CARTESIAN_POINT('Ctrl Pts',(-3.36446325227848,-1.,-2.23115945849739));
#50435=CARTESIAN_POINT('Ctrl Pts',(-3.36446325227848,1.,-2.23115945849739));
#50436=CARTESIAN_POINT('Ctrl Pts',(-3.37196214349304,-1.,-2.23275319569221));
#50437=CARTESIAN_POINT('Ctrl Pts',(-3.37196214349304,1.,-2.23275319569221));
#50438=CARTESIAN_POINT('Ctrl Pts',(-3.37947749555632,-1.,-2.23430995599561));
#50439=CARTESIAN_POINT('Ctrl Pts',(-3.37947749555632,1.,-2.23430995599561));
#50440=CARTESIAN_POINT('Ctrl Pts',(-3.38700968549563,-1.,-2.23583052276308));
#50441=CARTESIAN_POINT('Ctrl Pts',(-3.38700968549563,1.,-2.23583052276308));
#50442=CARTESIAN_POINT('Ctrl Pts',(-3.39455873448189,-1.,-2.23731541452791));
#50443=CARTESIAN_POINT('Ctrl Pts',(-3.39455873448189,1.,-2.23731541452791));
#50444=CARTESIAN_POINT('Ctrl Pts',(-3.40212434705647,-1.,-2.2387649112415));
#50445=CARTESIAN_POINT('Ctrl Pts',(-3.40212434705647,1.,-2.2387649112415));
#50446=CARTESIAN_POINT('Ctrl Pts',(-3.40970604190328,-1.,-2.24017914395289));
#50447=CARTESIAN_POINT('Ctrl Pts',(-3.40970604190328,1.,-2.24017914395289));
#50448=CARTESIAN_POINT('Ctrl Pts',(-3.41730325539172,-1.,-2.24155816587844));
#50449=CARTESIAN_POINT('Ctrl Pts',(-3.41730325539172,1.,-2.24155816587844));
#50450=CARTESIAN_POINT('Ctrl Pts',(-3.42491544683008,-1.,-2.24290202531101));
#50451=CARTESIAN_POINT('Ctrl Pts',(-3.42491544683008,1.,-2.24290202531101));
#50452=CARTESIAN_POINT('Ctrl Pts',(-3.43254222614803,-1.,-2.24421085338727));
#50453=CARTESIAN_POINT('Ctrl Pts',(-3.43254222614803,1.,-2.24421085338727));
#50454=CARTESIAN_POINT('Ctrl Pts',(-3.4401833646032,-1.,-2.24548487526022));
#50455=CARTESIAN_POINT('Ctrl Pts',(-3.4401833646032,1.,-2.24548487526022));
#50456=CARTESIAN_POINT('Ctrl Pts',(-3.44783872863151,-1.,-2.2467243706995));
#50457=CARTESIAN_POINT('Ctrl Pts',(-3.44783872863151,1.,-2.2467243706995));
#50458=CARTESIAN_POINT('Ctrl Pts',(-3.45550823512049,-1.,-2.2479296496077));
#50459=CARTESIAN_POINT('Ctrl Pts',(-3.45550823512049,1.,-2.2479296496077));
#50460=CARTESIAN_POINT('Ctrl Pts',(-3.46319180177573,-1.,-2.2491010234604));
#50461=CARTESIAN_POINT('Ctrl Pts',(-3.46319180177573,1.,-2.2491010234604));
#50462=CARTESIAN_POINT('Ctrl Pts',(-3.47088928979888,-1.,-2.25023877475942));
#50463=CARTESIAN_POINT('Ctrl Pts',(-3.47088928979888,1.,-2.25023877475942));
#50464=CARTESIAN_POINT('Ctrl Pts',(-3.47860048448691,-1.,-2.25134314238687));
#50465=CARTESIAN_POINT('Ctrl Pts',(-3.47860048448691,1.,-2.25134314238687));
#50466=CARTESIAN_POINT('Ctrl Pts',(-3.48632513240961,-1.,-2.25241433138695));
#50467=CARTESIAN_POINT('Ctrl Pts',(-3.48632513240961,1.,-2.25241433138695));
#50468=CARTESIAN_POINT('Ctrl Pts',(-3.49406296494791,-1.,-2.2534525170976));
#50469=CARTESIAN_POINT('Ctrl Pts',(-3.49406296494791,1.,-2.2534525170976));
#50470=CARTESIAN_POINT('Ctrl Pts',(-3.50181372617971,-1.,-2.25445785151868));
#50471=CARTESIAN_POINT('Ctrl Pts',(-3.50181372617971,1.,-2.25445785151868));
#50472=CARTESIAN_POINT('Ctrl Pts',(-3.50957720117341,-1.,-2.25543046979799));
#50473=CARTESIAN_POINT('Ctrl Pts',(-3.50957720117341,1.,-2.25543046979799));
#50474=CARTESIAN_POINT('Ctrl Pts',(-3.51735323667612,-1.,-2.25637049455044));
#50475=CARTESIAN_POINT('Ctrl Pts',(-3.51735323667612,1.,-2.25637049455044));
#50476=CARTESIAN_POINT('Ctrl Pts',(-3.52514172847711,-1.,-2.25727802940898));
#50477=CARTESIAN_POINT('Ctrl Pts',(-3.52514172847711,1.,-2.25727802940898));
#50478=CARTESIAN_POINT('Ctrl Pts',(-3.53138243688262,-1.,-2.25797812950104));
#50479=CARTESIAN_POINT('Ctrl Pts',(-3.53138243688262,1.,-2.25797812950104));
#50480=CARTESIAN_POINT('Ctrl Pts',(-3.53606853162228,-1.,-2.25848864343951));
#50481=CARTESIAN_POINT('Ctrl Pts',(-3.53606853162228,1.,-2.25848864343951));
#50482=CARTESIAN_POINT('Ctrl Pts',(-3.53919506647335,-1.,-2.2588225169468));
#50483=CARTESIAN_POINT('Ctrl Pts',(-3.53919506647335,1.,-2.2588225169468));
#50484=CARTESIAN_POINT('Ctrl Pts',(-3.54075895182139,-1.,-2.25898783642071));
#50485=CARTESIAN_POINT('Ctrl Pts',(-3.54075895182139,1.,-2.25898783642071));
#50486=CARTESIAN_POINT('',(-3.08655633322212,1.,-2.1297112484669));
#50487=CARTESIAN_POINT('Ctrl Pts',(-3.08655633322212,-1.,-2.1297112484669));
#50488=CARTESIAN_POINT('Ctrl Pts',(-3.08655633322212,-0.666666666666667,
-2.1297112484669));
#50489=CARTESIAN_POINT('Ctrl Pts',(-3.08655633322212,-0.333333333333333,
-2.1297112484669));
#50490=CARTESIAN_POINT('Ctrl Pts',(-3.08655633322212,0.333333333333333,
-2.1297112484669));
#50491=CARTESIAN_POINT('Ctrl Pts',(-3.08655633322212,0.666666666666667,
-2.1297112484669));
#50492=CARTESIAN_POINT('Ctrl Pts',(-3.08655633322212,1.,-2.1297112484669));
#50493=CARTESIAN_POINT('',(-3.54075895182139,1.,-2.25898783642071));
#50494=CARTESIAN_POINT('',(-3.54075895182139,0.,-2.25898783642071));
#50495=CARTESIAN_POINT('Ctrl Pts',(-3.08655633322211,1.,-2.1297112484669));
#50496=CARTESIAN_POINT('Ctrl Pts',(-3.08657131089497,1.,-2.1297578506149));
#50497=CARTESIAN_POINT('Ctrl Pts',(-3.08668447250322,1.,-2.12991938762374));
#50498=CARTESIAN_POINT('Ctrl Pts',(-3.08717896996098,1.,-2.13034980480424));
#50499=CARTESIAN_POINT('Ctrl Pts',(-3.08855597949761,1.,-2.13132142793017));
#50500=CARTESIAN_POINT('Ctrl Pts',(-3.09151235281963,1.,-2.13321032560893));
#50501=CARTESIAN_POINT('Ctrl Pts',(-3.0960450242104,1.,-2.13596538661048));
#50502=CARTESIAN_POINT('Ctrl Pts',(-3.10171267391049,1.,-2.13930228863751));
#50503=CARTESIAN_POINT('Ctrl Pts',(-3.10821808668859,1.,-2.14302815601973));
#50504=CARTESIAN_POINT('Ctrl Pts',(-3.11522827016855,1.,-2.14692798457532));
#50505=CARTESIAN_POINT('Ctrl Pts',(-3.12242318151938,1.,-2.15079698090585));
#50506=CARTESIAN_POINT('Ctrl Pts',(-3.12954386795646,1.,-2.1544724138292));
#50507=CARTESIAN_POINT('Ctrl Pts',(-3.13645356563038,1.,-2.15787423530676));
#50508=CARTESIAN_POINT('Ctrl Pts',(-3.14314440427022,1.,-2.16100905914435));
#50509=CARTESIAN_POINT('Ctrl Pts',(-3.14968624389054,1.,-2.16393520288072));
#50510=CARTESIAN_POINT('Ctrl Pts',(-3.15618975593656,1.,-2.1667372844769));
#50511=CARTESIAN_POINT('Ctrl Pts',(-3.16276685102972,1.,-2.16949910801219));
#50512=CARTESIAN_POINT('Ctrl Pts',(-3.16948480019497,1.,-2.17227212063817));
#50513=CARTESIAN_POINT('Ctrl Pts',(-3.17635032802523,1.,-2.17506466903694));
#50514=CARTESIAN_POINT('Ctrl Pts',(-3.18333474627807,1.,-2.17785968847142));
#50515=CARTESIAN_POINT('Ctrl Pts',(-3.19038924261573,1.,-2.18062558031778));
#50516=CARTESIAN_POINT('Ctrl Pts',(-3.19746293740411,1.,-2.18332898656602));
#50517=CARTESIAN_POINT('Ctrl Pts',(-3.20452259717976,1.,-2.18594876115934));
#50518=CARTESIAN_POINT('Ctrl Pts',(-3.21156188355769,1.,-2.18848253363901));
#50519=CARTESIAN_POINT('Ctrl Pts',(-3.21859043114095,1.,-2.19093901948667));
#50520=CARTESIAN_POINT('Ctrl Pts',(-3.22562734221646,1.,-2.19333345123538));
#50521=CARTESIAN_POINT('Ctrl Pts',(-3.23269332296933,1.,-2.19568204933168));
#50522=CARTESIAN_POINT('Ctrl Pts',(-3.23980245361308,1.,-2.19799623693253));
#50523=CARTESIAN_POINT('Ctrl Pts',(-3.24695715874338,1.,-2.20027910880981));
#50524=CARTESIAN_POINT('Ctrl Pts',(-3.25415277957775,1.,-2.20252866491545));
#50525=CARTESIAN_POINT('Ctrl Pts',(-3.26138036637705,1.,-2.20473979048678));
#50526=CARTESIAN_POINT('Ctrl Pts',(-3.26863006136782,1.,-2.20690665217743));
#50527=CARTESIAN_POINT('Ctrl Pts',(-3.2758944800554,1.,-2.2090250941743));
#50528=CARTESIAN_POINT('Ctrl Pts',(-3.28317133333131,1.,-2.21109449750641));
#50529=CARTESIAN_POINT('Ctrl Pts',(-3.29046159238343,1.,-2.21311648827391));
#50530=CARTESIAN_POINT('Ctrl Pts',(-3.29776825193159,1.,-2.21509406923368));
#50531=CARTESIAN_POINT('Ctrl Pts',(-3.30509487819569,1.,-2.21703059947836));
#50532=CARTESIAN_POINT('Ctrl Pts',(-3.31244421655666,1.,-2.21892881679086));
#50533=CARTESIAN_POINT('Ctrl Pts',(-3.31981686778022,1.,-2.22078990842776));
#50534=CARTESIAN_POINT('Ctrl Pts',(-3.3272119632604,1.,-2.22261398879635));
#50535=CARTESIAN_POINT('Ctrl Pts',(-3.33462772849598,1.,-2.22440049878511));
#50536=CARTESIAN_POINT('Ctrl Pts',(-3.34206209449375,1.,-2.22614863918047));
#50537=CARTESIAN_POINT('Ctrl Pts',(-3.34951327111096,1.,-2.22785777756576));
#50538=CARTESIAN_POINT('Ctrl Pts',(-3.35698038165483,1.,-2.22952789880982));
#50539=CARTESIAN_POINT('Ctrl Pts',(-3.36446325227848,1.,-2.23115945849739));
#50540=CARTESIAN_POINT('Ctrl Pts',(-3.37196214349304,1.,-2.23275319569221));
#50541=CARTESIAN_POINT('Ctrl Pts',(-3.37947749555632,1.,-2.23430995599561));
#50542=CARTESIAN_POINT('Ctrl Pts',(-3.38700968549563,1.,-2.23583052276308));
#50543=CARTESIAN_POINT('Ctrl Pts',(-3.39455873448189,1.,-2.23731541452791));
#50544=CARTESIAN_POINT('Ctrl Pts',(-3.40212434705647,1.,-2.2387649112415));
#50545=CARTESIAN_POINT('Ctrl Pts',(-3.40970604190328,1.,-2.24017914395289));
#50546=CARTESIAN_POINT('Ctrl Pts',(-3.41730325539172,1.,-2.24155816587844));
#50547=CARTESIAN_POINT('Ctrl Pts',(-3.42491544683008,1.,-2.24290202531101));
#50548=CARTESIAN_POINT('Ctrl Pts',(-3.43254222614803,1.,-2.24421085338727));
#50549=CARTESIAN_POINT('Ctrl Pts',(-3.4401833646032,1.,-2.24548487526022));
#50550=CARTESIAN_POINT('Ctrl Pts',(-3.44783872863151,1.,-2.2467243706995));
#50551=CARTESIAN_POINT('Ctrl Pts',(-3.45550823512049,1.,-2.2479296496077));
#50552=CARTESIAN_POINT('Ctrl Pts',(-3.46319180177573,1.,-2.2491010234604));
#50553=CARTESIAN_POINT('Ctrl Pts',(-3.47088928979888,1.,-2.25023877475942));
#50554=CARTESIAN_POINT('Ctrl Pts',(-3.47860048448691,1.,-2.25134314238687));
#50555=CARTESIAN_POINT('Ctrl Pts',(-3.48632513240961,1.,-2.25241433138695));
#50556=CARTESIAN_POINT('Ctrl Pts',(-3.49406296494791,1.,-2.2534525170976));
#50557=CARTESIAN_POINT('Ctrl Pts',(-3.50181372617971,1.,-2.25445785151868));
#50558=CARTESIAN_POINT('Ctrl Pts',(-3.50957720117341,1.,-2.25543046979799));
#50559=CARTESIAN_POINT('Ctrl Pts',(-3.51735323667612,1.,-2.25637049455044));
#50560=CARTESIAN_POINT('Ctrl Pts',(-3.52514172847711,1.,-2.25727802940898));
#50561=CARTESIAN_POINT('Ctrl Pts',(-3.53138243688262,1.,-2.25797812950104));
#50562=CARTESIAN_POINT('Ctrl Pts',(-3.53606853162228,1.,-2.25848864343951));
#50563=CARTESIAN_POINT('Ctrl Pts',(-3.53919506647335,1.,-2.2588225169468));
#50564=CARTESIAN_POINT('Ctrl Pts',(-3.54075895182139,1.,-2.25898783642071));
#50565=CARTESIAN_POINT('Origin',(-3.54075895182139,0.,-2.25898783642071));
#50566=CARTESIAN_POINT('',(-3.62024382630768,1.,-2.12928030988903));
#50567=CARTESIAN_POINT('Origin',(0.,0.,0.));
#50568=CARTESIAN_POINT('',(-2.97927412174388,1.,-2.27737254473378));
#50569=CARTESIAN_POINT('Origin',(0.,1.,0.));
#50570=CARTESIAN_POINT('Ctrl Pts',(-2.97927412174388,1.,-2.27737254473378));
#50571=CARTESIAN_POINT('Ctrl Pts',(-2.97927412174388,0.666666666666667,
-2.27737254473378));
#50572=CARTESIAN_POINT('Ctrl Pts',(-2.97927412174388,0.333333333333333,
-2.27737254473378));
#50573=CARTESIAN_POINT('Ctrl Pts',(-2.97927412174388,-0.333333333333333,
-2.27737254473378));
#50574=CARTESIAN_POINT('Ctrl Pts',(-2.97927412174388,-0.666666666666667,
-2.27737254473378));
#50575=CARTESIAN_POINT('Ctrl Pts',(-2.97927412174388,-1.,-2.27737254473378));
#50576=CARTESIAN_POINT('Ctrl Pts',(-3.24257979115744,-1.,-2.66939624221984));
#50577=CARTESIAN_POINT('Ctrl Pts',(-3.24257979115744,1.,-2.66939624221984));
#50578=CARTESIAN_POINT('Ctrl Pts',(-3.24193929584813,-1.,-2.66795998539861));
#50579=CARTESIAN_POINT('Ctrl Pts',(-3.24193929584813,1.,-2.66795998539861));
#50580=CARTESIAN_POINT('Ctrl Pts',(-3.24065561087681,-1.,-2.66508964664767));
#50581=CARTESIAN_POINT('Ctrl Pts',(-3.24065561087681,1.,-2.66508964664767));
#50582=CARTESIAN_POINT('Ctrl Pts',(-3.23872200036311,-1.,-2.6607906631973));
#50583=CARTESIAN_POINT('Ctrl Pts',(-3.23872200036311,1.,-2.6607906631973));
#50584=CARTESIAN_POINT('Ctrl Pts',(-3.23612768065687,-1.,-2.6550717396303));
#50585=CARTESIAN_POINT('Ctrl Pts',(-3.23612768065687,1.,-2.6550717396303));
#50586=CARTESIAN_POINT('Ctrl Pts',(-3.23285778738558,-1.,-2.64794488744246));
#50587=CARTESIAN_POINT('Ctrl Pts',(-3.23285778738558,1.,-2.64794488744246));
#50588=CARTESIAN_POINT('Ctrl Pts',(-3.2295608435934,-1.,-2.64083992182478));
#50589=CARTESIAN_POINT('Ctrl Pts',(-3.2295608435934,1.,-2.64083992182478));
#50590=CARTESIAN_POINT('Ctrl Pts',(-3.22623678292539,-1.,-2.63375697391438));
#50591=CARTESIAN_POINT('Ctrl Pts',(-3.22623678292539,1.,-2.63375697391438));
#50592=CARTESIAN_POINT('Ctrl Pts',(-3.222885536128,-1.,-2.62669622735548));
#50593=CARTESIAN_POINT('Ctrl Pts',(-3.222885536128,1.,-2.62669622735548));
#50594=CARTESIAN_POINT('Ctrl Pts',(-3.21950704108654,-1.,-2.61965792832396));
#50595=CARTESIAN_POINT('Ctrl Pts',(-3.21950704108654,1.,-2.61965792832396));
#50596=CARTESIAN_POINT('Ctrl Pts',(-3.21610123232465,-1.,-2.61264236718662));
#50597=CARTESIAN_POINT('Ctrl Pts',(-3.21610123232465,1.,-2.61264236718662));
#50598=CARTESIAN_POINT('Ctrl Pts',(-3.21266802609297,-1.,-2.60564985359699));
#50599=CARTESIAN_POINT('Ctrl Pts',(-3.21266802609297,1.,-2.60564985359699));
#50600=CARTESIAN_POINT('Ctrl Pts',(-3.2092073056959,-1.,-2.59868069194267));
#50601=CARTESIAN_POINT('Ctrl Pts',(-3.2092073056959,1.,-2.59868069194267));
#50602=CARTESIAN_POINT('Ctrl Pts',(-3.20571891028879,-1.,-2.59173516023605));
#50603=CARTESIAN_POINT('Ctrl Pts',(-3.20571891028879,1.,-2.59173516023605));
#50604=CARTESIAN_POINT('Ctrl Pts',(-3.20220261408685,-1.,-2.58481347777953));
#50605=CARTESIAN_POINT('Ctrl Pts',(-3.20220261408685,1.,-2.58481347777953));
#50606=CARTESIAN_POINT('Ctrl Pts',(-3.19865814628955,-1.,-2.577915819091));
#50607=CARTESIAN_POINT('Ctrl Pts',(-3.19865814628955,1.,-2.577915819091));
#50608=CARTESIAN_POINT('Ctrl Pts',(-3.19508523784548,-1.,-2.57104235898053));
#50609=CARTESIAN_POINT('Ctrl Pts',(-3.19508523784548,1.,-2.57104235898053));
#50610=CARTESIAN_POINT('Ctrl Pts',(-3.19148366395201,-1.,-2.56419331092909));
#50611=CARTESIAN_POINT('Ctrl Pts',(-3.19148366395201,1.,-2.56419331092909));
#50612=CARTESIAN_POINT('Ctrl Pts',(-3.1878532811617,-1.,-2.55736896206016));
#50613=CARTESIAN_POINT('Ctrl Pts',(-3.1878532811617,1.,-2.55736896206016));
#50614=CARTESIAN_POINT('Ctrl Pts',(-3.18419408529482,-1.,-2.55056972387638));
#50615=CARTESIAN_POINT('Ctrl Pts',(-3.18419408529482,1.,-2.55056972387638));
#50616=CARTESIAN_POINT('Ctrl Pts',(-3.18050619750515,-1.,-2.54379612552948));
#50617=CARTESIAN_POINT('Ctrl Pts',(-3.18050619750515,1.,-2.54379612552948));
#50618=CARTESIAN_POINT('Ctrl Pts',(-3.17678974135225,-1.,-2.53704871950871));
#50619=CARTESIAN_POINT('Ctrl Pts',(-3.17678974135225,1.,-2.53704871950871));
#50620=CARTESIAN_POINT('Ctrl Pts',(-3.17304474093574,-1.,-2.5303280040691));
#50621=CARTESIAN_POINT('Ctrl Pts',(-3.17304474093574,1.,-2.5303280040691));
#50622=CARTESIAN_POINT('Ctrl Pts',(-3.16927102130751,-1.,-2.523634346718));
#50623=CARTESIAN_POINT('Ctrl Pts',(-3.16927102130751,1.,-2.523634346718));
#50624=CARTESIAN_POINT('Ctrl Pts',(-3.16546808277069,-1.,-2.51696788755615));
#50625=CARTESIAN_POINT('Ctrl Pts',(-3.16546808277069,1.,-2.51696788755615));
#50626=CARTESIAN_POINT('Ctrl Pts',(-3.16163506380211,-1.,-2.51032851007939));
#50627=CARTESIAN_POINT('Ctrl Pts',(-3.16163506380211,1.,-2.51032851007939));
#50628=CARTESIAN_POINT('Ctrl Pts',(-3.15777102413998,-1.,-2.50371605688287));
#50629=CARTESIAN_POINT('Ctrl Pts',(-3.15777102413998,1.,-2.50371605688287));
#50630=CARTESIAN_POINT('Ctrl Pts',(-3.15387518039064,-1.,-2.49713050858911));
#50631=CARTESIAN_POINT('Ctrl Pts',(-3.15387518039064,1.,-2.49713050858911));
#50632=CARTESIAN_POINT('Ctrl Pts',(-3.14994715298903,-1.,-2.49057217131985));
#50633=CARTESIAN_POINT('Ctrl Pts',(-3.14994715298903,1.,-2.49057217131985));
#50634=CARTESIAN_POINT('Ctrl Pts',(-3.1459872272388,-1.,-2.48404187418376));
#50635=CARTESIAN_POINT('Ctrl Pts',(-3.1459872272388,1.,-2.48404187418376));
#50636=CARTESIAN_POINT('Ctrl Pts',(-3.14199655778845,-1.,-2.47754112428027));
#50637=CARTESIAN_POINT('Ctrl Pts',(-3.14199655778845,1.,-2.47754112428027));
#50638=CARTESIAN_POINT('Ctrl Pts',(-3.13797654408931,-1.,-2.47107164236827));
#50639=CARTESIAN_POINT('Ctrl Pts',(-3.13797654408931,1.,-2.47107164236827));
#50640=CARTESIAN_POINT('Ctrl Pts',(-3.13392826623902,-1.,-2.4646349433237));
#50641=CARTESIAN_POINT('Ctrl Pts',(-3.13392826623902,1.,-2.4646349433237));
#50642=CARTESIAN_POINT('Ctrl Pts',(-3.12985188384372,-1.,-2.45823188859366));
#50643=CARTESIAN_POINT('Ctrl Pts',(-3.12985188384372,1.,-2.45823188859366));
#50644=CARTESIAN_POINT('Ctrl Pts',(-3.12574608210849,-1.,-2.45186227369848));
#50645=CARTESIAN_POINT('Ctrl Pts',(-3.12574608210849,1.,-2.45186227369848));
#50646=CARTESIAN_POINT('Ctrl Pts',(-3.12160740887768,-1.,-2.44552433364716));
#50647=CARTESIAN_POINT('Ctrl Pts',(-3.12160740887768,1.,-2.44552433364716));
#50648=CARTESIAN_POINT('Ctrl Pts',(-3.11743156744182,-1.,-2.43921571477975));
#50649=CARTESIAN_POINT('Ctrl Pts',(-3.11743156744182,1.,-2.43921571477975));
#50650=CARTESIAN_POINT('Ctrl Pts',(-3.11321477659012,-1.,-2.4329344968514));
#50651=CARTESIAN_POINT('Ctrl Pts',(-3.11321477659012,1.,-2.4329344968514));
#50652=CARTESIAN_POINT('Ctrl Pts',(-3.10895518969592,-1.,-2.42668025870013));
#50653=CARTESIAN_POINT('Ctrl Pts',(-3.10895518969592,1.,-2.42668025870013));
#50654=CARTESIAN_POINT('Ctrl Pts',(-3.10465410280902,-1.,-2.42045498612494));
#50655=CARTESIAN_POINT('Ctrl Pts',(-3.10465410280902,1.,-2.42045498612494));
#50656=CARTESIAN_POINT('Ctrl Pts',(-3.10031775027683,-1.,-2.41426441798067));
#50657=CARTESIAN_POINT('Ctrl Pts',(-3.10031775027683,1.,-2.41426441798067));
#50658=CARTESIAN_POINT('Ctrl Pts',(-3.09595472616093,-1.,-2.40811612696382));
#50659=CARTESIAN_POINT('Ctrl Pts',(-3.09595472616093,1.,-2.40811612696382));
#50660=CARTESIAN_POINT('Ctrl Pts',(-3.09157266051115,-1.,-2.40201704423352));
#50661=CARTESIAN_POINT('Ctrl Pts',(-3.09157266051115,1.,-2.40201704423352));
#50662=CARTESIAN_POINT('Ctrl Pts',(-3.08717489512919,-1.,-2.39597098250635));
#50663=CARTESIAN_POINT('Ctrl Pts',(-3.08717489512919,1.,-2.39597098250635));
#50664=CARTESIAN_POINT('Ctrl Pts',(-3.08275773747083,-1.,-2.38997659219192));
#50665=CARTESIAN_POINT('Ctrl Pts',(-3.08275773747083,1.,-2.38997659219192));
#50666=CARTESIAN_POINT('Ctrl Pts',(-3.07830597244301,-1.,-2.38402401216107));
#50667=CARTESIAN_POINT('Ctrl Pts',(-3.07830597244301,1.,-2.38402401216107));
#50668=CARTESIAN_POINT('Ctrl Pts',(-3.07379777492133,-1.,-2.37809856205524));
#50669=CARTESIAN_POINT('Ctrl Pts',(-3.07379777492133,1.,-2.37809856205524));
#50670=CARTESIAN_POINT('Ctrl Pts',(-3.06921275497472,-1.,-2.37218678163157));
#50671=CARTESIAN_POINT('Ctrl Pts',(-3.06921275497472,1.,-2.37218678163157));
#50672=CARTESIAN_POINT('Ctrl Pts',(-3.06453964643152,-1.,-2.36628220107001));
#50673=CARTESIAN_POINT('Ctrl Pts',(-3.06453964643152,1.,-2.36628220107001));
#50674=CARTESIAN_POINT('Ctrl Pts',(-3.05978266240056,-1.,-2.36039011602084));
#50675=CARTESIAN_POINT('Ctrl Pts',(-3.05978266240056,1.,-2.36039011602084));
#50676=CARTESIAN_POINT('Ctrl Pts',(-3.05497218368188,-1.,-2.35453559889506));
#50677=CARTESIAN_POINT('Ctrl Pts',(-3.05497218368188,1.,-2.35453559889506));
#50678=CARTESIAN_POINT('Ctrl Pts',(-3.05015565829976,-1.,-2.34875673090816));
#50679=CARTESIAN_POINT('Ctrl Pts',(-3.05015565829976,1.,-2.34875673090816));
#50680=CARTESIAN_POINT('Ctrl Pts',(-3.04537822217311,-1.,-2.3430901708402));
#50681=CARTESIAN_POINT('Ctrl Pts',(-3.04537822217311,1.,-2.3430901708402));
#50682=CARTESIAN_POINT('Ctrl Pts',(-3.04066496998569,-1.,-2.33755792953726));
#50683=CARTESIAN_POINT('Ctrl Pts',(-3.04066496998569,1.,-2.33755792953726));
#50684=CARTESIAN_POINT('Ctrl Pts',(-3.03600588555765,-1.,-2.33215619079807));
#50685=CARTESIAN_POINT('Ctrl Pts',(-3.03600588555765,1.,-2.33215619079807));
#50686=CARTESIAN_POINT('Ctrl Pts',(-3.03133125185047,-1.,-2.32683687412027));
#50687=CARTESIAN_POINT('Ctrl Pts',(-3.03133125185047,1.,-2.32683687412027));
#50688=CARTESIAN_POINT('Ctrl Pts',(-3.02652678416478,-1.,-2.32151944306299));
#50689=CARTESIAN_POINT('Ctrl Pts',(-3.02652678416478,1.,-2.32151944306299));
#50690=CARTESIAN_POINT('Ctrl Pts',(-3.02147780668029,-1.,-2.31612479121528));
#50691=CARTESIAN_POINT('Ctrl Pts',(-3.02147780668029,1.,-2.31612479121528));
#50692=CARTESIAN_POINT('Ctrl Pts',(-3.01610726819019,-1.,-2.31060449886577));
#50693=CARTESIAN_POINT('Ctrl Pts',(-3.01610726819019,1.,-2.31060449886577));
#50694=CARTESIAN_POINT('Ctrl Pts',(-3.01041131063882,-1.,-2.30496809486528));
#50695=CARTESIAN_POINT('Ctrl Pts',(-3.01041131063882,1.,-2.30496809486528));
#50696=CARTESIAN_POINT('Ctrl Pts',(-3.00450832658822,-1.,-2.29932091315939));
#50697=CARTESIAN_POINT('Ctrl Pts',(-3.00450832658822,1.,-2.29932091315939));
#50698=CARTESIAN_POINT('Ctrl Pts',(-2.99863310340004,-1.,-2.29385894577999));
#50699=CARTESIAN_POINT('Ctrl Pts',(-2.99863310340004,1.,-2.29385894577999));
#50700=CARTESIAN_POINT('Ctrl Pts',(-2.9930793098434,-1.,-2.28882328690601));
#50701=CARTESIAN_POINT('Ctrl Pts',(-2.9930793098434,1.,-2.28882328690601));
#50702=CARTESIAN_POINT('Ctrl Pts',(-2.98815432734929,-1.,-2.28446419116036));
#50703=CARTESIAN_POINT('Ctrl Pts',(-2.98815432734929,1.,-2.28446419116036));
#50704=CARTESIAN_POINT('Ctrl Pts',(-2.98413343613858,-1.,-2.28100472516582));
#50705=CARTESIAN_POINT('Ctrl Pts',(-2.98413343613858,1.,-2.28100472516582));
#50706=CARTESIAN_POINT('Ctrl Pts',(-2.98120357932601,-1.,-2.2785960133424));
#50707=CARTESIAN_POINT('Ctrl Pts',(-2.98120357932601,1.,-2.2785960133424));
#50708=CARTESIAN_POINT('Ctrl Pts',(-2.97980276182744,-1.,-2.27756633754846));
#50709=CARTESIAN_POINT('Ctrl Pts',(-2.97980276182744,1.,-2.27756633754846));
#50710=CARTESIAN_POINT('Ctrl Pts',(-2.97929608861502,-1.,-2.27730961189188));
#50711=CARTESIAN_POINT('Ctrl Pts',(-2.97929608861502,1.,-2.27730961189188));
#50712=CARTESIAN_POINT('Ctrl Pts',(-2.97919987915565,-1.,-2.2773674298423));
#50713=CARTESIAN_POINT('Ctrl Pts',(-2.97919987915565,1.,-2.2773674298423));
#50714=CARTESIAN_POINT('Ctrl Pts',(-2.97921217251145,-1.,-2.27745358485296));
#50715=CARTESIAN_POINT('Ctrl Pts',(-2.97921217251145,1.,-2.27745358485296));
#50716=CARTESIAN_POINT('',(-3.24257979115744,1.,-2.66939624221984));
#50717=CARTESIAN_POINT('Ctrl Pts',(-3.24257979115744,1.,-2.66939624221984));
#50718=CARTESIAN_POINT('Ctrl Pts',(-3.24193929584813,1.,-2.66795998539861));
#50719=CARTESIAN_POINT('Ctrl Pts',(-3.24065561087681,1.,-2.66508964664767));
#50720=CARTESIAN_POINT('Ctrl Pts',(-3.23872200036311,1.,-2.6607906631973));
#50721=CARTESIAN_POINT('Ctrl Pts',(-3.23612768065687,1.,-2.6550717396303));
#50722=CARTESIAN_POINT('Ctrl Pts',(-3.23285778738558,1.,-2.64794488744246));
#50723=CARTESIAN_POINT('Ctrl Pts',(-3.2295608435934,1.,-2.64083992182478));
#50724=CARTESIAN_POINT('Ctrl Pts',(-3.22623678292539,1.,-2.63375697391438));
#50725=CARTESIAN_POINT('Ctrl Pts',(-3.222885536128,1.,-2.62669622735548));
#50726=CARTESIAN_POINT('Ctrl Pts',(-3.21950704108654,1.,-2.61965792832396));
#50727=CARTESIAN_POINT('Ctrl Pts',(-3.21610123232465,1.,-2.61264236718662));
#50728=CARTESIAN_POINT('Ctrl Pts',(-3.21266802609297,1.,-2.60564985359699));
#50729=CARTESIAN_POINT('Ctrl Pts',(-3.2092073056959,1.,-2.59868069194267));
#50730=CARTESIAN_POINT('Ctrl Pts',(-3.20571891028879,1.,-2.59173516023605));
#50731=CARTESIAN_POINT('Ctrl Pts',(-3.20220261408685,1.,-2.58481347777953));
#50732=CARTESIAN_POINT('Ctrl Pts',(-3.19865814628955,1.,-2.577915819091));
#50733=CARTESIAN_POINT('Ctrl Pts',(-3.19508523784548,1.,-2.57104235898053));
#50734=CARTESIAN_POINT('Ctrl Pts',(-3.19148366395201,1.,-2.56419331092909));
#50735=CARTESIAN_POINT('Ctrl Pts',(-3.1878532811617,1.,-2.55736896206016));
#50736=CARTESIAN_POINT('Ctrl Pts',(-3.18419408529482,1.,-2.55056972387638));
#50737=CARTESIAN_POINT('Ctrl Pts',(-3.18050619750515,1.,-2.54379612552948));
#50738=CARTESIAN_POINT('Ctrl Pts',(-3.17678974135225,1.,-2.53704871950871));
#50739=CARTESIAN_POINT('Ctrl Pts',(-3.17304474093574,1.,-2.5303280040691));
#50740=CARTESIAN_POINT('Ctrl Pts',(-3.16927102130751,1.,-2.523634346718));
#50741=CARTESIAN_POINT('Ctrl Pts',(-3.16546808277069,1.,-2.51696788755615));
#50742=CARTESIAN_POINT('Ctrl Pts',(-3.16163506380211,1.,-2.51032851007939));
#50743=CARTESIAN_POINT('Ctrl Pts',(-3.15777102413998,1.,-2.50371605688287));
#50744=CARTESIAN_POINT('Ctrl Pts',(-3.15387518039064,1.,-2.49713050858911));
#50745=CARTESIAN_POINT('Ctrl Pts',(-3.14994715298903,1.,-2.49057217131985));
#50746=CARTESIAN_POINT('Ctrl Pts',(-3.1459872272388,1.,-2.48404187418376));
#50747=CARTESIAN_POINT('Ctrl Pts',(-3.14199655778845,1.,-2.47754112428027));
#50748=CARTESIAN_POINT('Ctrl Pts',(-3.13797654408931,1.,-2.47107164236827));
#50749=CARTESIAN_POINT('Ctrl Pts',(-3.13392826623902,1.,-2.4646349433237));
#50750=CARTESIAN_POINT('Ctrl Pts',(-3.12985188384372,1.,-2.45823188859366));
#50751=CARTESIAN_POINT('Ctrl Pts',(-3.12574608210849,1.,-2.45186227369848));
#50752=CARTESIAN_POINT('Ctrl Pts',(-3.12160740887768,1.,-2.44552433364716));
#50753=CARTESIAN_POINT('Ctrl Pts',(-3.11743156744182,1.,-2.43921571477975));
#50754=CARTESIAN_POINT('Ctrl Pts',(-3.11321477659012,1.,-2.4329344968514));
#50755=CARTESIAN_POINT('Ctrl Pts',(-3.10895518969592,1.,-2.42668025870013));
#50756=CARTESIAN_POINT('Ctrl Pts',(-3.10465410280902,1.,-2.42045498612494));
#50757=CARTESIAN_POINT('Ctrl Pts',(-3.10031775027683,1.,-2.41426441798067));
#50758=CARTESIAN_POINT('Ctrl Pts',(-3.09595472616093,1.,-2.40811612696382));
#50759=CARTESIAN_POINT('Ctrl Pts',(-3.09157266051115,1.,-2.40201704423352));
#50760=CARTESIAN_POINT('Ctrl Pts',(-3.08717489512919,1.,-2.39597098250635));
#50761=CARTESIAN_POINT('Ctrl Pts',(-3.08275773747083,1.,-2.38997659219192));
#50762=CARTESIAN_POINT('Ctrl Pts',(-3.07830597244301,1.,-2.38402401216107));
#50763=CARTESIAN_POINT('Ctrl Pts',(-3.07379777492133,1.,-2.37809856205524));
#50764=CARTESIAN_POINT('Ctrl Pts',(-3.06921275497472,1.,-2.37218678163157));
#50765=CARTESIAN_POINT('Ctrl Pts',(-3.06453964643152,1.,-2.36628220107001));
#50766=CARTESIAN_POINT('Ctrl Pts',(-3.05978266240056,1.,-2.36039011602084));
#50767=CARTESIAN_POINT('Ctrl Pts',(-3.05497218368188,1.,-2.35453559889506));
#50768=CARTESIAN_POINT('Ctrl Pts',(-3.05015565829976,1.,-2.34875673090816));
#50769=CARTESIAN_POINT('Ctrl Pts',(-3.04537822217311,1.,-2.3430901708402));
#50770=CARTESIAN_POINT('Ctrl Pts',(-3.04066496998569,1.,-2.33755792953726));
#50771=CARTESIAN_POINT('Ctrl Pts',(-3.03600588555765,1.,-2.33215619079807));
#50772=CARTESIAN_POINT('Ctrl Pts',(-3.03133125185047,1.,-2.32683687412027));
#50773=CARTESIAN_POINT('Ctrl Pts',(-3.02652678416478,1.,-2.32151944306299));
#50774=CARTESIAN_POINT('Ctrl Pts',(-3.02147780668029,1.,-2.31612479121528));
#50775=CARTESIAN_POINT('Ctrl Pts',(-3.01610726819019,1.,-2.31060449886577));
#50776=CARTESIAN_POINT('Ctrl Pts',(-3.01041131063882,1.,-2.30496809486528));
#50777=CARTESIAN_POINT('Ctrl Pts',(-3.00450832658822,1.,-2.29932091315939));
#50778=CARTESIAN_POINT('Ctrl Pts',(-2.99863310340004,1.,-2.29385894577999));
#50779=CARTESIAN_POINT('Ctrl Pts',(-2.9930793098434,1.,-2.28882328690601));
#50780=CARTESIAN_POINT('Ctrl Pts',(-2.98815432734929,1.,-2.28446419116036));
#50781=CARTESIAN_POINT('Ctrl Pts',(-2.98413343613858,1.,-2.28100472516582));
#50782=CARTESIAN_POINT('Ctrl Pts',(-2.98142341809623,1.,-2.27877674853833));
#50783=CARTESIAN_POINT('Ctrl Pts',(-2.98007383024333,1.,-2.27776738270369));
#50784=CARTESIAN_POINT('Ctrl Pts',(-2.97951167106106,1.,-2.27743009389704));
#50785=CARTESIAN_POINT('Ctrl Pts',(-2.97932307137589,1.,-2.27737238849212));
#50786=CARTESIAN_POINT('Ctrl Pts',(-2.97927412174388,1.,-2.27737254473378));
#50787=CARTESIAN_POINT('',(-3.24257979115744,0.,-2.66939624221984));
#50788=CARTESIAN_POINT('Ctrl Pts',(-2.71546581445404,-1.,-2.58626089374824));
#50789=CARTESIAN_POINT('Ctrl Pts',(-2.71546581445404,1.,-2.58626089374824));
#50790=CARTESIAN_POINT('Ctrl Pts',(-2.71537879705104,-1.,-2.58626222935803));
#50791=CARTESIAN_POINT('Ctrl Pts',(-2.71537879705104,1.,-2.58626222935803));
#50792=CARTESIAN_POINT('Ctrl Pts',(-2.71533674141254,-1.,-2.58636629904103));
#50793=CARTESIAN_POINT('Ctrl Pts',(-2.71533674141254,1.,-2.58636629904103));
#50794=CARTESIAN_POINT('Ctrl Pts',(-2.71566956750452,-1.,-2.5868265735259));
#50795=CARTESIAN_POINT('Ctrl Pts',(-2.71566956750452,1.,-2.5868265735259));
#50796=CARTESIAN_POINT('Ctrl Pts',(-2.71690570241638,-1.,-2.58804906785417));
#50797=CARTESIAN_POINT('Ctrl Pts',(-2.71690570241638,1.,-2.58804906785417));
#50798=CARTESIAN_POINT('Ctrl Pts',(-2.71974308958086,-1.,-2.59056604771971));
#50799=CARTESIAN_POINT('Ctrl Pts',(-2.71974308958086,1.,-2.59056604771971));
#50800=CARTESIAN_POINT('Ctrl Pts',(-2.72378896977134,-1.,-2.59399625537278));
#50801=CARTESIAN_POINT('Ctrl Pts',(-2.72378896977134,1.,-2.59399625537278));
#50802=CARTESIAN_POINT('Ctrl Pts',(-2.7288648348152,-1.,-2.59817869034746));
#50803=CARTESIAN_POINT('Ctrl Pts',(-2.7288648348152,1.,-2.59817869034746));
#50804=CARTESIAN_POINT('Ctrl Pts',(-2.73470730109615,-1.,-2.60287635688728));
#50805=CARTESIAN_POINT('Ctrl Pts',(-2.73470730109615,1.,-2.60287635688728));
#50806=CARTESIAN_POINT('Ctrl Pts',(-2.7410211099909,-1.,-2.60782480638448));
#50807=CARTESIAN_POINT('Ctrl Pts',(-2.7410211099909,1.,-2.60782480638448));
#50808=CARTESIAN_POINT('Ctrl Pts',(-2.74752219567252,-1.,-2.61277170105813));
#50809=CARTESIAN_POINT('Ctrl Pts',(-2.74752219567252,1.,-2.61277170105813));
#50810=CARTESIAN_POINT('Ctrl Pts',(-2.7539802502603,-1.,-2.61751580407667));
#50811=CARTESIAN_POINT('Ctrl Pts',(-2.7539802502603,1.,-2.61751580407667));
#50812=CARTESIAN_POINT('Ctrl Pts',(-2.76027271596686,-1.,-2.62195665834605));
#50813=CARTESIAN_POINT('Ctrl Pts',(-2.76027271596686,1.,-2.62195665834605));
#50814=CARTESIAN_POINT('Ctrl Pts',(-2.76639078479021,-1.,-2.62609956506355));
#50815=CARTESIAN_POINT('Ctrl Pts',(-2.76639078479021,1.,-2.62609956506355));
#50816=CARTESIAN_POINT('Ctrl Pts',(-2.77239433377921,-1.,-2.63001305229625));
#50817=CARTESIAN_POINT('Ctrl Pts',(-2.77239433377921,1.,-2.63001305229625));
#50818=CARTESIAN_POINT('Ctrl Pts',(-2.77837943466449,-1.,-2.63379800904599));
#50819=CARTESIAN_POINT('Ctrl Pts',(-2.77837943466449,1.,-2.63379800904599));
#50820=CARTESIAN_POINT('Ctrl Pts',(-2.78444351041571,-1.,-2.637554714303));
#50821=CARTESIAN_POINT('Ctrl Pts',(-2.78444351041571,1.,-2.637554714303));
#50822=CARTESIAN_POINT('Ctrl Pts',(-2.79064495573224,-1.,-2.64134450532584));
#50823=CARTESIAN_POINT('Ctrl Pts',(-2.79064495573224,1.,-2.64134450532584));
#50824=CARTESIAN_POINT('Ctrl Pts',(-2.79698910670736,-1.,-2.64517667799319));
#50825=CARTESIAN_POINT('Ctrl Pts',(-2.79698910670736,1.,-2.64517667799319));
#50826=CARTESIAN_POINT('Ctrl Pts',(-2.80345029781152,-1.,-2.64902988983337));
#50827=CARTESIAN_POINT('Ctrl Pts',(-2.80345029781152,1.,-2.64902988983337));
#50828=CARTESIAN_POINT('Ctrl Pts',(-2.80998526078165,-1.,-2.65286529532208));
#50829=CARTESIAN_POINT('Ctrl Pts',(-2.80998526078165,1.,-2.65286529532208));
#50830=CARTESIAN_POINT('Ctrl Pts',(-2.81654896073883,-1.,-2.65664198781344));
#50831=CARTESIAN_POINT('Ctrl Pts',(-2.81654896073883,1.,-2.65664198781344));
#50832=CARTESIAN_POINT('Ctrl Pts',(-2.82311188135078,-1.,-2.66033388273461));
#50833=CARTESIAN_POINT('Ctrl Pts',(-2.82311188135078,1.,-2.66033388273461));
#50834=CARTESIAN_POINT('Ctrl Pts',(-2.82966813308998,-1.,-2.6639376472693));
#50835=CARTESIAN_POINT('Ctrl Pts',(-2.82966813308998,1.,-2.6639376472693));
#50836=CARTESIAN_POINT('Ctrl Pts',(-2.83622586853982,-1.,-2.66746339678107));
#50837=CARTESIAN_POINT('Ctrl Pts',(-2.83622586853982,1.,-2.66746339678107));
#50838=CARTESIAN_POINT('Ctrl Pts',(-2.84280157191323,-1.,-2.67092916452125));
#50839=CARTESIAN_POINT('Ctrl Pts',(-2.84280157191323,1.,-2.67092916452125));
#50840=CARTESIAN_POINT('Ctrl Pts',(-2.84941315703092,-1.,-2.67435421039677));
#50841=CARTESIAN_POINT('Ctrl Pts',(-2.84941315703092,1.,-2.67435421039677));
#50842=CARTESIAN_POINT('Ctrl Pts',(-2.85607274378018,-1.,-2.67775201955724));
#50843=CARTESIAN_POINT('Ctrl Pts',(-2.85607274378018,1.,-2.67775201955724));
#50844=CARTESIAN_POINT('Ctrl Pts',(-2.86278224277689,-1.,-2.68112602796308));
#50845=CARTESIAN_POINT('Ctrl Pts',(-2.86278224277689,1.,-2.68112602796308));
#50846=CARTESIAN_POINT('Ctrl Pts',(-2.86953736547238,-1.,-2.68447353139599));
#50847=CARTESIAN_POINT('Ctrl Pts',(-2.86953736547238,1.,-2.68447353139599));
#50848=CARTESIAN_POINT('Ctrl Pts',(-2.8763300724388,-1.,-2.68778807801686));
#50849=CARTESIAN_POINT('Ctrl Pts',(-2.8763300724388,1.,-2.68778807801686));
#50850=CARTESIAN_POINT('Ctrl Pts',(-2.88315153980466,-1.,-2.69106236420198));
#50851=CARTESIAN_POINT('Ctrl Pts',(-2.88315153980466,1.,-2.69106236420198));
#50852=CARTESIAN_POINT('Ctrl Pts',(-2.88999512410309,-1.,-2.69429113011374));
#50853=CARTESIAN_POINT('Ctrl Pts',(-2.88999512410309,1.,-2.69429113011374));
#50854=CARTESIAN_POINT('Ctrl Pts',(-2.89685866123671,-1.,-2.69747340630625));
#50855=CARTESIAN_POINT('Ctrl Pts',(-2.89685866123671,1.,-2.69747340630625));
#50856=CARTESIAN_POINT('Ctrl Pts',(-2.90374285605838,-1.,-2.70061095078692));
#50857=CARTESIAN_POINT('Ctrl Pts',(-2.90374285605838,1.,-2.70061095078692));
#50858=CARTESIAN_POINT('Ctrl Pts',(-2.91065019668329,-1.,-2.70370719782113));
#50859=CARTESIAN_POINT('Ctrl Pts',(-2.91065019668329,1.,-2.70370719782113));
#50860=CARTESIAN_POINT('Ctrl Pts',(-2.91758367994737,-1.,-2.70676602302518));
#50861=CARTESIAN_POINT('Ctrl Pts',(-2.91758367994737,1.,-2.70676602302518));
#50862=CARTESIAN_POINT('Ctrl Pts',(-2.92454558914778,-1.,-2.70979055994754));
#50863=CARTESIAN_POINT('Ctrl Pts',(-2.92454558914778,1.,-2.70979055994754));
#50864=CARTESIAN_POINT('Ctrl Pts',(-2.93153633192595,-1.,-2.71278207520817));
#50865=CARTESIAN_POINT('Ctrl Pts',(-2.93153633192595,1.,-2.71278207520817));
#50866=CARTESIAN_POINT('Ctrl Pts',(-2.93855503247266,-1.,-2.7157405459259));
#50867=CARTESIAN_POINT('Ctrl Pts',(-2.93855503247266,1.,-2.7157405459259));
#50868=CARTESIAN_POINT('Ctrl Pts',(-2.94560002559806,-1.,-2.71866514227965));
#50869=CARTESIAN_POINT('Ctrl Pts',(-2.94560002559806,1.,-2.71866514227965));
#50870=CARTESIAN_POINT('Ctrl Pts',(-2.95266939280621,-1.,-2.72155475123364));
#50871=CARTESIAN_POINT('Ctrl Pts',(-2.95266939280621,1.,-2.72155475123364));
#50872=CARTESIAN_POINT('Ctrl Pts',(-2.95976146492576,-1.,-2.72440846811729));
#50873=CARTESIAN_POINT('Ctrl Pts',(-2.95976146492576,1.,-2.72440846811729));
#50874=CARTESIAN_POINT('Ctrl Pts',(-2.96687537842451,-1.,-2.72722614084076));
#50875=CARTESIAN_POINT('Ctrl Pts',(-2.96687537842451,1.,-2.72722614084076));
#50876=CARTESIAN_POINT('Ctrl Pts',(-2.97401089032677,-1.,-2.73000819218414));
#50877=CARTESIAN_POINT('Ctrl Pts',(-2.97401089032677,1.,-2.73000819218414));
#50878=CARTESIAN_POINT('Ctrl Pts',(-2.98116814232129,-1.,-2.73275539286497));
#50879=CARTESIAN_POINT('Ctrl Pts',(-2.98116814232129,1.,-2.73275539286497));
#50880=CARTESIAN_POINT('Ctrl Pts',(-2.9883474369644,-1.,-2.73546864694536));
#50881=CARTESIAN_POINT('Ctrl Pts',(-2.9883474369644,1.,-2.73546864694536));
#50882=CARTESIAN_POINT('Ctrl Pts',(-2.99554902409778,-1.,-2.73814878711641));
#50883=CARTESIAN_POINT('Ctrl Pts',(-2.99554902409778,1.,-2.73814878711641));
#50884=CARTESIAN_POINT('Ctrl Pts',(-3.00277284351521,-1.,-2.74079632883931));
#50885=CARTESIAN_POINT('Ctrl Pts',(-3.00277284351521,1.,-2.74079632883931));
#50886=CARTESIAN_POINT('Ctrl Pts',(-3.01001855960162,-1.,-2.74341150239887));
#50887=CARTESIAN_POINT('Ctrl Pts',(-3.01001855960162,1.,-2.74341150239887));
#50888=CARTESIAN_POINT('Ctrl Pts',(-3.01728567646611,-1.,-2.74599436193625));
#50889=CARTESIAN_POINT('Ctrl Pts',(-3.01728567646611,1.,-2.74599436193625));
#50890=CARTESIAN_POINT('Ctrl Pts',(-3.02457362909245,-1.,-2.7485448718414));
#50891=CARTESIAN_POINT('Ctrl Pts',(-3.02457362909245,1.,-2.7485448718414));
#50892=CARTESIAN_POINT('Ctrl Pts',(-3.03188187589107,-1.,-2.75106299522979));
#50893=CARTESIAN_POINT('Ctrl Pts',(-3.03188187589107,1.,-2.75106299522979));
#50894=CARTESIAN_POINT('Ctrl Pts',(-3.03921001107977,-1.,-2.75354880060314));
#50895=CARTESIAN_POINT('Ctrl Pts',(-3.03921001107977,1.,-2.75354880060314));
#50896=CARTESIAN_POINT('Ctrl Pts',(-3.04655777351067,-1.,-2.75600247455925));
#50897=CARTESIAN_POINT('Ctrl Pts',(-3.04655777351067,1.,-2.75600247455925));
#50898=CARTESIAN_POINT('Ctrl Pts',(-3.05392498749847,-1.,-2.75842427252931));
#50899=CARTESIAN_POINT('Ctrl Pts',(-3.05392498749847,1.,-2.75842427252931));
#50900=CARTESIAN_POINT('Ctrl Pts',(-3.06131152247454,-1.,-2.76081448759882));
#50901=CARTESIAN_POINT('Ctrl Pts',(-3.06131152247454,1.,-2.76081448759882));
#50902=CARTESIAN_POINT('Ctrl Pts',(-3.0687172484321,-1.,-2.76317341453493));
#50903=CARTESIAN_POINT('Ctrl Pts',(-3.0687172484321,1.,-2.76317341453493));
#50904=CARTESIAN_POINT('Ctrl Pts',(-3.07614198408862,-1.,-2.76550131064852));
#50905=CARTESIAN_POINT('Ctrl Pts',(-3.07614198408862,1.,-2.76550131064852));
#50906=CARTESIAN_POINT('Ctrl Pts',(-3.08358548001504,-1.,-2.76779837829373));
#50907=CARTESIAN_POINT('Ctrl Pts',(-3.08358548001504,1.,-2.76779837829373));
#50908=CARTESIAN_POINT('Ctrl Pts',(-3.09104745382531,-1.,-2.7700647803451));
#50909=CARTESIAN_POINT('Ctrl Pts',(-3.09104745382531,1.,-2.7700647803451));
#50910=CARTESIAN_POINT('Ctrl Pts',(-3.0985276127786,-1.,-2.77230064796057));
#50911=CARTESIAN_POINT('Ctrl Pts',(-3.0985276127786,1.,-2.77230064796057));
#50912=CARTESIAN_POINT('Ctrl Pts',(-3.10602568032564,-1.,-2.77450609123362));
#50913=CARTESIAN_POINT('Ctrl Pts',(-3.10602568032564,1.,-2.77450609123362));
#50914=CARTESIAN_POINT('Ctrl Pts',(-3.11354142303921,-1.,-2.77668121002545));
#50915=CARTESIAN_POINT('Ctrl Pts',(-3.11354142303921,1.,-2.77668121002545));
#50916=CARTESIAN_POINT('Ctrl Pts',(-3.12107467037201,-1.,-2.77882610146731));
#50917=CARTESIAN_POINT('Ctrl Pts',(-3.12107467037201,1.,-2.77882610146731));
#50918=CARTESIAN_POINT('Ctrl Pts',(-3.12862530318457,-1.,-2.78094085161413));
#50919=CARTESIAN_POINT('Ctrl Pts',(-3.12862530318457,1.,-2.78094085161413));
#50920=CARTESIAN_POINT('Ctrl Pts',(-3.13467965833037,-1.,-2.78260859419319));
#50921=CARTESIAN_POINT('Ctrl Pts',(-3.13467965833037,1.,-2.78260859419319));
#50922=CARTESIAN_POINT('Ctrl Pts',(-3.13922819749279,-1.,-2.78384588958165));
#50923=CARTESIAN_POINT('Ctrl Pts',(-3.13922819749279,1.,-2.78384588958165));
#50924=CARTESIAN_POINT('Ctrl Pts',(-3.14226401018816,-1.,-2.7846647503589));
#50925=CARTESIAN_POINT('Ctrl Pts',(-3.14226401018816,1.,-2.7846647503589));
#50926=CARTESIAN_POINT('Ctrl Pts',(-3.14378277984898,-1.,-2.78507268004356));
#50927=CARTESIAN_POINT('Ctrl Pts',(-3.14378277984898,1.,-2.78507268004356));
#50928=CARTESIAN_POINT('',(-2.71539546306948,1.,-2.58633475774921));
#50929=CARTESIAN_POINT('Ctrl Pts',(-2.71539546306948,-1.,-2.58633475774921));
#50930=CARTESIAN_POINT('Ctrl Pts',(-2.71539546306948,-0.666666666666667,
-2.58633475774921));
#50931=CARTESIAN_POINT('Ctrl Pts',(-2.71539546306948,-0.333333333333333,
-2.58633475774921));
#50932=CARTESIAN_POINT('Ctrl Pts',(-2.71539546306948,0.333333333333333,
-2.58633475774921));
#50933=CARTESIAN_POINT('Ctrl Pts',(-2.71539546306948,0.666666666666667,
-2.58633475774921));
#50934=CARTESIAN_POINT('Ctrl Pts',(-2.71539546306948,1.,-2.58633475774921));
#50935=CARTESIAN_POINT('',(-3.14378277984898,1.,-2.78507268004356));
#50936=CARTESIAN_POINT('',(-3.14378277984898,0.,-2.78507268004356));
#50937=CARTESIAN_POINT('Ctrl Pts',(-2.71539546306948,1.,-2.58633475774921));
#50938=CARTESIAN_POINT('Ctrl Pts',(-2.71540296616024,1.,-2.58638312917167));
#50939=CARTESIAN_POINT('Ctrl Pts',(-2.71548946460575,1.,-2.58656037976753));
#50940=CARTESIAN_POINT('Ctrl Pts',(-2.71591054189786,1.,-2.58706285424357));
#50941=CARTESIAN_POINT('Ctrl Pts',(-2.71711860281815,1.,-2.58823792682672));
#50942=CARTESIAN_POINT('Ctrl Pts',(-2.71974308958086,1.,-2.59056604771971));
#50943=CARTESIAN_POINT('Ctrl Pts',(-2.72378896977134,1.,-2.59399625537278));
#50944=CARTESIAN_POINT('Ctrl Pts',(-2.7288648348152,1.,-2.59817869034746));
#50945=CARTESIAN_POINT('Ctrl Pts',(-2.73470730109615,1.,-2.60287635688728));
#50946=CARTESIAN_POINT('Ctrl Pts',(-2.7410211099909,1.,-2.60782480638448));
#50947=CARTESIAN_POINT('Ctrl Pts',(-2.74752219567252,1.,-2.61277170105813));
#50948=CARTESIAN_POINT('Ctrl Pts',(-2.7539802502603,1.,-2.61751580407667));
#50949=CARTESIAN_POINT('Ctrl Pts',(-2.76027271596686,1.,-2.62195665834605));
#50950=CARTESIAN_POINT('Ctrl Pts',(-2.76639078479021,1.,-2.62609956506355));
#50951=CARTESIAN_POINT('Ctrl Pts',(-2.77239433377921,1.,-2.63001305229625));
#50952=CARTESIAN_POINT('Ctrl Pts',(-2.77837943466449,1.,-2.63379800904599));
#50953=CARTESIAN_POINT('Ctrl Pts',(-2.78444351041571,1.,-2.637554714303));
#50954=CARTESIAN_POINT('Ctrl Pts',(-2.79064495573224,1.,-2.64134450532584));
#50955=CARTESIAN_POINT('Ctrl Pts',(-2.79698910670736,1.,-2.64517667799319));
#50956=CARTESIAN_POINT('Ctrl Pts',(-2.80345029781152,1.,-2.64902988983337));
#50957=CARTESIAN_POINT('Ctrl Pts',(-2.80998526078165,1.,-2.65286529532208));
#50958=CARTESIAN_POINT('Ctrl Pts',(-2.81654896073883,1.,-2.65664198781344));
#50959=CARTESIAN_POINT('Ctrl Pts',(-2.82311188135078,1.,-2.66033388273461));
#50960=CARTESIAN_POINT('Ctrl Pts',(-2.82966813308998,1.,-2.6639376472693));
#50961=CARTESIAN_POINT('Ctrl Pts',(-2.83622586853982,1.,-2.66746339678107));
#50962=CARTESIAN_POINT('Ctrl Pts',(-2.84280157191323,1.,-2.67092916452125));
#50963=CARTESIAN_POINT('Ctrl Pts',(-2.84941315703092,1.,-2.67435421039677));
#50964=CARTESIAN_POINT('Ctrl Pts',(-2.85607274378018,1.,-2.67775201955724));
#50965=CARTESIAN_POINT('Ctrl Pts',(-2.86278224277689,1.,-2.68112602796308));
#50966=CARTESIAN_POINT('Ctrl Pts',(-2.86953736547238,1.,-2.68447353139599));
#50967=CARTESIAN_POINT('Ctrl Pts',(-2.8763300724388,1.,-2.68778807801686));
#50968=CARTESIAN_POINT('Ctrl Pts',(-2.88315153980466,1.,-2.69106236420198));
#50969=CARTESIAN_POINT('Ctrl Pts',(-2.88999512410309,1.,-2.69429113011374));
#50970=CARTESIAN_POINT('Ctrl Pts',(-2.89685866123671,1.,-2.69747340630625));
#50971=CARTESIAN_POINT('Ctrl Pts',(-2.90374285605838,1.,-2.70061095078692));
#50972=CARTESIAN_POINT('Ctrl Pts',(-2.91065019668329,1.,-2.70370719782113));
#50973=CARTESIAN_POINT('Ctrl Pts',(-2.91758367994737,1.,-2.70676602302518));
#50974=CARTESIAN_POINT('Ctrl Pts',(-2.92454558914778,1.,-2.70979055994754));
#50975=CARTESIAN_POINT('Ctrl Pts',(-2.93153633192595,1.,-2.71278207520817));
#50976=CARTESIAN_POINT('Ctrl Pts',(-2.93855503247266,1.,-2.7157405459259));
#50977=CARTESIAN_POINT('Ctrl Pts',(-2.94560002559806,1.,-2.71866514227965));
#50978=CARTESIAN_POINT('Ctrl Pts',(-2.95266939280621,1.,-2.72155475123364));
#50979=CARTESIAN_POINT('Ctrl Pts',(-2.95976146492576,1.,-2.72440846811729));
#50980=CARTESIAN_POINT('Ctrl Pts',(-2.96687537842451,1.,-2.72722614084076));
#50981=CARTESIAN_POINT('Ctrl Pts',(-2.97401089032677,1.,-2.73000819218414));
#50982=CARTESIAN_POINT('Ctrl Pts',(-2.98116814232129,1.,-2.73275539286497));
#50983=CARTESIAN_POINT('Ctrl Pts',(-2.9883474369644,1.,-2.73546864694536));
#50984=CARTESIAN_POINT('Ctrl Pts',(-2.99554902409778,1.,-2.73814878711641));
#50985=CARTESIAN_POINT('Ctrl Pts',(-3.00277284351521,1.,-2.74079632883931));
#50986=CARTESIAN_POINT('Ctrl Pts',(-3.01001855960162,1.,-2.74341150239887));
#50987=CARTESIAN_POINT('Ctrl Pts',(-3.01728567646611,1.,-2.74599436193625));
#50988=CARTESIAN_POINT('Ctrl Pts',(-3.02457362909245,1.,-2.7485448718414));
#50989=CARTESIAN_POINT('Ctrl Pts',(-3.03188187589107,1.,-2.75106299522979));
#50990=CARTESIAN_POINT('Ctrl Pts',(-3.03921001107977,1.,-2.75354880060314));
#50991=CARTESIAN_POINT('Ctrl Pts',(-3.04655777351067,1.,-2.75600247455925));
#50992=CARTESIAN_POINT('Ctrl Pts',(-3.05392498749847,1.,-2.75842427252931));
#50993=CARTESIAN_POINT('Ctrl Pts',(-3.06131152247454,1.,-2.76081448759882));
#50994=CARTESIAN_POINT('Ctrl Pts',(-3.0687172484321,1.,-2.76317341453493));
#50995=CARTESIAN_POINT('Ctrl Pts',(-3.07614198408862,1.,-2.76550131064852));
#50996=CARTESIAN_POINT('Ctrl Pts',(-3.08358548001504,1.,-2.76779837829373));
#50997=CARTESIAN_POINT('Ctrl Pts',(-3.09104745382531,1.,-2.7700647803451));
#50998=CARTESIAN_POINT('Ctrl Pts',(-3.0985276127786,1.,-2.77230064796057));
#50999=CARTESIAN_POINT('Ctrl Pts',(-3.10602568032564,1.,-2.77450609123362));
#51000=CARTESIAN_POINT('Ctrl Pts',(-3.11354142303921,1.,-2.77668121002545));
#51001=CARTESIAN_POINT('Ctrl Pts',(-3.12107467037201,1.,-2.77882610146731));
#51002=CARTESIAN_POINT('Ctrl Pts',(-3.12862530318457,1.,-2.78094085161413));
#51003=CARTESIAN_POINT('Ctrl Pts',(-3.13467965833037,1.,-2.78260859419319));
#51004=CARTESIAN_POINT('Ctrl Pts',(-3.13922819749279,1.,-2.78384588958165));
#51005=CARTESIAN_POINT('Ctrl Pts',(-3.14226401018816,1.,-2.7846647503589));
#51006=CARTESIAN_POINT('Ctrl Pts',(-3.14378277984898,1.,-2.78507268004356));
#51007=CARTESIAN_POINT('Origin',(-3.14378277984898,0.,-2.78507268004356));
#51008=CARTESIAN_POINT('',(-3.24257979115744,1.,-2.66939624221984));
#51009=CARTESIAN_POINT('Origin',(0.,0.,0.));
#51010=CARTESIAN_POINT('',(-2.58633475775051,1.,-2.71539546306824));
#51011=CARTESIAN_POINT('Origin',(0.,1.,0.));
#51012=CARTESIAN_POINT('Ctrl Pts',(-2.58633475775051,1.,-2.71539546306824));
#51013=CARTESIAN_POINT('Ctrl Pts',(-2.58633475775051,0.666666666666667,
-2.71539546306824));
#51014=CARTESIAN_POINT('Ctrl Pts',(-2.58633475775051,0.333333333333333,
-2.71539546306824));
#51015=CARTESIAN_POINT('Ctrl Pts',(-2.58633475775051,-0.333333333333333,
-2.71539546306824));
#51016=CARTESIAN_POINT('Ctrl Pts',(-2.58633475775051,-0.666666666666667,
-2.71539546306824));
#51017=CARTESIAN_POINT('Ctrl Pts',(-2.58633475775051,-1.,-2.71539546306824));
#51018=CARTESIAN_POINT('Ctrl Pts',(-2.78507268004356,-1.,-3.14378277984898));
#51019=CARTESIAN_POINT('Ctrl Pts',(-2.78507268004356,1.,-3.14378277984898));
#51020=CARTESIAN_POINT('Ctrl Pts',(-2.78466475036183,-1.,-3.14226401019149));
#51021=CARTESIAN_POINT('Ctrl Pts',(-2.78466475036183,1.,-3.14226401019149));
#51022=CARTESIAN_POINT('Ctrl Pts',(-2.78384588958965,-1.,-3.13922819750185));
#51023=CARTESIAN_POINT('Ctrl Pts',(-2.78384588958965,1.,-3.13922819750185));
#51024=CARTESIAN_POINT('Ctrl Pts',(-2.78260859420629,-1.,-3.1346796583452));
#51025=CARTESIAN_POINT('Ctrl Pts',(-2.78260859420629,1.,-3.1346796583452));
#51026=CARTESIAN_POINT('Ctrl Pts',(-2.78094085162947,-1.,-3.12862530320194));
#51027=CARTESIAN_POINT('Ctrl Pts',(-2.78094085162947,1.,-3.12862530320194));
#51028=CARTESIAN_POINT('Ctrl Pts',(-2.77882610147986,-1.,-3.12107467038623));
#51029=CARTESIAN_POINT('Ctrl Pts',(-2.77882610147986,1.,-3.12107467038623));
#51030=CARTESIAN_POINT('Ctrl Pts',(-2.77668121003225,-1.,-3.11354142304692));
#51031=CARTESIAN_POINT('Ctrl Pts',(-2.77668121003225,1.,-3.11354142304692));
#51032=CARTESIAN_POINT('Ctrl Pts',(-2.7745060912343,-1.,-3.10602568032641));
#51033=CARTESIAN_POINT('Ctrl Pts',(-2.7745060912343,1.,-3.10602568032641));
#51034=CARTESIAN_POINT('Ctrl Pts',(-2.77230064795679,-1.,-3.09852761277432));
#51035=CARTESIAN_POINT('Ctrl Pts',(-2.77230064795679,1.,-3.09852761277432));
#51036=CARTESIAN_POINT('Ctrl Pts',(-2.77006478033937,-1.,-3.09104745381882));
#51037=CARTESIAN_POINT('Ctrl Pts',(-2.77006478033937,1.,-3.09104745381882));
#51038=CARTESIAN_POINT('Ctrl Pts',(-2.76779837828843,-1.,-3.08358548000904));
#51039=CARTESIAN_POINT('Ctrl Pts',(-2.76779837828843,1.,-3.08358548000904));
#51040=CARTESIAN_POINT('Ctrl Pts',(-2.76550131064522,-1.,-3.07614198408488));
#51041=CARTESIAN_POINT('Ctrl Pts',(-2.76550131064522,1.,-3.07614198408488));
#51042=CARTESIAN_POINT('Ctrl Pts',(-2.76317341453415,-1.,-3.06871724843121));
#51043=CARTESIAN_POINT('Ctrl Pts',(-2.76317341453415,1.,-3.06871724843121));
#51044=CARTESIAN_POINT('Ctrl Pts',(-2.76081448760011,-1.,-3.06131152247599));
#51045=CARTESIAN_POINT('Ctrl Pts',(-2.76081448760011,1.,-3.06131152247599));
#51046=CARTESIAN_POINT('Ctrl Pts',(-2.75842427253164,-1.,-3.05392498750112));
#51047=CARTESIAN_POINT('Ctrl Pts',(-2.75842427253164,1.,-3.05392498750112));
#51048=CARTESIAN_POINT('Ctrl Pts',(-2.7560024745616,-1.,-3.04655777351333));
#51049=CARTESIAN_POINT('Ctrl Pts',(-2.7560024745616,1.,-3.04655777351333));
#51050=CARTESIAN_POINT('Ctrl Pts',(-2.75354880060473,-1.,-3.03921001108158));
#51051=CARTESIAN_POINT('Ctrl Pts',(-2.75354880060473,1.,-3.03921001108158));
#51052=CARTESIAN_POINT('Ctrl Pts',(-2.75106299523032,-1.,-3.03188187589168));
#51053=CARTESIAN_POINT('Ctrl Pts',(-2.75106299523032,1.,-3.03188187589168));
#51054=CARTESIAN_POINT('Ctrl Pts',(-2.74854487184099,-1.,-3.02457362909199));
#51055=CARTESIAN_POINT('Ctrl Pts',(-2.74854487184099,1.,-3.02457362909199));
#51056=CARTESIAN_POINT('Ctrl Pts',(-2.74599436193528,-1.,-3.01728567646502));
#51057=CARTESIAN_POINT('Ctrl Pts',(-2.74599436193528,1.,-3.01728567646502));
#51058=CARTESIAN_POINT('Ctrl Pts',(-2.7434115023978,-1.,-3.01001855960041));
#51059=CARTESIAN_POINT('Ctrl Pts',(-2.7434115023978,1.,-3.01001855960041));
#51060=CARTESIAN_POINT('Ctrl Pts',(-2.74079632883852,-1.,-3.00277284351431));
#51061=CARTESIAN_POINT('Ctrl Pts',(-2.74079632883852,1.,-3.00277284351431));
#51062=CARTESIAN_POINT('Ctrl Pts',(-2.73814878711609,-1.,-2.99554902409741));
#51063=CARTESIAN_POINT('Ctrl Pts',(-2.73814878711609,1.,-2.99554902409741));
#51064=CARTESIAN_POINT('Ctrl Pts',(-2.73546864694548,-1.,-2.98834743696455));
#51065=CARTESIAN_POINT('Ctrl Pts',(-2.73546864694548,1.,-2.98834743696455));
#51066=CARTESIAN_POINT('Ctrl Pts',(-2.73275539286537,-1.,-2.98116814232175));
#51067=CARTESIAN_POINT('Ctrl Pts',(-2.73275539286537,1.,-2.98116814232175));
#51068=CARTESIAN_POINT('Ctrl Pts',(-2.7300081921846,-1.,-2.97401089032729));
#51069=CARTESIAN_POINT('Ctrl Pts',(-2.7300081921846,1.,-2.97401089032729));
#51070=CARTESIAN_POINT('Ctrl Pts',(-2.72722614084112,-1.,-2.96687537842492));
#51071=CARTESIAN_POINT('Ctrl Pts',(-2.72722614084112,1.,-2.96687537842492));
#51072=CARTESIAN_POINT('Ctrl Pts',(-2.72440846811745,-1.,-2.95976146492595));
#51073=CARTESIAN_POINT('Ctrl Pts',(-2.72440846811745,1.,-2.95976146492595));
#51074=CARTESIAN_POINT('Ctrl Pts',(-2.72155475123361,-1.,-2.95266939280617));
#51075=CARTESIAN_POINT('Ctrl Pts',(-2.72155475123361,1.,-2.95266939280617));
#51076=CARTESIAN_POINT('Ctrl Pts',(-2.71866514227952,-1.,-2.94560002559789));
#51077=CARTESIAN_POINT('Ctrl Pts',(-2.71866514227952,1.,-2.94560002559789));
#51078=CARTESIAN_POINT('Ctrl Pts',(-2.71574054592575,-1.,-2.93855503247248));
#51079=CARTESIAN_POINT('Ctrl Pts',(-2.71574054592575,1.,-2.93855503247248));
#51080=CARTESIAN_POINT('Ctrl Pts',(-2.71278207520807,-1.,-2.93153633192583));
#51081=CARTESIAN_POINT('Ctrl Pts',(-2.71278207520807,1.,-2.93153633192583));
#51082=CARTESIAN_POINT('Ctrl Pts',(-2.70979055994751,-1.,-2.92454558914774));
#51083=CARTESIAN_POINT('Ctrl Pts',(-2.70979055994751,1.,-2.92454558914774));
#51084=CARTESIAN_POINT('Ctrl Pts',(-2.70676602302518,-1.,-2.91758367994738));
#51085=CARTESIAN_POINT('Ctrl Pts',(-2.70676602302518,1.,-2.91758367994738));
#51086=CARTESIAN_POINT('Ctrl Pts',(-2.70370719782114,-1.,-2.91065019668331));
#51087=CARTESIAN_POINT('Ctrl Pts',(-2.70370719782114,1.,-2.91065019668331));
#51088=CARTESIAN_POINT('Ctrl Pts',(-2.70061095078692,-1.,-2.90374285605839));
#51089=CARTESIAN_POINT('Ctrl Pts',(-2.70061095078692,1.,-2.90374285605839));
#51090=CARTESIAN_POINT('Ctrl Pts',(-2.69747340630621,-1.,-2.89685866123668));
#51091=CARTESIAN_POINT('Ctrl Pts',(-2.69747340630621,1.,-2.89685866123668));
#51092=CARTESIAN_POINT('Ctrl Pts',(-2.69429113011369,-1.,-2.88999512410304));
#51093=CARTESIAN_POINT('Ctrl Pts',(-2.69429113011369,1.,-2.88999512410304));
#51094=CARTESIAN_POINT('Ctrl Pts',(-2.69106236420197,-1.,-2.88315153980464));
#51095=CARTESIAN_POINT('Ctrl Pts',(-2.69106236420197,1.,-2.88315153980464));
#51096=CARTESIAN_POINT('Ctrl Pts',(-2.68778807801691,-1.,-2.87633007243885));
#51097=CARTESIAN_POINT('Ctrl Pts',(-2.68778807801691,1.,-2.87633007243885));
#51098=CARTESIAN_POINT('Ctrl Pts',(-2.68447353139611,-1.,-2.8695373654725));
#51099=CARTESIAN_POINT('Ctrl Pts',(-2.68447353139611,1.,-2.8695373654725));
#51100=CARTESIAN_POINT('Ctrl Pts',(-2.68112602796323,-1.,-2.86278224277705));
#51101=CARTESIAN_POINT('Ctrl Pts',(-2.68112602796323,1.,-2.86278224277705));
#51102=CARTESIAN_POINT('Ctrl Pts',(-2.67775201955736,-1.,-2.85607274378031));
#51103=CARTESIAN_POINT('Ctrl Pts',(-2.67775201955736,1.,-2.85607274378031));
#51104=CARTESIAN_POINT('Ctrl Pts',(-2.67435421039682,-1.,-2.84941315703096));
#51105=CARTESIAN_POINT('Ctrl Pts',(-2.67435421039682,1.,-2.84941315703096));
#51106=CARTESIAN_POINT('Ctrl Pts',(-2.67092916452117,-1.,-2.84280157191314));
#51107=CARTESIAN_POINT('Ctrl Pts',(-2.67092916452117,1.,-2.84280157191314));
#51108=CARTESIAN_POINT('Ctrl Pts',(-2.66746339678085,-1.,-2.8362258685396));
#51109=CARTESIAN_POINT('Ctrl Pts',(-2.66746339678085,1.,-2.8362258685396));
#51110=CARTESIAN_POINT('Ctrl Pts',(-2.66393764726902,-1.,-2.82966813308969));
#51111=CARTESIAN_POINT('Ctrl Pts',(-2.66393764726902,1.,-2.82966813308969));
#51112=CARTESIAN_POINT('Ctrl Pts',(-2.66033388273437,-1.,-2.82311188135053));
#51113=CARTESIAN_POINT('Ctrl Pts',(-2.66033388273437,1.,-2.82311188135053));
#51114=CARTESIAN_POINT('Ctrl Pts',(-2.65664198781335,-1.,-2.81654896073874));
#51115=CARTESIAN_POINT('Ctrl Pts',(-2.65664198781335,1.,-2.81654896073874));
#51116=CARTESIAN_POINT('Ctrl Pts',(-2.65286529532221,-1.,-2.80998526078179));
#51117=CARTESIAN_POINT('Ctrl Pts',(-2.65286529532221,1.,-2.80998526078179));
#51118=CARTESIAN_POINT('Ctrl Pts',(-2.64902988983373,-1.,-2.80345029781191));
#51119=CARTESIAN_POINT('Ctrl Pts',(-2.64902988983373,1.,-2.80345029781191));
#51120=CARTESIAN_POINT('Ctrl Pts',(-2.6451766779937,-1.,-2.7969891067079));
#51121=CARTESIAN_POINT('Ctrl Pts',(-2.6451766779937,1.,-2.7969891067079));
#51122=CARTESIAN_POINT('Ctrl Pts',(-2.64134450532632,-1.,-2.79064495573275));
#51123=CARTESIAN_POINT('Ctrl Pts',(-2.64134450532632,1.,-2.79064495573275));
#51124=CARTESIAN_POINT('Ctrl Pts',(-2.63755471430322,-1.,-2.78444351041594));
#51125=CARTESIAN_POINT('Ctrl Pts',(-2.63755471430322,1.,-2.78444351041594));
#51126=CARTESIAN_POINT('Ctrl Pts',(-2.63379800904575,-1.,-2.77837943466423));
#51127=CARTESIAN_POINT('Ctrl Pts',(-2.63379800904575,1.,-2.77837943466423));
#51128=CARTESIAN_POINT('Ctrl Pts',(-2.63001305229548,-1.,-2.77239433377839));
#51129=CARTESIAN_POINT('Ctrl Pts',(-2.63001305229548,1.,-2.77239433377839));
#51130=CARTESIAN_POINT('Ctrl Pts',(-2.6260995650624,-1.,-2.76639078478898));
#51131=CARTESIAN_POINT('Ctrl Pts',(-2.6260995650624,1.,-2.76639078478898));
#51132=CARTESIAN_POINT('Ctrl Pts',(-2.62195665834491,-1.,-2.76027271596564));
#51133=CARTESIAN_POINT('Ctrl Pts',(-2.62195665834491,1.,-2.76027271596564));
#51134=CARTESIAN_POINT('Ctrl Pts',(-2.61751580407608,-1.,-2.75398025025967));
#51135=CARTESIAN_POINT('Ctrl Pts',(-2.61751580407608,1.,-2.75398025025967));
#51136=CARTESIAN_POINT('Ctrl Pts',(-2.61277170105864,-1.,-2.74752219567307));
#51137=CARTESIAN_POINT('Ctrl Pts',(-2.61277170105864,1.,-2.74752219567307));
#51138=CARTESIAN_POINT('Ctrl Pts',(-2.60782480638629,-1.,-2.74102110999284));
#51139=CARTESIAN_POINT('Ctrl Pts',(-2.60782480638629,1.,-2.74102110999284));
#51140=CARTESIAN_POINT('Ctrl Pts',(-2.60287635689,-1.,-2.73470730109906));
#51141=CARTESIAN_POINT('Ctrl Pts',(-2.60287635689,1.,-2.73470730109906));
#51142=CARTESIAN_POINT('Ctrl Pts',(-2.5981786903501,-1.,-2.72886483481804));
#51143=CARTESIAN_POINT('Ctrl Pts',(-2.5981786903501,1.,-2.72886483481804));
#51144=CARTESIAN_POINT('Ctrl Pts',(-2.59399625537407,-1.,-2.72378896977273));
#51145=CARTESIAN_POINT('Ctrl Pts',(-2.59399625537407,1.,-2.72378896977273));
#51146=CARTESIAN_POINT('Ctrl Pts',(-2.59056604771863,-1.,-2.7197430895797));
#51147=CARTESIAN_POINT('Ctrl Pts',(-2.59056604771863,1.,-2.7197430895797));
#51148=CARTESIAN_POINT('Ctrl Pts',(-2.58804906785078,-1.,-2.71690570241274));
#51149=CARTESIAN_POINT('Ctrl Pts',(-2.58804906785078,1.,-2.71690570241274));
#51150=CARTESIAN_POINT('Ctrl Pts',(-2.58682657352212,-1.,-2.71566956750046));
#51151=CARTESIAN_POINT('Ctrl Pts',(-2.58682657352212,1.,-2.71566956750046));
#51152=CARTESIAN_POINT('Ctrl Pts',(-2.58636629903847,-1.,-2.71533674140979));
#51153=CARTESIAN_POINT('Ctrl Pts',(-2.58636629903847,1.,-2.71533674140979));
#51154=CARTESIAN_POINT('Ctrl Pts',(-2.58626222935706,-1.,-2.71537879705));
#51155=CARTESIAN_POINT('Ctrl Pts',(-2.58626222935706,1.,-2.71537879705));
#51156=CARTESIAN_POINT('Ctrl Pts',(-2.58626089374824,-1.,-2.71546581445404));
#51157=CARTESIAN_POINT('Ctrl Pts',(-2.58626089374824,1.,-2.71546581445404));
#51158=CARTESIAN_POINT('',(-2.78507268004356,1.,-3.14378277984898));
#51159=CARTESIAN_POINT('Ctrl Pts',(-2.78507268004356,1.,-3.14378277984898));
#51160=CARTESIAN_POINT('Ctrl Pts',(-2.78466475036183,1.,-3.14226401019149));
#51161=CARTESIAN_POINT('Ctrl Pts',(-2.78384588958965,1.,-3.13922819750185));
#51162=CARTESIAN_POINT('Ctrl Pts',(-2.78260859420629,1.,-3.1346796583452));
#51163=CARTESIAN_POINT('Ctrl Pts',(-2.78094085162947,1.,-3.12862530320194));
#51164=CARTESIAN_POINT('Ctrl Pts',(-2.77882610147986,1.,-3.12107467038623));
#51165=CARTESIAN_POINT('Ctrl Pts',(-2.77668121003225,1.,-3.11354142304692));
#51166=CARTESIAN_POINT('Ctrl Pts',(-2.7745060912343,1.,-3.10602568032641));
#51167=CARTESIAN_POINT('Ctrl Pts',(-2.77230064795679,1.,-3.09852761277432));
#51168=CARTESIAN_POINT('Ctrl Pts',(-2.77006478033937,1.,-3.09104745381882));
#51169=CARTESIAN_POINT('Ctrl Pts',(-2.76779837828843,1.,-3.08358548000904));
#51170=CARTESIAN_POINT('Ctrl Pts',(-2.76550131064522,1.,-3.07614198408488));
#51171=CARTESIAN_POINT('Ctrl Pts',(-2.76317341453415,1.,-3.06871724843121));
#51172=CARTESIAN_POINT('Ctrl Pts',(-2.76081448760011,1.,-3.06131152247599));
#51173=CARTESIAN_POINT('Ctrl Pts',(-2.75842427253164,1.,-3.05392498750112));
#51174=CARTESIAN_POINT('Ctrl Pts',(-2.7560024745616,1.,-3.04655777351333));
#51175=CARTESIAN_POINT('Ctrl Pts',(-2.75354880060473,1.,-3.03921001108158));
#51176=CARTESIAN_POINT('Ctrl Pts',(-2.75106299523032,1.,-3.03188187589168));
#51177=CARTESIAN_POINT('Ctrl Pts',(-2.74854487184099,1.,-3.02457362909199));
#51178=CARTESIAN_POINT('Ctrl Pts',(-2.74599436193528,1.,-3.01728567646502));
#51179=CARTESIAN_POINT('Ctrl Pts',(-2.7434115023978,1.,-3.01001855960041));
#51180=CARTESIAN_POINT('Ctrl Pts',(-2.74079632883852,1.,-3.00277284351431));
#51181=CARTESIAN_POINT('Ctrl Pts',(-2.73814878711609,1.,-2.99554902409741));
#51182=CARTESIAN_POINT('Ctrl Pts',(-2.73546864694548,1.,-2.98834743696455));
#51183=CARTESIAN_POINT('Ctrl Pts',(-2.73275539286537,1.,-2.98116814232175));
#51184=CARTESIAN_POINT('Ctrl Pts',(-2.7300081921846,1.,-2.97401089032729));
#51185=CARTESIAN_POINT('Ctrl Pts',(-2.72722614084112,1.,-2.96687537842492));
#51186=CARTESIAN_POINT('Ctrl Pts',(-2.72440846811745,1.,-2.95976146492595));
#51187=CARTESIAN_POINT('Ctrl Pts',(-2.72155475123361,1.,-2.95266939280617));
#51188=CARTESIAN_POINT('Ctrl Pts',(-2.71866514227952,1.,-2.94560002559789));
#51189=CARTESIAN_POINT('Ctrl Pts',(-2.71574054592575,1.,-2.93855503247248));
#51190=CARTESIAN_POINT('Ctrl Pts',(-2.71278207520807,1.,-2.93153633192583));
#51191=CARTESIAN_POINT('Ctrl Pts',(-2.70979055994751,1.,-2.92454558914774));
#51192=CARTESIAN_POINT('Ctrl Pts',(-2.70676602302518,1.,-2.91758367994738));
#51193=CARTESIAN_POINT('Ctrl Pts',(-2.70370719782114,1.,-2.91065019668331));
#51194=CARTESIAN_POINT('Ctrl Pts',(-2.70061095078692,1.,-2.90374285605839));
#51195=CARTESIAN_POINT('Ctrl Pts',(-2.69747340630621,1.,-2.89685866123668));
#51196=CARTESIAN_POINT('Ctrl Pts',(-2.69429113011369,1.,-2.88999512410304));
#51197=CARTESIAN_POINT('Ctrl Pts',(-2.69106236420197,1.,-2.88315153980464));
#51198=CARTESIAN_POINT('Ctrl Pts',(-2.68778807801691,1.,-2.87633007243885));
#51199=CARTESIAN_POINT('Ctrl Pts',(-2.68447353139611,1.,-2.8695373654725));
#51200=CARTESIAN_POINT('Ctrl Pts',(-2.68112602796323,1.,-2.86278224277705));
#51201=CARTESIAN_POINT('Ctrl Pts',(-2.67775201955736,1.,-2.85607274378031));
#51202=CARTESIAN_POINT('Ctrl Pts',(-2.67435421039682,1.,-2.84941315703096));
#51203=CARTESIAN_POINT('Ctrl Pts',(-2.67092916452117,1.,-2.84280157191314));
#51204=CARTESIAN_POINT('Ctrl Pts',(-2.66746339678085,1.,-2.8362258685396));
#51205=CARTESIAN_POINT('Ctrl Pts',(-2.66393764726902,1.,-2.82966813308969));
#51206=CARTESIAN_POINT('Ctrl Pts',(-2.66033388273437,1.,-2.82311188135053));
#51207=CARTESIAN_POINT('Ctrl Pts',(-2.65664198781335,1.,-2.81654896073874));
#51208=CARTESIAN_POINT('Ctrl Pts',(-2.65286529532221,1.,-2.80998526078179));
#51209=CARTESIAN_POINT('Ctrl Pts',(-2.64902988983373,1.,-2.80345029781191));
#51210=CARTESIAN_POINT('Ctrl Pts',(-2.6451766779937,1.,-2.7969891067079));
#51211=CARTESIAN_POINT('Ctrl Pts',(-2.64134450532632,1.,-2.79064495573275));
#51212=CARTESIAN_POINT('Ctrl Pts',(-2.63755471430322,1.,-2.78444351041594));
#51213=CARTESIAN_POINT('Ctrl Pts',(-2.63379800904575,1.,-2.77837943466423));
#51214=CARTESIAN_POINT('Ctrl Pts',(-2.63001305229548,1.,-2.77239433377839));
#51215=CARTESIAN_POINT('Ctrl Pts',(-2.6260995650624,1.,-2.76639078478898));
#51216=CARTESIAN_POINT('Ctrl Pts',(-2.62195665834491,1.,-2.76027271596564));
#51217=CARTESIAN_POINT('Ctrl Pts',(-2.61751580407608,1.,-2.75398025025967));
#51218=CARTESIAN_POINT('Ctrl Pts',(-2.61277170105864,1.,-2.74752219567307));
#51219=CARTESIAN_POINT('Ctrl Pts',(-2.60782480638629,1.,-2.74102110999284));
#51220=CARTESIAN_POINT('Ctrl Pts',(-2.60287635689,1.,-2.73470730109906));
#51221=CARTESIAN_POINT('Ctrl Pts',(-2.5981786903501,1.,-2.72886483481804));
#51222=CARTESIAN_POINT('Ctrl Pts',(-2.59399625537407,1.,-2.72378896977273));
#51223=CARTESIAN_POINT('Ctrl Pts',(-2.59056604771863,1.,-2.7197430895797));
#51224=CARTESIAN_POINT('Ctrl Pts',(-2.58823792682724,1.,-2.7171186028189));
#51225=CARTESIAN_POINT('Ctrl Pts',(-2.58706285424469,1.,-2.71591054189884));
#51226=CARTESIAN_POINT('Ctrl Pts',(-2.58656037976884,1.,-2.71548946460616));
#51227=CARTESIAN_POINT('Ctrl Pts',(-2.58638312917291,1.,-2.71540296615967));
#51228=CARTESIAN_POINT('Ctrl Pts',(-2.58633475775051,1.,-2.71539546306824));
#51229=CARTESIAN_POINT('',(-2.78507268004356,0.,-3.14378277984898));
#51230=CARTESIAN_POINT('Ctrl Pts',(-2.27745358485296,-1.,-2.97921217251145));
#51231=CARTESIAN_POINT('Ctrl Pts',(-2.27745358485296,1.,-2.97921217251145));
#51232=CARTESIAN_POINT('Ctrl Pts',(-2.27736742984319,-1.,-2.97919987915679));
#51233=CARTESIAN_POINT('Ctrl Pts',(-2.27736742984319,1.,-2.97919987915679));
#51234=CARTESIAN_POINT('Ctrl Pts',(-2.2773096118942,-1.,-2.97929608861798));
#51235=CARTESIAN_POINT('Ctrl Pts',(-2.2773096118942,1.,-2.97929608861798));
#51236=CARTESIAN_POINT('Ctrl Pts',(-2.27756633755188,-1.,-2.97980276183181));
#51237=CARTESIAN_POINT('Ctrl Pts',(-2.27756633755188,1.,-2.97980276183181));
#51238=CARTESIAN_POINT('Ctrl Pts',(-2.27859601334547,-1.,-2.98120357932994));
#51239=CARTESIAN_POINT('Ctrl Pts',(-2.27859601334547,1.,-2.98120357932994));
#51240=CARTESIAN_POINT('Ctrl Pts',(-2.28100472516679,-1.,-2.98413343613983));
#51241=CARTESIAN_POINT('Ctrl Pts',(-2.28100472516679,1.,-2.98413343613983));
#51242=CARTESIAN_POINT('Ctrl Pts',(-2.28446419115919,-1.,-2.9881543273478));
#51243=CARTESIAN_POINT('Ctrl Pts',(-2.28446419115919,1.,-2.9881543273478));
#51244=CARTESIAN_POINT('Ctrl Pts',(-2.28882328690362,-1.,-2.99307930984034));
#51245=CARTESIAN_POINT('Ctrl Pts',(-2.28882328690362,1.,-2.99307930984034));
#51246=CARTESIAN_POINT('Ctrl Pts',(-2.29385894577754,-1.,-2.99863310339691));
#51247=CARTESIAN_POINT('Ctrl Pts',(-2.29385894577754,1.,-2.99863310339691));
#51248=CARTESIAN_POINT('Ctrl Pts',(-2.29932091315775,-1.,-3.00450832658613));
#51249=CARTESIAN_POINT('Ctrl Pts',(-2.29932091315775,1.,-3.00450832658613));
#51250=CARTESIAN_POINT('Ctrl Pts',(-2.30496809486482,-1.,-3.01041131063823));
#51251=CARTESIAN_POINT('Ctrl Pts',(-2.30496809486482,1.,-3.01041131063823));
#51252=CARTESIAN_POINT('Ctrl Pts',(-2.31060449886629,-1.,-3.01610726819086));
#51253=CARTESIAN_POINT('Ctrl Pts',(-2.31060449886629,1.,-3.01610726819086));
#51254=CARTESIAN_POINT('Ctrl Pts',(-2.31612479121631,-1.,-3.02147780668161));
#51255=CARTESIAN_POINT('Ctrl Pts',(-2.31612479121631,1.,-3.02147780668161));
#51256=CARTESIAN_POINT('Ctrl Pts',(-2.32151944306402,-1.,-3.02652678416611));
#51257=CARTESIAN_POINT('Ctrl Pts',(-2.32151944306402,1.,-3.02652678416611));
#51258=CARTESIAN_POINT('Ctrl Pts',(-2.32683687412097,-1.,-3.03133125185136));
#51259=CARTESIAN_POINT('Ctrl Pts',(-2.32683687412097,1.,-3.03133125185136));
#51260=CARTESIAN_POINT('Ctrl Pts',(-2.33215619079829,-1.,-3.03600588555793));
#51261=CARTESIAN_POINT('Ctrl Pts',(-2.33215619079829,1.,-3.03600588555793));
#51262=CARTESIAN_POINT('Ctrl Pts',(-2.33755792953706,-1.,-3.04066496998544));
#51263=CARTESIAN_POINT('Ctrl Pts',(-2.33755792953706,1.,-3.04066496998544));
#51264=CARTESIAN_POINT('Ctrl Pts',(-2.34309017083977,-1.,-3.04537822217256));
#51265=CARTESIAN_POINT('Ctrl Pts',(-2.34309017083977,1.,-3.04537822217256));
#51266=CARTESIAN_POINT('Ctrl Pts',(-2.34875673090771,-1.,-3.05015565829918));
#51267=CARTESIAN_POINT('Ctrl Pts',(-2.34875673090771,1.,-3.05015565829918));
#51268=CARTESIAN_POINT('Ctrl Pts',(-2.35453559889474,-1.,-3.05497218368146));
#51269=CARTESIAN_POINT('Ctrl Pts',(-2.35453559889474,1.,-3.05497218368146));
#51270=CARTESIAN_POINT('Ctrl Pts',(-2.36039011602072,-1.,-3.0597826624004));
#51271=CARTESIAN_POINT('Ctrl Pts',(-2.36039011602072,1.,-3.0597826624004));
#51272=CARTESIAN_POINT('Ctrl Pts',(-2.36628220107009,-1.,-3.06453964643162));
#51273=CARTESIAN_POINT('Ctrl Pts',(-2.36628220107009,1.,-3.06453964643162));
#51274=CARTESIAN_POINT('Ctrl Pts',(-2.37218678163178,-1.,-3.069212754975));
#51275=CARTESIAN_POINT('Ctrl Pts',(-2.37218678163178,1.,-3.069212754975));
#51276=CARTESIAN_POINT('Ctrl Pts',(-2.37809856205548,-1.,-3.07379777492165));
#51277=CARTESIAN_POINT('Ctrl Pts',(-2.37809856205548,1.,-3.07379777492165));
#51278=CARTESIAN_POINT('Ctrl Pts',(-2.38402401216126,-1.,-3.07830597244326));
#51279=CARTESIAN_POINT('Ctrl Pts',(-2.38402401216126,1.,-3.07830597244326));
#51280=CARTESIAN_POINT('Ctrl Pts',(-2.38997659219199,-1.,-3.08275773747093));
#51281=CARTESIAN_POINT('Ctrl Pts',(-2.38997659219199,1.,-3.08275773747093));
#51282=CARTESIAN_POINT('Ctrl Pts',(-2.39597098250631,-1.,-3.08717489512914));
#51283=CARTESIAN_POINT('Ctrl Pts',(-2.39597098250631,1.,-3.08717489512914));
#51284=CARTESIAN_POINT('Ctrl Pts',(-2.40201704423341,-1.,-3.091572660511));
#51285=CARTESIAN_POINT('Ctrl Pts',(-2.40201704423341,1.,-3.091572660511));
#51286=CARTESIAN_POINT('Ctrl Pts',(-2.40811612696369,-1.,-3.09595472616076));
#51287=CARTESIAN_POINT('Ctrl Pts',(-2.40811612696369,1.,-3.09595472616076));
#51288=CARTESIAN_POINT('Ctrl Pts',(-2.41426441798057,-1.,-3.1003177502767));
#51289=CARTESIAN_POINT('Ctrl Pts',(-2.41426441798057,1.,-3.1003177502767));
#51290=CARTESIAN_POINT('Ctrl Pts',(-2.42045498612489,-1.,-3.10465410280896));
#51291=CARTESIAN_POINT('Ctrl Pts',(-2.42045498612489,1.,-3.10465410280896));
#51292=CARTESIAN_POINT('Ctrl Pts',(-2.42668025870015,-1.,-3.10895518969595));
#51293=CARTESIAN_POINT('Ctrl Pts',(-2.42668025870015,1.,-3.10895518969595));
#51294=CARTESIAN_POINT('Ctrl Pts',(-2.43293449685144,-1.,-3.11321477659018));
#51295=CARTESIAN_POINT('Ctrl Pts',(-2.43293449685144,1.,-3.11321477659018));
#51296=CARTESIAN_POINT('Ctrl Pts',(-2.43921571477977,-1.,-3.11743156744186));
#51297=CARTESIAN_POINT('Ctrl Pts',(-2.43921571477977,1.,-3.11743156744186));
#51298=CARTESIAN_POINT('Ctrl Pts',(-2.44552433364715,-1.,-3.12160740887768));
#51299=CARTESIAN_POINT('Ctrl Pts',(-2.44552433364715,1.,-3.12160740887768));
#51300=CARTESIAN_POINT('Ctrl Pts',(-2.45186227369846,-1.,-3.12574608210847));
#51301=CARTESIAN_POINT('Ctrl Pts',(-2.45186227369846,1.,-3.12574608210847));
#51302=CARTESIAN_POINT('Ctrl Pts',(-2.45823188859366,-1.,-3.12985188384371));
#51303=CARTESIAN_POINT('Ctrl Pts',(-2.45823188859366,1.,-3.12985188384371));
#51304=CARTESIAN_POINT('Ctrl Pts',(-2.46463494332374,-1.,-3.13392826623906));
#51305=CARTESIAN_POINT('Ctrl Pts',(-2.46463494332374,1.,-3.13392826623906));
#51306=CARTESIAN_POINT('Ctrl Pts',(-2.47107164236838,-1.,-3.13797654408943));
#51307=CARTESIAN_POINT('Ctrl Pts',(-2.47107164236838,1.,-3.13797654408943));
#51308=CARTESIAN_POINT('Ctrl Pts',(-2.47754112428043,-1.,-3.14199655778863));
#51309=CARTESIAN_POINT('Ctrl Pts',(-2.47754112428043,1.,-3.14199655778863));
#51310=CARTESIAN_POINT('Ctrl Pts',(-2.4840418741839,-1.,-3.14598722723896));
#51311=CARTESIAN_POINT('Ctrl Pts',(-2.4840418741839,1.,-3.14598722723896));
#51312=CARTESIAN_POINT('Ctrl Pts',(-2.49057217131988,-1.,-3.14994715298907));
#51313=CARTESIAN_POINT('Ctrl Pts',(-2.49057217131988,1.,-3.14994715298907));
#51314=CARTESIAN_POINT('Ctrl Pts',(-2.49713050858896,-1.,-3.15387518039046));
#51315=CARTESIAN_POINT('Ctrl Pts',(-2.49713050858896,1.,-3.15387518039046));
#51316=CARTESIAN_POINT('Ctrl Pts',(-2.50371605688252,-1.,-3.15777102413957));
#51317=CARTESIAN_POINT('Ctrl Pts',(-2.50371605688252,1.,-3.15777102413957));
#51318=CARTESIAN_POINT('Ctrl Pts',(-2.51032851007894,-1.,-3.16163506380157));
#51319=CARTESIAN_POINT('Ctrl Pts',(-2.51032851007894,1.,-3.16163506380157));
#51320=CARTESIAN_POINT('Ctrl Pts',(-2.51696788755577,-1.,-3.16546808277023));
#51321=CARTESIAN_POINT('Ctrl Pts',(-2.51696788755577,1.,-3.16546808277023));
#51322=CARTESIAN_POINT('Ctrl Pts',(-2.52363434671788,-1.,-3.16927102130736));
#51323=CARTESIAN_POINT('Ctrl Pts',(-2.52363434671788,1.,-3.16927102130736));
#51324=CARTESIAN_POINT('Ctrl Pts',(-2.53032800406941,-1.,-3.17304474093612));
#51325=CARTESIAN_POINT('Ctrl Pts',(-2.53032800406941,1.,-3.17304474093612));
#51326=CARTESIAN_POINT('Ctrl Pts',(-2.53704871950948,-1.,-3.17678974135318));
#51327=CARTESIAN_POINT('Ctrl Pts',(-2.53704871950948,1.,-3.17678974135318));
#51328=CARTESIAN_POINT('Ctrl Pts',(-2.54379612553051,-1.,-3.1805061975064));
#51329=CARTESIAN_POINT('Ctrl Pts',(-2.54379612553051,1.,-3.1805061975064));
#51330=CARTESIAN_POINT('Ctrl Pts',(-2.55056972387731,-1.,-3.18419408529594));
#51331=CARTESIAN_POINT('Ctrl Pts',(-2.55056972387731,1.,-3.18419408529594));
#51332=CARTESIAN_POINT('Ctrl Pts',(-2.55736896206056,-1.,-3.18785328116218));
#51333=CARTESIAN_POINT('Ctrl Pts',(-2.55736896206056,1.,-3.18785328116218));
#51334=CARTESIAN_POINT('Ctrl Pts',(-2.56419331092858,-1.,-3.19148366395139));
#51335=CARTESIAN_POINT('Ctrl Pts',(-2.56419331092858,1.,-3.19148366395139));
#51336=CARTESIAN_POINT('Ctrl Pts',(-2.57104235897899,-1.,-3.19508523784363));
#51337=CARTESIAN_POINT('Ctrl Pts',(-2.57104235897899,1.,-3.19508523784363));
#51338=CARTESIAN_POINT('Ctrl Pts',(-2.57791581908875,-1.,-3.19865814628682));
#51339=CARTESIAN_POINT('Ctrl Pts',(-2.57791581908875,1.,-3.19865814628682));
#51340=CARTESIAN_POINT('Ctrl Pts',(-2.58481347777729,-1.,-3.20220261408414));
#51341=CARTESIAN_POINT('Ctrl Pts',(-2.58481347777729,1.,-3.20220261408414));
#51342=CARTESIAN_POINT('Ctrl Pts',(-2.59173516023481,-1.,-3.2057189102873));
#51343=CARTESIAN_POINT('Ctrl Pts',(-2.59173516023481,1.,-3.2057189102873));
#51344=CARTESIAN_POINT('Ctrl Pts',(-2.59868069194342,-1.,-3.20920730569681));
#51345=CARTESIAN_POINT('Ctrl Pts',(-2.59868069194342,1.,-3.20920730569681));
#51346=CARTESIAN_POINT('Ctrl Pts',(-2.60564985360017,-1.,-3.21266802609682));
#51347=CARTESIAN_POINT('Ctrl Pts',(-2.60564985360017,1.,-3.21266802609682));
#51348=CARTESIAN_POINT('Ctrl Pts',(-2.61264236719171,-1.,-3.21610123233082));
#51349=CARTESIAN_POINT('Ctrl Pts',(-2.61264236719171,1.,-3.21610123233082));
#51350=CARTESIAN_POINT('Ctrl Pts',(-2.61965792832947,-1.,-3.21950704109321));
#51351=CARTESIAN_POINT('Ctrl Pts',(-2.61965792832947,1.,-3.21950704109321));
#51352=CARTESIAN_POINT('Ctrl Pts',(-2.62669622735912,-1.,-3.2228855361324));
#51353=CARTESIAN_POINT('Ctrl Pts',(-2.62669622735912,1.,-3.2228855361324));
#51354=CARTESIAN_POINT('Ctrl Pts',(-2.63375697391372,-1.,-3.2262367829246));
#51355=CARTESIAN_POINT('Ctrl Pts',(-2.63375697391372,1.,-3.2262367829246));
#51356=CARTESIAN_POINT('Ctrl Pts',(-2.64083992181823,-1.,-3.22956084358547));
#51357=CARTESIAN_POINT('Ctrl Pts',(-2.64083992181823,1.,-3.22956084358547));
#51358=CARTESIAN_POINT('Ctrl Pts',(-2.64794488743038,-1.,-3.23285778737096));
#51359=CARTESIAN_POINT('Ctrl Pts',(-2.64794488743038,1.,-3.23285778737096));
#51360=CARTESIAN_POINT('Ctrl Pts',(-2.65507173961555,-1.,-3.236127680639));
#51361=CARTESIAN_POINT('Ctrl Pts',(-2.65507173961555,1.,-3.236127680639));
#51362=CARTESIAN_POINT('Ctrl Pts',(-2.6607906631847,-1.,-3.23872200034785));
#51363=CARTESIAN_POINT('Ctrl Pts',(-2.6607906631847,1.,-3.23872200034785));
#51364=CARTESIAN_POINT('Ctrl Pts',(-2.66508964663997,-1.,-3.24065561086749));
#51365=CARTESIAN_POINT('Ctrl Pts',(-2.66508964663997,1.,-3.24065561086749));
#51366=CARTESIAN_POINT('Ctrl Pts',(-2.66795998539579,-1.,-3.24193929584471));
#51367=CARTESIAN_POINT('Ctrl Pts',(-2.66795998539579,1.,-3.24193929584471));
#51368=CARTESIAN_POINT('Ctrl Pts',(-2.66939624221984,-1.,-3.24257979115744));
#51369=CARTESIAN_POINT('Ctrl Pts',(-2.66939624221984,1.,-3.24257979115744));
#51370=CARTESIAN_POINT('',(-2.27737254473521,1.,-2.97927412174279));
#51371=CARTESIAN_POINT('Ctrl Pts',(-2.27737254473521,-1.,-2.97927412174279));
#51372=CARTESIAN_POINT('Ctrl Pts',(-2.27737254473521,-0.666666666666667,
-2.97927412174279));
#51373=CARTESIAN_POINT('Ctrl Pts',(-2.27737254473521,-0.333333333333333,
-2.97927412174279));
#51374=CARTESIAN_POINT('Ctrl Pts',(-2.27737254473521,0.333333333333333,
-2.97927412174279));
#51375=CARTESIAN_POINT('Ctrl Pts',(-2.27737254473521,0.666666666666667,
-2.97927412174279));
#51376=CARTESIAN_POINT('Ctrl Pts',(-2.27737254473521,1.,-2.97927412174279));
#51377=CARTESIAN_POINT('',(-2.66939624221984,1.,-3.24257979115744));
#51378=CARTESIAN_POINT('',(-2.66939624221984,0.,-3.24257979115744));
#51379=CARTESIAN_POINT('Ctrl Pts',(-2.27737254473521,1.,-2.97927412174279));
#51380=CARTESIAN_POINT('Ctrl Pts',(-2.27737238849288,1.,-2.97932307137477));
#51381=CARTESIAN_POINT('Ctrl Pts',(-2.27743009389684,1.,-2.9795116710597));
#51382=CARTESIAN_POINT('Ctrl Pts',(-2.27776738270289,1.,-2.98007383024208));
#51383=CARTESIAN_POINT('Ctrl Pts',(-2.27877674853766,1.,-2.9814234180956));
#51384=CARTESIAN_POINT('Ctrl Pts',(-2.28100472516679,1.,-2.98413343613983));
#51385=CARTESIAN_POINT('Ctrl Pts',(-2.28446419115919,1.,-2.9881543273478));
#51386=CARTESIAN_POINT('Ctrl Pts',(-2.28882328690362,1.,-2.99307930984034));
#51387=CARTESIAN_POINT('Ctrl Pts',(-2.29385894577754,1.,-2.99863310339691));
#51388=CARTESIAN_POINT('Ctrl Pts',(-2.29932091315775,1.,-3.00450832658613));
#51389=CARTESIAN_POINT('Ctrl Pts',(-2.30496809486482,1.,-3.01041131063823));
#51390=CARTESIAN_POINT('Ctrl Pts',(-2.31060449886629,1.,-3.01610726819086));
#51391=CARTESIAN_POINT('Ctrl Pts',(-2.31612479121631,1.,-3.02147780668161));
#51392=CARTESIAN_POINT('Ctrl Pts',(-2.32151944306402,1.,-3.02652678416611));
#51393=CARTESIAN_POINT('Ctrl Pts',(-2.32683687412097,1.,-3.03133125185136));
#51394=CARTESIAN_POINT('Ctrl Pts',(-2.33215619079829,1.,-3.03600588555793));
#51395=CARTESIAN_POINT('Ctrl Pts',(-2.33755792953706,1.,-3.04066496998544));
#51396=CARTESIAN_POINT('Ctrl Pts',(-2.34309017083977,1.,-3.04537822217256));
#51397=CARTESIAN_POINT('Ctrl Pts',(-2.34875673090771,1.,-3.05015565829918));
#51398=CARTESIAN_POINT('Ctrl Pts',(-2.35453559889474,1.,-3.05497218368146));
#51399=CARTESIAN_POINT('Ctrl Pts',(-2.36039011602072,1.,-3.0597826624004));
#51400=CARTESIAN_POINT('Ctrl Pts',(-2.36628220107009,1.,-3.06453964643162));
#51401=CARTESIAN_POINT('Ctrl Pts',(-2.37218678163178,1.,-3.069212754975));
#51402=CARTESIAN_POINT('Ctrl Pts',(-2.37809856205548,1.,-3.07379777492165));
#51403=CARTESIAN_POINT('Ctrl Pts',(-2.38402401216126,1.,-3.07830597244326));
#51404=CARTESIAN_POINT('Ctrl Pts',(-2.38997659219199,1.,-3.08275773747093));
#51405=CARTESIAN_POINT('Ctrl Pts',(-2.39597098250631,1.,-3.08717489512914));
#51406=CARTESIAN_POINT('Ctrl Pts',(-2.40201704423341,1.,-3.091572660511));
#51407=CARTESIAN_POINT('Ctrl Pts',(-2.40811612696369,1.,-3.09595472616076));
#51408=CARTESIAN_POINT('Ctrl Pts',(-2.41426441798057,1.,-3.1003177502767));
#51409=CARTESIAN_POINT('Ctrl Pts',(-2.42045498612489,1.,-3.10465410280896));
#51410=CARTESIAN_POINT('Ctrl Pts',(-2.42668025870015,1.,-3.10895518969595));
#51411=CARTESIAN_POINT('Ctrl Pts',(-2.43293449685144,1.,-3.11321477659018));
#51412=CARTESIAN_POINT('Ctrl Pts',(-2.43921571477977,1.,-3.11743156744186));
#51413=CARTESIAN_POINT('Ctrl Pts',(-2.44552433364715,1.,-3.12160740887768));
#51414=CARTESIAN_POINT('Ctrl Pts',(-2.45186227369846,1.,-3.12574608210847));
#51415=CARTESIAN_POINT('Ctrl Pts',(-2.45823188859366,1.,-3.12985188384371));
#51416=CARTESIAN_POINT('Ctrl Pts',(-2.46463494332374,1.,-3.13392826623906));
#51417=CARTESIAN_POINT('Ctrl Pts',(-2.47107164236838,1.,-3.13797654408943));
#51418=CARTESIAN_POINT('Ctrl Pts',(-2.47754112428043,1.,-3.14199655778863));
#51419=CARTESIAN_POINT('Ctrl Pts',(-2.4840418741839,1.,-3.14598722723896));
#51420=CARTESIAN_POINT('Ctrl Pts',(-2.49057217131988,1.,-3.14994715298907));
#51421=CARTESIAN_POINT('Ctrl Pts',(-2.49713050858896,1.,-3.15387518039046));
#51422=CARTESIAN_POINT('Ctrl Pts',(-2.50371605688252,1.,-3.15777102413957));
#51423=CARTESIAN_POINT('Ctrl Pts',(-2.51032851007894,1.,-3.16163506380157));
#51424=CARTESIAN_POINT('Ctrl Pts',(-2.51696788755577,1.,-3.16546808277023));
#51425=CARTESIAN_POINT('Ctrl Pts',(-2.52363434671788,1.,-3.16927102130736));
#51426=CARTESIAN_POINT('Ctrl Pts',(-2.53032800406941,1.,-3.17304474093612));
#51427=CARTESIAN_POINT('Ctrl Pts',(-2.53704871950948,1.,-3.17678974135318));
#51428=CARTESIAN_POINT('Ctrl Pts',(-2.54379612553051,1.,-3.1805061975064));
#51429=CARTESIAN_POINT('Ctrl Pts',(-2.55056972387731,1.,-3.18419408529594));
#51430=CARTESIAN_POINT('Ctrl Pts',(-2.55736896206056,1.,-3.18785328116218));
#51431=CARTESIAN_POINT('Ctrl Pts',(-2.56419331092858,1.,-3.19148366395139));
#51432=CARTESIAN_POINT('Ctrl Pts',(-2.57104235897899,1.,-3.19508523784363));
#51433=CARTESIAN_POINT('Ctrl Pts',(-2.57791581908875,1.,-3.19865814628682));
#51434=CARTESIAN_POINT('Ctrl Pts',(-2.58481347777729,1.,-3.20220261408414));
#51435=CARTESIAN_POINT('Ctrl Pts',(-2.59173516023481,1.,-3.2057189102873));
#51436=CARTESIAN_POINT('Ctrl Pts',(-2.59868069194342,1.,-3.20920730569681));
#51437=CARTESIAN_POINT('Ctrl Pts',(-2.60564985360017,1.,-3.21266802609682));
#51438=CARTESIAN_POINT('Ctrl Pts',(-2.61264236719171,1.,-3.21610123233082));
#51439=CARTESIAN_POINT('Ctrl Pts',(-2.61965792832947,1.,-3.21950704109321));
#51440=CARTESIAN_POINT('Ctrl Pts',(-2.62669622735912,1.,-3.2228855361324));
#51441=CARTESIAN_POINT('Ctrl Pts',(-2.63375697391372,1.,-3.2262367829246));
#51442=CARTESIAN_POINT('Ctrl Pts',(-2.64083992181823,1.,-3.22956084358547));
#51443=CARTESIAN_POINT('Ctrl Pts',(-2.64794488743038,1.,-3.23285778737096));
#51444=CARTESIAN_POINT('Ctrl Pts',(-2.65507173961555,1.,-3.236127680639));
#51445=CARTESIAN_POINT('Ctrl Pts',(-2.6607906631847,1.,-3.23872200034785));
#51446=CARTESIAN_POINT('Ctrl Pts',(-2.66508964663997,1.,-3.24065561086749));
#51447=CARTESIAN_POINT('Ctrl Pts',(-2.66795998539579,1.,-3.24193929584471));
#51448=CARTESIAN_POINT('Ctrl Pts',(-2.66939624221984,1.,-3.24257979115744));
#51449=CARTESIAN_POINT('Origin',(-2.66939624221984,0.,-3.24257979115744));
#51450=CARTESIAN_POINT('',(-2.78507268004356,1.,-3.14378277984898));
#51451=CARTESIAN_POINT('Origin',(0.,0.,0.));
#51452=CARTESIAN_POINT('',(-2.12971124846838,1.,-3.08655633322109));
#51453=CARTESIAN_POINT('Origin',(0.,1.,0.));
#51454=CARTESIAN_POINT('Ctrl Pts',(-2.12971124846838,1.,-3.08655633322109));
#51455=CARTESIAN_POINT('Ctrl Pts',(-2.12971124846838,0.666666666666667,
-3.08655633322109));
#51456=CARTESIAN_POINT('Ctrl Pts',(-2.12971124846838,0.333333333333333,
-3.08655633322109));
#51457=CARTESIAN_POINT('Ctrl Pts',(-2.12971124846838,-0.333333333333333,
-3.08655633322109));
#51458=CARTESIAN_POINT('Ctrl Pts',(-2.12971124846838,-0.666666666666667,
-3.08655633322109));
#51459=CARTESIAN_POINT('Ctrl Pts',(-2.12971124846838,-1.,-3.08655633322109));
#51460=CARTESIAN_POINT('Ctrl Pts',(-2.25898783642071,-1.,-3.54075895182139));
#51461=CARTESIAN_POINT('Ctrl Pts',(-2.25898783642071,1.,-3.54075895182139));
#51462=CARTESIAN_POINT('Ctrl Pts',(-2.25882251694918,-1.,-3.5391950664771));
#51463=CARTESIAN_POINT('Ctrl Pts',(-2.25882251694918,1.,-3.5391950664771));
#51464=CARTESIAN_POINT('Ctrl Pts',(-2.25848864344599,-1.,-3.53606853163247));
#51465=CARTESIAN_POINT('Ctrl Pts',(-2.25848864344599,1.,-3.53606853163247));
#51466=CARTESIAN_POINT('Ctrl Pts',(-2.25797812951166,-1.,-3.53138243689932));
#51467=CARTESIAN_POINT('Ctrl Pts',(-2.25797812951166,1.,-3.53138243689932));
#51468=CARTESIAN_POINT('Ctrl Pts',(-2.25727802942141,-1.,-3.52514172849666));
#51469=CARTESIAN_POINT('Ctrl Pts',(-2.25727802942141,1.,-3.52514172849666));
#51470=CARTESIAN_POINT('Ctrl Pts',(-2.25637049456061,-1.,-3.51735323669213));
#51471=CARTESIAN_POINT('Ctrl Pts',(-2.25637049456061,1.,-3.51735323669213));
#51472=CARTESIAN_POINT('Ctrl Pts',(-2.25543046980351,-1.,-3.50957720118209));
#51473=CARTESIAN_POINT('Ctrl Pts',(-2.25543046980351,1.,-3.50957720118209));
#51474=CARTESIAN_POINT('Ctrl Pts',(-2.25445785151923,-1.,-3.50181372618058));
#51475=CARTESIAN_POINT('Ctrl Pts',(-2.25445785151923,1.,-3.50181372618058));
#51476=CARTESIAN_POINT('Ctrl Pts',(-2.25345251709453,-1.,-3.49406296494309));
#51477=CARTESIAN_POINT('Ctrl Pts',(-2.25345251709453,1.,-3.49406296494309));
#51478=CARTESIAN_POINT('Ctrl Pts',(-2.25241433138231,-1.,-3.48632513240231));
#51479=CARTESIAN_POINT('Ctrl Pts',(-2.25241433138231,1.,-3.48632513240231));
#51480=CARTESIAN_POINT('Ctrl Pts',(-2.25134314238258,-1.,-3.47860048448015));
#51481=CARTESIAN_POINT('Ctrl Pts',(-2.25134314238258,1.,-3.47860048448015));
#51482=CARTESIAN_POINT('Ctrl Pts',(-2.25023877475674,-1.,-3.47088928979467));
#51483=CARTESIAN_POINT('Ctrl Pts',(-2.25023877475674,1.,-3.47088928979467));
#51484=CARTESIAN_POINT('Ctrl Pts',(-2.24910102345977,-1.,-3.46319180177474));
#51485=CARTESIAN_POINT('Ctrl Pts',(-2.24910102345977,1.,-3.46319180177474));
#51486=CARTESIAN_POINT('Ctrl Pts',(-2.24792964960874,-1.,-3.45550823512213));
#51487=CARTESIAN_POINT('Ctrl Pts',(-2.24792964960874,1.,-3.45550823512213));
#51488=CARTESIAN_POINT('Ctrl Pts',(-2.24672437070139,-1.,-3.44783872863448));
#51489=CARTESIAN_POINT('Ctrl Pts',(-2.24672437070139,1.,-3.44783872863448));
#51490=CARTESIAN_POINT('Ctrl Pts',(-2.24548487526212,-1.,-3.44018336460619));
#51491=CARTESIAN_POINT('Ctrl Pts',(-2.24548487526212,1.,-3.44018336460619));
#51492=CARTESIAN_POINT('Ctrl Pts',(-2.24421085338856,-1.,-3.43254222615007));
#51493=CARTESIAN_POINT('Ctrl Pts',(-2.24421085338856,1.,-3.43254222615007));
#51494=CARTESIAN_POINT('Ctrl Pts',(-2.24290202531144,-1.,-3.42491544683075));
#51495=CARTESIAN_POINT('Ctrl Pts',(-2.24290202531144,1.,-3.42491544683075));
#51496=CARTESIAN_POINT('Ctrl Pts',(-2.24155816587811,-1.,-3.41730325539119));
#51497=CARTESIAN_POINT('Ctrl Pts',(-2.24155816587811,1.,-3.41730325539119));
#51498=CARTESIAN_POINT('Ctrl Pts',(-2.24017914395211,-1.,-3.40970604190205));
#51499=CARTESIAN_POINT('Ctrl Pts',(-2.24017914395211,1.,-3.40970604190205));
#51500=CARTESIAN_POINT('Ctrl Pts',(-2.23876491124064,-1.,-3.40212434705511));
#51501=CARTESIAN_POINT('Ctrl Pts',(-2.23876491124064,1.,-3.40212434705511));
#51502=CARTESIAN_POINT('Ctrl Pts',(-2.23731541452727,-1.,-3.39455873448088));
#51503=CARTESIAN_POINT('Ctrl Pts',(-2.23731541452727,1.,-3.39455873448088));
#51504=CARTESIAN_POINT('Ctrl Pts',(-2.23583052276281,-1.,-3.38700968549522));
#51505=CARTESIAN_POINT('Ctrl Pts',(-2.23583052276281,1.,-3.38700968549522));
#51506=CARTESIAN_POINT('Ctrl Pts',(-2.23430995599572,-1.,-3.37947749555649));
#51507=CARTESIAN_POINT('Ctrl Pts',(-2.23430995599572,1.,-3.37947749555649));
#51508=CARTESIAN_POINT('Ctrl Pts',(-2.23275319569253,-1.,-3.37196214349356));
#51509=CARTESIAN_POINT('Ctrl Pts',(-2.23275319569253,1.,-3.37196214349356));
#51510=CARTESIAN_POINT('Ctrl Pts',(-2.23115945849777,-1.,-3.36446325227908));
#51511=CARTESIAN_POINT('Ctrl Pts',(-2.23115945849777,1.,-3.36446325227908));
#51512=CARTESIAN_POINT('Ctrl Pts',(-2.22952789881011,-1.,-3.35698038165529));
#51513=CARTESIAN_POINT('Ctrl Pts',(-2.22952789881011,1.,-3.35698038165529));
#51514=CARTESIAN_POINT('Ctrl Pts',(-2.22785777756588,-1.,-3.34951327111117));
#51515=CARTESIAN_POINT('Ctrl Pts',(-2.22785777756588,1.,-3.34951327111117));
#51516=CARTESIAN_POINT('Ctrl Pts',(-2.22614863918044,-1.,-3.34206209449371));
#51517=CARTESIAN_POINT('Ctrl Pts',(-2.22614863918044,1.,-3.34206209449371));
#51518=CARTESIAN_POINT('Ctrl Pts',(-2.224400498785,-1.,-3.3346277284958));
#51519=CARTESIAN_POINT('Ctrl Pts',(-2.224400498785,1.,-3.3346277284958));
#51520=CARTESIAN_POINT('Ctrl Pts',(-2.22261398879623,-1.,-3.32721196326019));
#51521=CARTESIAN_POINT('Ctrl Pts',(-2.22261398879623,1.,-3.32721196326019));
#51522=CARTESIAN_POINT('Ctrl Pts',(-2.22078990842768,-1.,-3.31981686778008));
#51523=CARTESIAN_POINT('Ctrl Pts',(-2.22078990842768,1.,-3.31981686778008));
#51524=CARTESIAN_POINT('Ctrl Pts',(-2.21892881679083,-1.,-3.31244421655662));
#51525=CARTESIAN_POINT('Ctrl Pts',(-2.21892881679083,1.,-3.31244421655662));
#51526=CARTESIAN_POINT('Ctrl Pts',(-2.21703059947837,-1.,-3.3050948781957));
#51527=CARTESIAN_POINT('Ctrl Pts',(-2.21703059947837,1.,-3.3050948781957));
#51528=CARTESIAN_POINT('Ctrl Pts',(-2.2150940692337,-1.,-3.29776825193162));
#51529=CARTESIAN_POINT('Ctrl Pts',(-2.2150940692337,1.,-3.29776825193162));
#51530=CARTESIAN_POINT('Ctrl Pts',(-2.21311648827391,-1.,-3.29046159238344));
#51531=CARTESIAN_POINT('Ctrl Pts',(-2.21311648827391,1.,-3.29046159238344));
#51532=CARTESIAN_POINT('Ctrl Pts',(-2.21109449750638,-1.,-3.28317133333127));
#51533=CARTESIAN_POINT('Ctrl Pts',(-2.21109449750638,1.,-3.28317133333127));
#51534=CARTESIAN_POINT('Ctrl Pts',(-2.20902509417425,-1.,-3.27589448005534));
#51535=CARTESIAN_POINT('Ctrl Pts',(-2.20902509417425,1.,-3.27589448005534));
#51536=CARTESIAN_POINT('Ctrl Pts',(-2.20690665217741,-1.,-3.2686300613678));
#51537=CARTESIAN_POINT('Ctrl Pts',(-2.20690665217741,1.,-3.2686300613678));
#51538=CARTESIAN_POINT('Ctrl Pts',(-2.20473979048682,-1.,-3.26138036637711));
#51539=CARTESIAN_POINT('Ctrl Pts',(-2.20473979048682,1.,-3.26138036637711));
#51540=CARTESIAN_POINT('Ctrl Pts',(-2.20252866491554,-1.,-3.25415277957789));
#51541=CARTESIAN_POINT('Ctrl Pts',(-2.20252866491554,1.,-3.25415277957789));
#51542=CARTESIAN_POINT('Ctrl Pts',(-2.20027910880993,-1.,-3.24695715874356));
#51543=CARTESIAN_POINT('Ctrl Pts',(-2.20027910880993,1.,-3.24695715874356));
#51544=CARTESIAN_POINT('Ctrl Pts',(-2.19799623693263,-1.,-3.23980245361323));
#51545=CARTESIAN_POINT('Ctrl Pts',(-2.19799623693263,1.,-3.23980245361323));
#51546=CARTESIAN_POINT('Ctrl Pts',(-2.19568204933172,-1.,-3.23269332296938));
#51547=CARTESIAN_POINT('Ctrl Pts',(-2.19568204933172,1.,-3.23269332296938));
#51548=CARTESIAN_POINT('Ctrl Pts',(-2.19333345123531,-1.,-3.22562734221636));
#51549=CARTESIAN_POINT('Ctrl Pts',(-2.19333345123531,1.,-3.22562734221636));
#51550=CARTESIAN_POINT('Ctrl Pts',(-2.1909390194865,-1.,-3.21859043114069));
#51551=CARTESIAN_POINT('Ctrl Pts',(-2.1909390194865,1.,-3.21859043114069));
#51552=CARTESIAN_POINT('Ctrl Pts',(-2.18848253363878,-1.,-3.21156188355736));
#51553=CARTESIAN_POINT('Ctrl Pts',(-2.18848253363878,1.,-3.21156188355736));
#51554=CARTESIAN_POINT('Ctrl Pts',(-2.18594876115914,-1.,-3.20452259717947));
#51555=CARTESIAN_POINT('Ctrl Pts',(-2.18594876115914,1.,-3.20452259717947));
#51556=CARTESIAN_POINT('Ctrl Pts',(-2.18332898656595,-1.,-3.197462937404));
#51557=CARTESIAN_POINT('Ctrl Pts',(-2.18332898656595,1.,-3.197462937404));
#51558=CARTESIAN_POINT('Ctrl Pts',(-2.18062558031789,-1.,-3.19038924261589));
#51559=CARTESIAN_POINT('Ctrl Pts',(-2.18062558031789,1.,-3.19038924261589));
#51560=CARTESIAN_POINT('Ctrl Pts',(-2.17785968847172,-1.,-3.18333474627851));
#51561=CARTESIAN_POINT('Ctrl Pts',(-2.17785968847172,1.,-3.18333474627851));
#51562=CARTESIAN_POINT('Ctrl Pts',(-2.17506466903736,-1.,-3.17635032802584));
#51563=CARTESIAN_POINT('Ctrl Pts',(-2.17506466903736,1.,-3.17635032802584));
#51564=CARTESIAN_POINT('Ctrl Pts',(-2.17227212063857,-1.,-3.16948480019555));
#51565=CARTESIAN_POINT('Ctrl Pts',(-2.17227212063857,1.,-3.16948480019555));
#51566=CARTESIAN_POINT('Ctrl Pts',(-2.16949910801237,-1.,-3.16276685102999));
#51567=CARTESIAN_POINT('Ctrl Pts',(-2.16949910801237,1.,-3.16276685102999));
#51568=CARTESIAN_POINT('Ctrl Pts',(-2.1667372844767,-1.,-3.15618975593627));
#51569=CARTESIAN_POINT('Ctrl Pts',(-2.1667372844767,1.,-3.15618975593627));
#51570=CARTESIAN_POINT('Ctrl Pts',(-2.16393520288009,-1.,-3.14968624388961));
#51571=CARTESIAN_POINT('Ctrl Pts',(-2.16393520288009,1.,-3.14968624388961));
#51572=CARTESIAN_POINT('Ctrl Pts',(-2.16100905914341,-1.,-3.14314440426882));
#51573=CARTESIAN_POINT('Ctrl Pts',(-2.16100905914341,1.,-3.14314440426882));
#51574=CARTESIAN_POINT('Ctrl Pts',(-2.15787423530583,-1.,-3.136453565629));
#51575=CARTESIAN_POINT('Ctrl Pts',(-2.15787423530583,1.,-3.136453565629));
#51576=CARTESIAN_POINT('Ctrl Pts',(-2.15447241382872,-1.,-3.12954386795575));
#51577=CARTESIAN_POINT('Ctrl Pts',(-2.15447241382872,1.,-3.12954386795575));
#51578=CARTESIAN_POINT('Ctrl Pts',(-2.15079698090627,-1.,-3.12242318152001));
#51579=CARTESIAN_POINT('Ctrl Pts',(-2.15079698090627,1.,-3.12242318152001));
#51580=CARTESIAN_POINT('Ctrl Pts',(-2.1469279845768,-1.,-3.11522827017075));
#51581=CARTESIAN_POINT('Ctrl Pts',(-2.1469279845768,1.,-3.11522827017075));
#51582=CARTESIAN_POINT('Ctrl Pts',(-2.14302815602195,-1.,-3.10821808669189));
#51583=CARTESIAN_POINT('Ctrl Pts',(-2.14302815602195,1.,-3.10821808669189));
#51584=CARTESIAN_POINT('Ctrl Pts',(-2.13930228863968,-1.,-3.1017126739137));
#51585=CARTESIAN_POINT('Ctrl Pts',(-2.13930228863968,1.,-3.1017126739137));
#51586=CARTESIAN_POINT('Ctrl Pts',(-2.13596538661154,-1.,-3.09604502421197));
#51587=CARTESIAN_POINT('Ctrl Pts',(-2.13596538661154,1.,-3.09604502421197));
#51588=CARTESIAN_POINT('Ctrl Pts',(-2.13321032560805,-1.,-3.09151235281832));
#51589=CARTESIAN_POINT('Ctrl Pts',(-2.13321032560805,1.,-3.09151235281832));
#51590=CARTESIAN_POINT('Ctrl Pts',(-2.13116819908264,-1.,-3.08831615619661));
#51591=CARTESIAN_POINT('Ctrl Pts',(-2.13116819908264,1.,-3.08831615619661));
#51592=CARTESIAN_POINT('Ctrl Pts',(-2.1301541297915,-1.,-3.08690399991003));
#51593=CARTESIAN_POINT('Ctrl Pts',(-2.1301541297915,1.,-3.08690399991003));
#51594=CARTESIAN_POINT('Ctrl Pts',(-2.12975158752197,-1.,-3.08650326866821));
#51595=CARTESIAN_POINT('Ctrl Pts',(-2.12975158752197,1.,-3.08650326866821));
#51596=CARTESIAN_POINT('Ctrl Pts',(-2.12964222015945,-1.,-3.08652852644876));
#51597=CARTESIAN_POINT('Ctrl Pts',(-2.12964222015945,1.,-3.08652852644876));
#51598=CARTESIAN_POINT('Ctrl Pts',(-2.12962728847314,-1.,-3.08661426358891));
#51599=CARTESIAN_POINT('Ctrl Pts',(-2.12962728847314,1.,-3.08661426358891));
#51600=CARTESIAN_POINT('',(-2.25898783642071,1.,-3.54075895182139));
#51601=CARTESIAN_POINT('Ctrl Pts',(-2.25898783642071,1.,-3.54075895182139));
#51602=CARTESIAN_POINT('Ctrl Pts',(-2.25882251694918,1.,-3.5391950664771));
#51603=CARTESIAN_POINT('Ctrl Pts',(-2.25848864344599,1.,-3.53606853163247));
#51604=CARTESIAN_POINT('Ctrl Pts',(-2.25797812951166,1.,-3.53138243689932));
#51605=CARTESIAN_POINT('Ctrl Pts',(-2.25727802942141,1.,-3.52514172849666));
#51606=CARTESIAN_POINT('Ctrl Pts',(-2.25637049456061,1.,-3.51735323669213));
#51607=CARTESIAN_POINT('Ctrl Pts',(-2.25543046980351,1.,-3.50957720118209));
#51608=CARTESIAN_POINT('Ctrl Pts',(-2.25445785151923,1.,-3.50181372618058));
#51609=CARTESIAN_POINT('Ctrl Pts',(-2.25345251709453,1.,-3.49406296494309));
#51610=CARTESIAN_POINT('Ctrl Pts',(-2.25241433138231,1.,-3.48632513240231));
#51611=CARTESIAN_POINT('Ctrl Pts',(-2.25134314238258,1.,-3.47860048448015));
#51612=CARTESIAN_POINT('Ctrl Pts',(-2.25023877475674,1.,-3.47088928979467));
#51613=CARTESIAN_POINT('Ctrl Pts',(-2.24910102345977,1.,-3.46319180177474));
#51614=CARTESIAN_POINT('Ctrl Pts',(-2.24792964960874,1.,-3.45550823512213));
#51615=CARTESIAN_POINT('Ctrl Pts',(-2.24672437070139,1.,-3.44783872863448));
#51616=CARTESIAN_POINT('Ctrl Pts',(-2.24548487526212,1.,-3.44018336460619));
#51617=CARTESIAN_POINT('Ctrl Pts',(-2.24421085338856,1.,-3.43254222615007));
#51618=CARTESIAN_POINT('Ctrl Pts',(-2.24290202531144,1.,-3.42491544683075));
#51619=CARTESIAN_POINT('Ctrl Pts',(-2.24155816587811,1.,-3.41730325539119));
#51620=CARTESIAN_POINT('Ctrl Pts',(-2.24017914395211,1.,-3.40970604190205));
#51621=CARTESIAN_POINT('Ctrl Pts',(-2.23876491124064,1.,-3.40212434705511));
#51622=CARTESIAN_POINT('Ctrl Pts',(-2.23731541452727,1.,-3.39455873448088));
#51623=CARTESIAN_POINT('Ctrl Pts',(-2.23583052276281,1.,-3.38700968549522));
#51624=CARTESIAN_POINT('Ctrl Pts',(-2.23430995599572,1.,-3.37947749555649));
#51625=CARTESIAN_POINT('Ctrl Pts',(-2.23275319569253,1.,-3.37196214349356));
#51626=CARTESIAN_POINT('Ctrl Pts',(-2.23115945849777,1.,-3.36446325227908));
#51627=CARTESIAN_POINT('Ctrl Pts',(-2.22952789881011,1.,-3.35698038165529));
#51628=CARTESIAN_POINT('Ctrl Pts',(-2.22785777756588,1.,-3.34951327111117));
#51629=CARTESIAN_POINT('Ctrl Pts',(-2.22614863918044,1.,-3.34206209449371));
#51630=CARTESIAN_POINT('Ctrl Pts',(-2.224400498785,1.,-3.3346277284958));
#51631=CARTESIAN_POINT('Ctrl Pts',(-2.22261398879623,1.,-3.32721196326019));
#51632=CARTESIAN_POINT('Ctrl Pts',(-2.22078990842768,1.,-3.31981686778008));
#51633=CARTESIAN_POINT('Ctrl Pts',(-2.21892881679083,1.,-3.31244421655662));
#51634=CARTESIAN_POINT('Ctrl Pts',(-2.21703059947837,1.,-3.3050948781957));
#51635=CARTESIAN_POINT('Ctrl Pts',(-2.2150940692337,1.,-3.29776825193162));
#51636=CARTESIAN_POINT('Ctrl Pts',(-2.21311648827391,1.,-3.29046159238344));
#51637=CARTESIAN_POINT('Ctrl Pts',(-2.21109449750638,1.,-3.28317133333127));
#51638=CARTESIAN_POINT('Ctrl Pts',(-2.20902509417425,1.,-3.27589448005534));
#51639=CARTESIAN_POINT('Ctrl Pts',(-2.20690665217741,1.,-3.2686300613678));
#51640=CARTESIAN_POINT('Ctrl Pts',(-2.20473979048682,1.,-3.26138036637711));
#51641=CARTESIAN_POINT('Ctrl Pts',(-2.20252866491554,1.,-3.25415277957789));
#51642=CARTESIAN_POINT('Ctrl Pts',(-2.20027910880993,1.,-3.24695715874356));
#51643=CARTESIAN_POINT('Ctrl Pts',(-2.19799623693263,1.,-3.23980245361323));
#51644=CARTESIAN_POINT('Ctrl Pts',(-2.19568204933172,1.,-3.23269332296938));
#51645=CARTESIAN_POINT('Ctrl Pts',(-2.19333345123531,1.,-3.22562734221636));
#51646=CARTESIAN_POINT('Ctrl Pts',(-2.1909390194865,1.,-3.21859043114069));
#51647=CARTESIAN_POINT('Ctrl Pts',(-2.18848253363878,1.,-3.21156188355736));
#51648=CARTESIAN_POINT('Ctrl Pts',(-2.18594876115914,1.,-3.20452259717947));
#51649=CARTESIAN_POINT('Ctrl Pts',(-2.18332898656595,1.,-3.197462937404));
#51650=CARTESIAN_POINT('Ctrl Pts',(-2.18062558031789,1.,-3.19038924261589));
#51651=CARTESIAN_POINT('Ctrl Pts',(-2.17785968847172,1.,-3.18333474627851));
#51652=CARTESIAN_POINT('Ctrl Pts',(-2.17506466903736,1.,-3.17635032802584));
#51653=CARTESIAN_POINT('Ctrl Pts',(-2.17227212063857,1.,-3.16948480019555));
#51654=CARTESIAN_POINT('Ctrl Pts',(-2.16949910801237,1.,-3.16276685102999));
#51655=CARTESIAN_POINT('Ctrl Pts',(-2.1667372844767,1.,-3.15618975593627));
#51656=CARTESIAN_POINT('Ctrl Pts',(-2.16393520288009,1.,-3.14968624388961));
#51657=CARTESIAN_POINT('Ctrl Pts',(-2.16100905914341,1.,-3.14314440426882));
#51658=CARTESIAN_POINT('Ctrl Pts',(-2.15787423530583,1.,-3.136453565629));
#51659=CARTESIAN_POINT('Ctrl Pts',(-2.15447241382872,1.,-3.12954386795575));
#51660=CARTESIAN_POINT('Ctrl Pts',(-2.15079698090627,1.,-3.12242318152001));
#51661=CARTESIAN_POINT('Ctrl Pts',(-2.1469279845768,1.,-3.11522827017075));
#51662=CARTESIAN_POINT('Ctrl Pts',(-2.14302815602195,1.,-3.10821808669189));
#51663=CARTESIAN_POINT('Ctrl Pts',(-2.13930228863968,1.,-3.1017126739137));
#51664=CARTESIAN_POINT('Ctrl Pts',(-2.13596538661154,1.,-3.09604502421197));
#51665=CARTESIAN_POINT('Ctrl Pts',(-2.13321032560805,1.,-3.09151235281832));
#51666=CARTESIAN_POINT('Ctrl Pts',(-2.13132142793056,1.,-3.08855597949844));
#51667=CARTESIAN_POINT('Ctrl Pts',(-2.13034980480519,1.,-3.08717896996213));
#51668=CARTESIAN_POINT('Ctrl Pts',(-2.12991938762497,1.,-3.08668447250383));
#51669=CARTESIAN_POINT('Ctrl Pts',(-2.1297578506162,1.,-3.0865713108946));
#51670=CARTESIAN_POINT('Ctrl Pts',(-2.12971124846838,1.,-3.0865563332211));
#51671=CARTESIAN_POINT('',(-2.25898783642071,0.,-3.54075895182139));
#51672=CARTESIAN_POINT('Ctrl Pts',(-1.7833628895577,-1.,-3.2988053601491));
#51673=CARTESIAN_POINT('Ctrl Pts',(-1.7833628895577,1.,-3.2988053601491));
#51674=CARTESIAN_POINT('Ctrl Pts',(-1.78327971836342,-1.,-3.29877974053316));
#51675=CARTESIAN_POINT('Ctrl Pts',(-1.78327971836342,1.,-3.29877974053316));
#51676=CARTESIAN_POINT('Ctrl Pts',(-1.78320756177373,-1.,-3.29886572077632));
#51677=CARTESIAN_POINT('Ctrl Pts',(-1.78320756177373,1.,-3.29886572077632));
#51678=CARTESIAN_POINT('Ctrl Pts',(-1.7833818655594,-1.,-3.29940631674303));
#51679=CARTESIAN_POINT('Ctrl Pts',(-1.7833818655594,1.,-3.29940631674303));
#51680=CARTESIAN_POINT('Ctrl Pts',(-1.78417972819938,-1.,-3.30095096463517));
#51681=CARTESIAN_POINT('Ctrl Pts',(-1.78417972819938,1.,-3.30095096463517));
#51682=CARTESIAN_POINT('Ctrl Pts',(-1.78610045419846,-1.,-3.30422155559112));
#51683=CARTESIAN_POINT('Ctrl Pts',(-1.78610045419846,1.,-3.30422155559112));
#51684=CARTESIAN_POINT('Ctrl Pts',(-1.78888832245873,-1.,-3.30873412266788));
#51685=CARTESIAN_POINT('Ctrl Pts',(-1.78888832245873,1.,-3.30873412266788));
#51686=CARTESIAN_POINT('Ctrl Pts',(-1.79242331349949,-1.,-3.31428038326424));
#51687=CARTESIAN_POINT('Ctrl Pts',(-1.79242331349949,1.,-3.31428038326424));
#51688=CARTESIAN_POINT('Ctrl Pts',(-1.79652817033251,-1.,-3.3205535510082));
#51689=CARTESIAN_POINT('Ctrl Pts',(-1.79652817033251,1.,-3.3205535510082));
#51690=CARTESIAN_POINT('Ctrl Pts',(-1.80100380443406,-1.,-3.32721088039578));
#51691=CARTESIAN_POINT('Ctrl Pts',(-1.80100380443406,1.,-3.32721088039578));
#51692=CARTESIAN_POINT('Ctrl Pts',(-1.80565802981102,-1.,-3.33392460276808));
#51693=CARTESIAN_POINT('Ctrl Pts',(-1.80565802981102,1.,-3.33392460276808));
#51694=CARTESIAN_POINT('Ctrl Pts',(-1.81033399625352,-1.,-3.34043216147606));
#51695=CARTESIAN_POINT('Ctrl Pts',(-1.81033399625352,1.,-3.34043216147606));
#51696=CARTESIAN_POINT('Ctrl Pts',(-1.81494618732853,-1.,-3.34660014370673));
#51697=CARTESIAN_POINT('Ctrl Pts',(-1.81494618732853,1.,-3.34660014370673));
#51698=CARTESIAN_POINT('Ctrl Pts',(-1.81948458796829,-1.,-3.35243086937598));
#51699=CARTESIAN_POINT('Ctrl Pts',(-1.81948458796829,1.,-3.35243086937598));
#51700=CARTESIAN_POINT('Ctrl Pts',(-1.82398496829301,-1.,-3.35800801557424));
#51701=CARTESIAN_POINT('Ctrl Pts',(-1.82398496829301,1.,-3.35800801557424));
#51702=CARTESIAN_POINT('Ctrl Pts',(-1.82850752153199,-1.,-3.36345722124158));
#51703=CARTESIAN_POINT('Ctrl Pts',(-1.82850752153199,1.,-3.36345722124158));
#51704=CARTESIAN_POINT('Ctrl Pts',(-1.83311391452322,-1.,-3.36890396271836));
#51705=CARTESIAN_POINT('Ctrl Pts',(-1.83311391452322,1.,-3.36890396271836));
#51706=CARTESIAN_POINT('Ctrl Pts',(-1.83784072967077,-1.,-3.37442462015853));
#51707=CARTESIAN_POINT('Ctrl Pts',(-1.83784072967077,1.,-3.37442462015853));
#51708=CARTESIAN_POINT('Ctrl Pts',(-1.84269016931643,-1.,-3.38002968341157));
#51709=CARTESIAN_POINT('Ctrl Pts',(-1.84269016931643,1.,-3.38002968341157));
#51710=CARTESIAN_POINT('Ctrl Pts',(-1.84764441927753,-1.,-3.38569092349592));
#51711=CARTESIAN_POINT('Ctrl Pts',(-1.84764441927753,1.,-3.38569092349592));
#51712=CARTESIAN_POINT('Ctrl Pts',(-1.85267433291769,-1.,-3.39135802549398));
#51713=CARTESIAN_POINT('Ctrl Pts',(-1.85267433291769,1.,-3.39135802549398));
#51714=CARTESIAN_POINT('Ctrl Pts',(-1.85774972037062,-1.,-3.39697816833067));
#51715=CARTESIAN_POINT('Ctrl Pts',(-1.85774972037062,1.,-3.39697816833067));
#51716=CARTESIAN_POINT('Ctrl Pts',(-1.86285057051245,-1.,-3.40251742305476));
#51717=CARTESIAN_POINT('Ctrl Pts',(-1.86285057051245,1.,-3.40251742305476));
#51718=CARTESIAN_POINT('Ctrl Pts',(-1.86797231196654,-1.,-3.40797080000549));
#51719=CARTESIAN_POINT('Ctrl Pts',(-1.86797231196654,1.,-3.40797080000549));
#51720=CARTESIAN_POINT('Ctrl Pts',(-1.87311957248121,-1.,-3.41335043875209));
#51721=CARTESIAN_POINT('Ctrl Pts',(-1.87311957248121,1.,-3.41335043875209));
#51722=CARTESIAN_POINT('Ctrl Pts',(-1.87830245689344,-1.,-3.41867858383771));
#51723=CARTESIAN_POINT('Ctrl Pts',(-1.87830245689344,1.,-3.41867858383771));
#51724=CARTESIAN_POINT('Ctrl Pts',(-1.8835320506206,-1.,-3.42397908819736));
#51725=CARTESIAN_POINT('Ctrl Pts',(-1.8835320506206,1.,-3.42397908819736));
#51726=CARTESIAN_POINT('Ctrl Pts',(-1.88881571322009,-1.,-3.42926852222158));
#51727=CARTESIAN_POINT('Ctrl Pts',(-1.88881571322009,1.,-3.42926852222158));
#51728=CARTESIAN_POINT('Ctrl Pts',(-1.89415420002542,-1.,-3.43455074411571));
#51729=CARTESIAN_POINT('Ctrl Pts',(-1.89415420002542,1.,-3.43455074411571));
#51730=CARTESIAN_POINT('Ctrl Pts',(-1.89954426803384,-1.,-3.4398218567809));
#51731=CARTESIAN_POINT('Ctrl Pts',(-1.89954426803384,1.,-3.4398218567809));
#51732=CARTESIAN_POINT('Ctrl Pts',(-1.90498026502305,-1.,-3.44507323983367));
#51733=CARTESIAN_POINT('Ctrl Pts',(-1.90498026502305,1.,-3.44507323983367));
#51734=CARTESIAN_POINT('Ctrl Pts',(-1.91045605593639,-1.,-3.45029522038888));
#51735=CARTESIAN_POINT('Ctrl Pts',(-1.91045605593639,1.,-3.45029522038888));
#51736=CARTESIAN_POINT('Ctrl Pts',(-1.91596694784064,-1.,-3.4554807430995));
#51737=CARTESIAN_POINT('Ctrl Pts',(-1.91596694784064,1.,-3.4554807430995));
#51738=CARTESIAN_POINT('Ctrl Pts',(-1.92151118213212,-1.,-3.46062821722485));
#51739=CARTESIAN_POINT('Ctrl Pts',(-1.92151118213212,1.,-3.46062821722485));
#51740=CARTESIAN_POINT('Ctrl Pts',(-1.92708888591158,-1.,-3.46573953254084));
#51741=CARTESIAN_POINT('Ctrl Pts',(-1.92708888591158,1.,-3.46573953254084));
#51742=CARTESIAN_POINT('Ctrl Pts',(-1.93270136427081,-1.,-3.47081872409781));
#51743=CARTESIAN_POINT('Ctrl Pts',(-1.93270136427081,1.,-3.47081872409781));
#51744=CARTESIAN_POINT('Ctrl Pts',(-1.93835026973887,-1.,-3.47587040389915));
#51745=CARTESIAN_POINT('Ctrl Pts',(-1.93835026973887,1.,-3.47587040389915));
#51746=CARTESIAN_POINT('Ctrl Pts',(-1.94403680554065,-1.,-3.48089825770416));
#51747=CARTESIAN_POINT('Ctrl Pts',(-1.94403680554065,1.,-3.48089825770416));
#51748=CARTESIAN_POINT('Ctrl Pts',(-1.94976096795911,-1.,-3.48590361610814));
#51749=CARTESIAN_POINT('Ctrl Pts',(-1.94976096795911,1.,-3.48590361610814));
#51750=CARTESIAN_POINT('Ctrl Pts',(-1.95552193112084,-1.,-3.49088618670987));
#51751=CARTESIAN_POINT('Ctrl Pts',(-1.95552193112084,1.,-3.49088618670987));
#51752=CARTESIAN_POINT('Ctrl Pts',(-1.961318367765,-1.,-3.49584466573064));
#51753=CARTESIAN_POINT('Ctrl Pts',(-1.961318367765,1.,-3.49584466573064));
#51754=CARTESIAN_POINT('Ctrl Pts',(-1.96714879724052,-1.,-3.50077740176267));
#51755=CARTESIAN_POINT('Ctrl Pts',(-1.96714879724052,1.,-3.50077740176267));
#51756=CARTESIAN_POINT('Ctrl Pts',(-1.97301191162968,-1.,-3.5056830186108));
#51757=CARTESIAN_POINT('Ctrl Pts',(-1.97301191162968,1.,-3.5056830186108));
#51758=CARTESIAN_POINT('Ctrl Pts',(-1.97890693666288,-1.,-3.51056110478287));
#51759=CARTESIAN_POINT('Ctrl Pts',(-1.97890693666288,1.,-3.51056110478287));
#51760=CARTESIAN_POINT('Ctrl Pts',(-1.9848335106103,-1.,-3.51541198728301));
#51761=CARTESIAN_POINT('Ctrl Pts',(-1.9848335106103,1.,-3.51541198728301));
#51762=CARTESIAN_POINT('Ctrl Pts',(-1.99079153006112,-1.,-3.52023644289142));
#51763=CARTESIAN_POINT('Ctrl Pts',(-1.99079153006112,1.,-3.52023644289142));
#51764=CARTESIAN_POINT('Ctrl Pts',(-1.99678100339296,-1.,-3.52503542491728));
#51765=CARTESIAN_POINT('Ctrl Pts',(-1.99678100339296,1.,-3.52503542491728));
#51766=CARTESIAN_POINT('Ctrl Pts',(-2.00280191090366,-1.,-3.52980980250224));
#51767=CARTESIAN_POINT('Ctrl Pts',(-2.00280191090366,1.,-3.52980980250224));
#51768=CARTESIAN_POINT('Ctrl Pts',(-2.00885403604746,-1.,-3.53456004727424));
#51769=CARTESIAN_POINT('Ctrl Pts',(-2.00885403604746,1.,-3.53456004727424));
#51770=CARTESIAN_POINT('Ctrl Pts',(-2.01493698847351,-1.,-3.53928627453642));
#51771=CARTESIAN_POINT('Ctrl Pts',(-2.01493698847351,1.,-3.53928627453642));
#51772=CARTESIAN_POINT('Ctrl Pts',(-2.02105027983104,-1.,-3.54398838254136));
#51773=CARTESIAN_POINT('Ctrl Pts',(-2.02105027983104,1.,-3.54398838254136));
#51774=CARTESIAN_POINT('Ctrl Pts',(-2.02719338376175,-1.,-3.54866616282227));
#51775=CARTESIAN_POINT('Ctrl Pts',(-2.02719338376175,1.,-3.54866616282227));
#51776=CARTESIAN_POINT('Ctrl Pts',(-2.03336579658133,-1.,-3.55331941293949));
#51777=CARTESIAN_POINT('Ctrl Pts',(-2.03336579658133,1.,-3.55331941293949));
#51778=CARTESIAN_POINT('Ctrl Pts',(-2.03956711119976,-1.,-3.55794807264844));
#51779=CARTESIAN_POINT('Ctrl Pts',(-2.03956711119976,1.,-3.55794807264844));
#51780=CARTESIAN_POINT('Ctrl Pts',(-2.04579702158876,-1.,-3.56255223871505));
#51781=CARTESIAN_POINT('Ctrl Pts',(-2.04579702158876,1.,-3.56255223871505));
#51782=CARTESIAN_POINT('Ctrl Pts',(-2.05205528172911,-1.,-3.56713209977904));
#51783=CARTESIAN_POINT('Ctrl Pts',(-2.05205528172911,1.,-3.56713209977904));
#51784=CARTESIAN_POINT('Ctrl Pts',(-2.05834167687425,-1.,-3.5716878942334));
#51785=CARTESIAN_POINT('Ctrl Pts',(-2.05834167687425,1.,-3.5716878942334));
#51786=CARTESIAN_POINT('Ctrl Pts',(-2.06465599229234,-1.,-3.57621986224402));
#51787=CARTESIAN_POINT('Ctrl Pts',(-2.06465599229234,1.,-3.57621986224402));
#51788=CARTESIAN_POINT('Ctrl Pts',(-2.07099797606,-1.,-3.58072819250872));
#51789=CARTESIAN_POINT('Ctrl Pts',(-2.07099797606,1.,-3.58072819250872));
#51790=CARTESIAN_POINT('Ctrl Pts',(-2.07736732842524,-1.,-3.58521300039988));
#51791=CARTESIAN_POINT('Ctrl Pts',(-2.07736732842524,1.,-3.58521300039988));
#51792=CARTESIAN_POINT('Ctrl Pts',(-2.08376373049196,-1.,-3.58967435355834));
#51793=CARTESIAN_POINT('Ctrl Pts',(-2.08376373049196,1.,-3.58967435355834));
#51794=CARTESIAN_POINT('Ctrl Pts',(-2.09018686331706,-1.,-3.5941122862608));
#51795=CARTESIAN_POINT('Ctrl Pts',(-2.09018686331706,1.,-3.5941122862608));
#51796=CARTESIAN_POINT('Ctrl Pts',(-2.09663642986579,-1.,-3.59852681775396));
#51797=CARTESIAN_POINT('Ctrl Pts',(-2.09663642986579,1.,-3.59852681775396));
#51798=CARTESIAN_POINT('Ctrl Pts',(-2.10311217727687,-1.,-3.60291797087849));
#51799=CARTESIAN_POINT('Ctrl Pts',(-2.10311217727687,1.,-3.60291797087849));
#51800=CARTESIAN_POINT('Ctrl Pts',(-2.10961391333497,-1.,-3.60728578530968));
#51801=CARTESIAN_POINT('Ctrl Pts',(-2.10961391333497,1.,-3.60728578530968));
#51802=CARTESIAN_POINT('Ctrl Pts',(-2.11614149813928,-1.,-3.61163030607452));
#51803=CARTESIAN_POINT('Ctrl Pts',(-2.11614149813928,1.,-3.61163030607452));
#51804=CARTESIAN_POINT('Ctrl Pts',(-2.12138417125349,-1.,-3.61508732215187));
#51805=CARTESIAN_POINT('Ctrl Pts',(-2.12138417125349,1.,-3.61508732215187));
#51806=CARTESIAN_POINT('Ctrl Pts',(-2.12532774376144,-1.,-3.61766963589442));
#51807=CARTESIAN_POINT('Ctrl Pts',(-2.12532774376144,1.,-3.61766963589442));
#51808=CARTESIAN_POINT('Ctrl Pts',(-2.12796193131142,-1.,-3.61938653648716));
#51809=CARTESIAN_POINT('Ctrl Pts',(-2.12796193131142,1.,-3.61938653648716));
#51810=CARTESIAN_POINT('Ctrl Pts',(-2.12928030988903,-1.,-3.62024382630768));
#51811=CARTESIAN_POINT('Ctrl Pts',(-2.12928030988903,1.,-3.62024382630768));
#51812=CARTESIAN_POINT('',(-1.78327315618341,1.,-3.29885386921514));
#51813=CARTESIAN_POINT('Ctrl Pts',(-1.78327315618341,-1.,-3.29885386921513));
#51814=CARTESIAN_POINT('Ctrl Pts',(-1.78327315618341,-0.666666666666667,
-3.29885386921513));
#51815=CARTESIAN_POINT('Ctrl Pts',(-1.78327315618341,-0.333333333333333,
-3.29885386921513));
#51816=CARTESIAN_POINT('Ctrl Pts',(-1.78327315618341,0.333333333333333,
-3.29885386921513));
#51817=CARTESIAN_POINT('Ctrl Pts',(-1.78327315618341,0.666666666666667,
-3.29885386921513));
#51818=CARTESIAN_POINT('Ctrl Pts',(-1.78327315618341,1.,-3.29885386921513));
#51819=CARTESIAN_POINT('',(-2.12928030988903,1.,-3.62024382630768));
#51820=CARTESIAN_POINT('',(-2.12928030988903,0.,-3.62024382630768));
#51821=CARTESIAN_POINT('Ctrl Pts',(-1.78327315618341,1.,-3.29885386921514));
#51822=CARTESIAN_POINT('Ctrl Pts',(-1.78326534445518,1.,-3.29890219175423));
#51823=CARTESIAN_POINT('Ctrl Pts',(-1.78329283591905,1.,-3.29909749657808));
#51824=CARTESIAN_POINT('Ctrl Pts',(-1.78353803106924,1.,-3.299705498242));
#51825=CARTESIAN_POINT('Ctrl Pts',(-1.78432384788174,1.,-3.30119637003394));
#51826=CARTESIAN_POINT('Ctrl Pts',(-1.78610045419846,1.,-3.30422155559112));
#51827=CARTESIAN_POINT('Ctrl Pts',(-1.78888832245873,1.,-3.30873412266788));
#51828=CARTESIAN_POINT('Ctrl Pts',(-1.79242331349949,1.,-3.31428038326424));
#51829=CARTESIAN_POINT('Ctrl Pts',(-1.79652817033251,1.,-3.3205535510082));
#51830=CARTESIAN_POINT('Ctrl Pts',(-1.80100380443406,1.,-3.32721088039578));
#51831=CARTESIAN_POINT('Ctrl Pts',(-1.80565802981102,1.,-3.33392460276808));
#51832=CARTESIAN_POINT('Ctrl Pts',(-1.81033399625352,1.,-3.34043216147606));
#51833=CARTESIAN_POINT('Ctrl Pts',(-1.81494618732853,1.,-3.34660014370673));
#51834=CARTESIAN_POINT('Ctrl Pts',(-1.81948458796829,1.,-3.35243086937598));
#51835=CARTESIAN_POINT('Ctrl Pts',(-1.82398496829301,1.,-3.35800801557424));
#51836=CARTESIAN_POINT('Ctrl Pts',(-1.82850752153199,1.,-3.36345722124158));
#51837=CARTESIAN_POINT('Ctrl Pts',(-1.83311391452322,1.,-3.36890396271836));
#51838=CARTESIAN_POINT('Ctrl Pts',(-1.83784072967077,1.,-3.37442462015853));
#51839=CARTESIAN_POINT('Ctrl Pts',(-1.84269016931643,1.,-3.38002968341157));
#51840=CARTESIAN_POINT('Ctrl Pts',(-1.84764441927753,1.,-3.38569092349592));
#51841=CARTESIAN_POINT('Ctrl Pts',(-1.85267433291769,1.,-3.39135802549398));
#51842=CARTESIAN_POINT('Ctrl Pts',(-1.85774972037062,1.,-3.39697816833067));
#51843=CARTESIAN_POINT('Ctrl Pts',(-1.86285057051245,1.,-3.40251742305476));
#51844=CARTESIAN_POINT('Ctrl Pts',(-1.86797231196654,1.,-3.40797080000549));
#51845=CARTESIAN_POINT('Ctrl Pts',(-1.87311957248121,1.,-3.41335043875209));
#51846=CARTESIAN_POINT('Ctrl Pts',(-1.87830245689344,1.,-3.41867858383771));
#51847=CARTESIAN_POINT('Ctrl Pts',(-1.8835320506206,1.,-3.42397908819736));
#51848=CARTESIAN_POINT('Ctrl Pts',(-1.88881571322009,1.,-3.42926852222158));
#51849=CARTESIAN_POINT('Ctrl Pts',(-1.89415420002542,1.,-3.43455074411571));
#51850=CARTESIAN_POINT('Ctrl Pts',(-1.89954426803384,1.,-3.4398218567809));
#51851=CARTESIAN_POINT('Ctrl Pts',(-1.90498026502305,1.,-3.44507323983367));
#51852=CARTESIAN_POINT('Ctrl Pts',(-1.91045605593639,1.,-3.45029522038888));
#51853=CARTESIAN_POINT('Ctrl Pts',(-1.91596694784064,1.,-3.4554807430995));
#51854=CARTESIAN_POINT('Ctrl Pts',(-1.92151118213212,1.,-3.46062821722485));
#51855=CARTESIAN_POINT('Ctrl Pts',(-1.92708888591158,1.,-3.46573953254084));
#51856=CARTESIAN_POINT('Ctrl Pts',(-1.93270136427081,1.,-3.47081872409781));
#51857=CARTESIAN_POINT('Ctrl Pts',(-1.93835026973887,1.,-3.47587040389915));
#51858=CARTESIAN_POINT('Ctrl Pts',(-1.94403680554065,1.,-3.48089825770416));
#51859=CARTESIAN_POINT('Ctrl Pts',(-1.94976096795911,1.,-3.48590361610814));
#51860=CARTESIAN_POINT('Ctrl Pts',(-1.95552193112084,1.,-3.49088618670987));
#51861=CARTESIAN_POINT('Ctrl Pts',(-1.961318367765,1.,-3.49584466573064));
#51862=CARTESIAN_POINT('Ctrl Pts',(-1.96714879724052,1.,-3.50077740176267));
#51863=CARTESIAN_POINT('Ctrl Pts',(-1.97301191162968,1.,-3.5056830186108));
#51864=CARTESIAN_POINT('Ctrl Pts',(-1.97890693666288,1.,-3.51056110478287));
#51865=CARTESIAN_POINT('Ctrl Pts',(-1.9848335106103,1.,-3.51541198728301));
#51866=CARTESIAN_POINT('Ctrl Pts',(-1.99079153006112,1.,-3.52023644289142));
#51867=CARTESIAN_POINT('Ctrl Pts',(-1.99678100339296,1.,-3.52503542491728));
#51868=CARTESIAN_POINT('Ctrl Pts',(-2.00280191090366,1.,-3.52980980250224));
#51869=CARTESIAN_POINT('Ctrl Pts',(-2.00885403604746,1.,-3.53456004727424));
#51870=CARTESIAN_POINT('Ctrl Pts',(-2.01493698847351,1.,-3.53928627453642));
#51871=CARTESIAN_POINT('Ctrl Pts',(-2.02105027983104,1.,-3.54398838254136));
#51872=CARTESIAN_POINT('Ctrl Pts',(-2.02719338376175,1.,-3.54866616282227));
#51873=CARTESIAN_POINT('Ctrl Pts',(-2.03336579658133,1.,-3.55331941293949));
#51874=CARTESIAN_POINT('Ctrl Pts',(-2.03956711119976,1.,-3.55794807264844));
#51875=CARTESIAN_POINT('Ctrl Pts',(-2.04579702158876,1.,-3.56255223871505));
#51876=CARTESIAN_POINT('Ctrl Pts',(-2.05205528172911,1.,-3.56713209977904));
#51877=CARTESIAN_POINT('Ctrl Pts',(-2.05834167687425,1.,-3.5716878942334));
#51878=CARTESIAN_POINT('Ctrl Pts',(-2.06465599229234,1.,-3.57621986224402));
#51879=CARTESIAN_POINT('Ctrl Pts',(-2.07099797606,1.,-3.58072819250872));
#51880=CARTESIAN_POINT('Ctrl Pts',(-2.07736732842524,1.,-3.58521300039988));
#51881=CARTESIAN_POINT('Ctrl Pts',(-2.08376373049196,1.,-3.58967435355834));
#51882=CARTESIAN_POINT('Ctrl Pts',(-2.09018686331706,1.,-3.5941122862608));
#51883=CARTESIAN_POINT('Ctrl Pts',(-2.09663642986579,1.,-3.59852681775396));
#51884=CARTESIAN_POINT('Ctrl Pts',(-2.10311217727687,1.,-3.60291797087849));
#51885=CARTESIAN_POINT('Ctrl Pts',(-2.10961391333497,1.,-3.60728578530968));
#51886=CARTESIAN_POINT('Ctrl Pts',(-2.11614149813928,1.,-3.61163030607452));
#51887=CARTESIAN_POINT('Ctrl Pts',(-2.12138417125349,1.,-3.61508732215187));
#51888=CARTESIAN_POINT('Ctrl Pts',(-2.12532774376144,1.,-3.61766963589442));
#51889=CARTESIAN_POINT('Ctrl Pts',(-2.12796193131142,1.,-3.61938653648716));
#51890=CARTESIAN_POINT('Ctrl Pts',(-2.12928030988903,1.,-3.62024382630768));
#51891=CARTESIAN_POINT('Origin',(-2.12928030988903,0.,-3.62024382630768));
#51892=CARTESIAN_POINT('',(-2.25898783642071,1.,-3.54075895182139));
#51893=CARTESIAN_POINT('Origin',(0.,0.,0.));
#51894=CARTESIAN_POINT('',(-1.62064718014256,1.,-3.38171594275687));
#51895=CARTESIAN_POINT('Origin',(0.,1.,0.));
#51896=CARTESIAN_POINT('Ctrl Pts',(-1.62064718014256,1.,-3.38171594275687));
#51897=CARTESIAN_POINT('Ctrl Pts',(-1.62064718014256,0.666666666666667,
-3.38171594275687));
#51898=CARTESIAN_POINT('Ctrl Pts',(-1.62064718014256,0.333333333333333,
-3.38171594275687));
#51899=CARTESIAN_POINT('Ctrl Pts',(-1.62064718014256,-0.333333333333333,
-3.38171594275687));
#51900=CARTESIAN_POINT('Ctrl Pts',(-1.62064718014256,-0.666666666666667,
-3.38171594275687));
#51901=CARTESIAN_POINT('Ctrl Pts',(-1.62064718014256,-1.,-3.38171594275687));
#51902=CARTESIAN_POINT('Ctrl Pts',(-1.67727921511438,-1.,-3.85054988729471));
#51903=CARTESIAN_POINT('Ctrl Pts',(-1.67727921511438,1.,-3.85054988729471));
#51904=CARTESIAN_POINT('Ctrl Pts',(-1.6773605765671,-1.,-3.84897939431104));
#51905=CARTESIAN_POINT('Ctrl Pts',(-1.6773605765671,1.,-3.84897939431104));
#51906=CARTESIAN_POINT('Ctrl Pts',(-1.67751991140661,-1.,-3.84583912297567));
#51907=CARTESIAN_POINT('Ctrl Pts',(-1.67751991140661,1.,-3.84583912297567));
#51908=CARTESIAN_POINT('Ctrl Pts',(-1.67774874946867,-1.,-3.8411308598706));
#51909=CARTESIAN_POINT('Ctrl Pts',(-1.67774874946867,1.,-3.8411308598706));
#51910=CARTESIAN_POINT('Ctrl Pts',(-1.67803353065273,-1.,-3.83485746516115));
#51911=CARTESIAN_POINT('Ctrl Pts',(-1.67803353065273,1.,-3.83485746516115));
#51912=CARTESIAN_POINT('Ctrl Pts',(-1.67835555760094,-1.,-3.82702289288453));
#51913=CARTESIAN_POINT('Ctrl Pts',(-1.67835555760094,1.,-3.82702289288453));
#51914=CARTESIAN_POINT('Ctrl Pts',(-1.67864354606363,-1.,-3.81919554100522));
#51915=CARTESIAN_POINT('Ctrl Pts',(-1.67864354606363,1.,-3.81919554100522));
#51916=CARTESIAN_POINT('Ctrl Pts',(-1.67889737738311,-1.,-3.81137549624273));
#51917=CARTESIAN_POINT('Ctrl Pts',(-1.67889737738311,1.,-3.81137549624273));
#51918=CARTESIAN_POINT('Ctrl Pts',(-1.67911690648128,-1.,-3.80356289078481));
#51919=CARTESIAN_POINT('Ctrl Pts',(-1.67911690648128,1.,-3.80356289078481));
#51920=CARTESIAN_POINT('Ctrl Pts',(-1.67930196625203,-1.,-3.7957579157763));
#51921=CARTESIAN_POINT('Ctrl Pts',(-1.67930196625203,1.,-3.7957579157763));
#51922=CARTESIAN_POINT('Ctrl Pts',(-1.67945236653175,-1.,-3.78796080021026));
#51923=CARTESIAN_POINT('Ctrl Pts',(-1.67945236653175,1.,-3.78796080021026));
#51924=CARTESIAN_POINT('Ctrl Pts',(-1.67956789211943,-1.,-3.78017178196859));
#51925=CARTESIAN_POINT('Ctrl Pts',(-1.67956789211943,1.,-3.78017178196859));
#51926=CARTESIAN_POINT('Ctrl Pts',(-1.67964830084946,-1.,-3.77239107928394));
#51927=CARTESIAN_POINT('Ctrl Pts',(-1.67964830084946,1.,-3.77239107928394));
#51928=CARTESIAN_POINT('Ctrl Pts',(-1.67969332319322,-1.,-3.76461886684523));
#51929=CARTESIAN_POINT('Ctrl Pts',(-1.67969332319322,1.,-3.76461886684523));
#51930=CARTESIAN_POINT('Ctrl Pts',(-1.67970265841379,-1.,-3.75685523754816));
#51931=CARTESIAN_POINT('Ctrl Pts',(-1.67970265841379,1.,-3.75685523754816));
#51932=CARTESIAN_POINT('Ctrl Pts',(-1.67967598599665,-1.,-3.74910022394845));
#51933=CARTESIAN_POINT('Ctrl Pts',(-1.67967598599665,1.,-3.74910022394845));
#51934=CARTESIAN_POINT('Ctrl Pts',(-1.67961298685316,-1.,-3.74135385965622));
#51935=CARTESIAN_POINT('Ctrl Pts',(-1.67961298685316,1.,-3.74135385965622));
#51936=CARTESIAN_POINT('Ctrl Pts',(-1.67951336376434,-1.,-3.73361623282617));
#51937=CARTESIAN_POINT('Ctrl Pts',(-1.67951336376434,1.,-3.73361623282617));
#51938=CARTESIAN_POINT('Ctrl Pts',(-1.67937685856627,-1.,-3.72588753416339));
#51939=CARTESIAN_POINT('Ctrl Pts',(-1.67937685856627,1.,-3.72588753416339));
#51940=CARTESIAN_POINT('Ctrl Pts',(-1.6792032807165,-1.,-3.71816812842188));
#51941=CARTESIAN_POINT('Ctrl Pts',(-1.6792032807165,1.,-3.71816812842188));
#51942=CARTESIAN_POINT('Ctrl Pts',(-1.67899249793398,-1.,-3.71045854208195));
#51943=CARTESIAN_POINT('Ctrl Pts',(-1.67899249793398,1.,-3.71045854208195));
#51944=CARTESIAN_POINT('Ctrl Pts',(-1.6787443694862,-1.,-3.70275932350998));
#51945=CARTESIAN_POINT('Ctrl Pts',(-1.6787443694862,1.,-3.70275932350998));
#51946=CARTESIAN_POINT('Ctrl Pts',(-1.67845869064304,-1.,-3.69507092759545));
#51947=CARTESIAN_POINT('Ctrl Pts',(-1.67845869064304,1.,-3.69507092759545));
#51948=CARTESIAN_POINT('Ctrl Pts',(-1.67813513867973,-1.,-3.68739360236505));
#51949=CARTESIAN_POINT('Ctrl Pts',(-1.67813513867973,1.,-3.68739360236505));
#51950=CARTESIAN_POINT('Ctrl Pts',(-1.67777320475872,-1.,-3.6797272457918));
#51951=CARTESIAN_POINT('Ctrl Pts',(-1.67777320475872,1.,-3.6797272457918));
#51952=CARTESIAN_POINT('Ctrl Pts',(-1.67737217414901,-1.,-3.67207136294639));
#51953=CARTESIAN_POINT('Ctrl Pts',(-1.67737217414901,1.,-3.67207136294639));
#51954=CARTESIAN_POINT('Ctrl Pts',(-1.67693128053153,-1.,-3.66442538671018));
#51955=CARTESIAN_POINT('Ctrl Pts',(-1.67693128053153,1.,-3.66442538671018));
#51956=CARTESIAN_POINT('Ctrl Pts',(-1.67644983469459,-1.,-3.65678894416442));
#51957=CARTESIAN_POINT('Ctrl Pts',(-1.67644983469459,1.,-3.65678894416442));
#51958=CARTESIAN_POINT('Ctrl Pts',(-1.6759273594669,-1.,-3.64916213574663));
#51959=CARTESIAN_POINT('Ctrl Pts',(-1.6759273594669,1.,-3.64916213574663));
#51960=CARTESIAN_POINT('Ctrl Pts',(-1.67536373264839,-1.,-3.6415458297232));
#51961=CARTESIAN_POINT('Ctrl Pts',(-1.67536373264839,1.,-3.6415458297232));
#51962=CARTESIAN_POINT('Ctrl Pts',(-1.67475929882962,-1.,-3.63394189312902));
#51963=CARTESIAN_POINT('Ctrl Pts',(-1.67475929882962,1.,-3.63394189312902));
#51964=CARTESIAN_POINT('Ctrl Pts',(-1.67411452372265,-1.,-3.62635249450908));
#51965=CARTESIAN_POINT('Ctrl Pts',(-1.67411452372265,1.,-3.62635249450908));
#51966=CARTESIAN_POINT('Ctrl Pts',(-1.67342968196223,-1.,-3.61877947398179));
#51967=CARTESIAN_POINT('Ctrl Pts',(-1.67342968196223,1.,-3.61877947398179));
#51968=CARTESIAN_POINT('Ctrl Pts',(-1.67270452466968,-1.,-3.61122367156182));
#51969=CARTESIAN_POINT('Ctrl Pts',(-1.67270452466968,1.,-3.61122367156182));
#51970=CARTESIAN_POINT('Ctrl Pts',(-1.67193797318598,-1.,-3.60368430815203));
#51971=CARTESIAN_POINT('Ctrl Pts',(-1.67193797318598,1.,-3.60368430815203));
#51972=CARTESIAN_POINT('Ctrl Pts',(-1.67112775290706,-1.,-3.59615824388808));
#51973=CARTESIAN_POINT('Ctrl Pts',(-1.67112775290706,1.,-3.59615824388808));
#51974=CARTESIAN_POINT('Ctrl Pts',(-1.67027110397601,-1.,-3.5886414309783));
#51975=CARTESIAN_POINT('Ctrl Pts',(-1.67027110397601,1.,-3.5886414309783));
#51976=CARTESIAN_POINT('Ctrl Pts',(-1.66936552908228,-1.,-3.58113044183823));
#51977=CARTESIAN_POINT('Ctrl Pts',(-1.66936552908228,1.,-3.58113044183823));
#51978=CARTESIAN_POINT('Ctrl Pts',(-1.66840957407299,-1.,-3.57362406285884));
#51979=CARTESIAN_POINT('Ctrl Pts',(-1.66840957407299,1.,-3.57362406285884));
#51980=CARTESIAN_POINT('Ctrl Pts',(-1.66740349220308,-1.,-3.56612465179429));
#51981=CARTESIAN_POINT('Ctrl Pts',(-1.66740349220308,1.,-3.56612465179429));
#51982=CARTESIAN_POINT('Ctrl Pts',(-1.66635023293121,-1.,-3.55864015233617));
#51983=CARTESIAN_POINT('Ctrl Pts',(-1.66635023293121,1.,-3.55864015233617));
#51984=CARTESIAN_POINT('Ctrl Pts',(-1.66525401569004,-1.,-3.5511812134288));
#51985=CARTESIAN_POINT('Ctrl Pts',(-1.66525401569004,1.,-3.5511812134288));
#51986=CARTESIAN_POINT('Ctrl Pts',(-1.66411849222334,-1.,-3.5437574747503));
#51987=CARTESIAN_POINT('Ctrl Pts',(-1.66411849222334,1.,-3.5437574747503));
#51988=CARTESIAN_POINT('Ctrl Pts',(-1.66294490916113,-1.,-3.53637385060225));
#51989=CARTESIAN_POINT('Ctrl Pts',(-1.66294490916113,1.,-3.53637385060225));
#51990=CARTESIAN_POINT('Ctrl Pts',(-1.66173058912365,-1.,-3.52902746211081));
#51991=CARTESIAN_POINT('Ctrl Pts',(-1.66173058912365,1.,-3.52902746211081));
#51992=CARTESIAN_POINT('Ctrl Pts',(-1.66046645222266,-1.,-3.52170261543787));
#51993=CARTESIAN_POINT('Ctrl Pts',(-1.66046645222266,1.,-3.52170261543787));
#51994=CARTESIAN_POINT('Ctrl Pts',(-1.65913971687324,-1.,-3.51437632188903));
#51995=CARTESIAN_POINT('Ctrl Pts',(-1.65913971687324,1.,-3.51437632188903));
#51996=CARTESIAN_POINT('Ctrl Pts',(-1.65773832633617,-1.,-3.5070273314651));
#51997=CARTESIAN_POINT('Ctrl Pts',(-1.65773832633617,1.,-3.5070273314651));
#51998=CARTESIAN_POINT('Ctrl Pts',(-1.65625517961583,-1.,-3.49964476477929));
#51999=CARTESIAN_POINT('Ctrl Pts',(-1.65625517961583,1.,-3.49964476477929));
#52000=CARTESIAN_POINT('Ctrl Pts',(-1.65469162644476,-1.,-3.49223525300194));
#52001=CARTESIAN_POINT('Ctrl Pts',(-1.65469162644476,1.,-3.49223525300194));
#52002=CARTESIAN_POINT('Ctrl Pts',(-1.65306335367762,-1.,-3.48483492840942));
#52003=CARTESIAN_POINT('Ctrl Pts',(-1.65306335367762,1.,-3.48483492840942));
#52004=CARTESIAN_POINT('Ctrl Pts',(-1.65139534930353,-1.,-3.47749926256543));
#52005=CARTESIAN_POINT('Ctrl Pts',(-1.65139534930353,1.,-3.47749926256543));
#52006=CARTESIAN_POINT('Ctrl Pts',(-1.64971118698285,-1.,-3.47028140996055));
#52007=CARTESIAN_POINT('Ctrl Pts',(-1.64971118698285,1.,-3.47028140996055));
#52008=CARTESIAN_POINT('Ctrl Pts',(-1.64802323352752,-1.,-3.46321237515029));
#52009=CARTESIAN_POINT('Ctrl Pts',(-1.64802323352752,1.,-3.46321237515029));
#52010=CARTESIAN_POINT('Ctrl Pts',(-1.64632429697506,-1.,-3.4562842106239));
#52011=CARTESIAN_POINT('Ctrl Pts',(-1.64632429697506,1.,-3.4562842106239));
#52012=CARTESIAN_POINT('Ctrl Pts',(-1.64457408708059,-1.,-3.44942242546693));
#52013=CARTESIAN_POINT('Ctrl Pts',(-1.64457408708059,1.,-3.44942242546693));
#52014=CARTESIAN_POINT('Ctrl Pts',(-1.64270733821042,-1.,-3.44250337701736));
#52015=CARTESIAN_POINT('Ctrl Pts',(-1.64270733821042,1.,-3.44250337701736));
#52016=CARTESIAN_POINT('Ctrl Pts',(-1.64065778701952,-1.,-3.43540451921397));
#52017=CARTESIAN_POINT('Ctrl Pts',(-1.64065778701952,1.,-3.43540451921397));
#52018=CARTESIAN_POINT('Ctrl Pts',(-1.6383787624689,-1.,-3.42804772926213));
#52019=CARTESIAN_POINT('Ctrl Pts',(-1.6383787624689,1.,-3.42804772926213));
#52020=CARTESIAN_POINT('Ctrl Pts',(-1.63586250099804,-1.,-3.4204397459095));
#52021=CARTESIAN_POINT('Ctrl Pts',(-1.63586250099804,1.,-3.4204397459095));
#52022=CARTESIAN_POINT('Ctrl Pts',(-1.63316667054156,-1.,-3.41272817148719));
#52023=CARTESIAN_POINT('Ctrl Pts',(-1.63316667054156,1.,-3.41272817148719));
#52024=CARTESIAN_POINT('Ctrl Pts',(-1.63041148964996,-1.,-3.40519422740596));
#52025=CARTESIAN_POINT('Ctrl Pts',(-1.63041148964996,1.,-3.40519422740596));
#52026=CARTESIAN_POINT('Ctrl Pts',(-1.62774916464571,-1.,-3.39818605298342));
#52027=CARTESIAN_POINT('Ctrl Pts',(-1.62774916464571,1.,-3.39818605298342));
#52028=CARTESIAN_POINT('Ctrl Pts',(-1.62533996116793,-1.,-3.39206617497078));
#52029=CARTESIAN_POINT('Ctrl Pts',(-1.62533996116793,1.,-3.39206617497078));
#52030=CARTESIAN_POINT('Ctrl Pts',(-1.62332788556183,-1.,-3.38715832178929));
#52031=CARTESIAN_POINT('Ctrl Pts',(-1.62332788556183,1.,-3.38715832178929));
#52032=CARTESIAN_POINT('Ctrl Pts',(-1.62181089631134,-1.,-3.38368201668123));
#52033=CARTESIAN_POINT('Ctrl Pts',(-1.62181089631134,1.,-3.38368201668123));
#52034=CARTESIAN_POINT('Ctrl Pts',(-1.62103022180917,-1.,-3.38212861099481));
#52035=CARTESIAN_POINT('Ctrl Pts',(-1.62103022180917,1.,-3.38212861099481));
#52036=CARTESIAN_POINT('Ctrl Pts',(-1.6206953236804,-1.,-3.38166984193496));
#52037=CARTESIAN_POINT('Ctrl Pts',(-1.6206953236804,1.,-3.38166984193496));
#52038=CARTESIAN_POINT('Ctrl Pts',(-1.62058335162421,-1.,-3.38167767992546));
#52039=CARTESIAN_POINT('Ctrl Pts',(-1.62058335162421,1.,-3.38167767992546));
#52040=CARTESIAN_POINT('Ctrl Pts',(-1.62055519152809,-1.,-3.38176002566879));
#52041=CARTESIAN_POINT('Ctrl Pts',(-1.62055519152809,1.,-3.38176002566879));
#52042=CARTESIAN_POINT('',(-1.67727921511438,1.,-3.85054988729471));
#52043=CARTESIAN_POINT('Ctrl Pts',(-1.67727921511438,1.,-3.85054988729471));
#52044=CARTESIAN_POINT('Ctrl Pts',(-1.6773605765671,1.,-3.84897939431104));
#52045=CARTESIAN_POINT('Ctrl Pts',(-1.67751991140661,1.,-3.84583912297567));
#52046=CARTESIAN_POINT('Ctrl Pts',(-1.67774874946867,1.,-3.8411308598706));
#52047=CARTESIAN_POINT('Ctrl Pts',(-1.67803353065273,1.,-3.83485746516115));
#52048=CARTESIAN_POINT('Ctrl Pts',(-1.67835555760094,1.,-3.82702289288453));
#52049=CARTESIAN_POINT('Ctrl Pts',(-1.67864354606363,1.,-3.81919554100522));
#52050=CARTESIAN_POINT('Ctrl Pts',(-1.67889737738311,1.,-3.81137549624273));
#52051=CARTESIAN_POINT('Ctrl Pts',(-1.67911690648128,1.,-3.80356289078481));
#52052=CARTESIAN_POINT('Ctrl Pts',(-1.67930196625203,1.,-3.7957579157763));
#52053=CARTESIAN_POINT('Ctrl Pts',(-1.67945236653175,1.,-3.78796080021026));
#52054=CARTESIAN_POINT('Ctrl Pts',(-1.67956789211943,1.,-3.78017178196859));
#52055=CARTESIAN_POINT('Ctrl Pts',(-1.67964830084946,1.,-3.77239107928394));
#52056=CARTESIAN_POINT('Ctrl Pts',(-1.67969332319322,1.,-3.76461886684523));
#52057=CARTESIAN_POINT('Ctrl Pts',(-1.67970265841379,1.,-3.75685523754816));
#52058=CARTESIAN_POINT('Ctrl Pts',(-1.67967598599665,1.,-3.74910022394845));
#52059=CARTESIAN_POINT('Ctrl Pts',(-1.67961298685316,1.,-3.74135385965622));
#52060=CARTESIAN_POINT('Ctrl Pts',(-1.67951336376434,1.,-3.73361623282617));
#52061=CARTESIAN_POINT('Ctrl Pts',(-1.67937685856627,1.,-3.72588753416339));
#52062=CARTESIAN_POINT('Ctrl Pts',(-1.6792032807165,1.,-3.71816812842188));
#52063=CARTESIAN_POINT('Ctrl Pts',(-1.67899249793398,1.,-3.71045854208195));
#52064=CARTESIAN_POINT('Ctrl Pts',(-1.6787443694862,1.,-3.70275932350998));
#52065=CARTESIAN_POINT('Ctrl Pts',(-1.67845869064304,1.,-3.69507092759545));
#52066=CARTESIAN_POINT('Ctrl Pts',(-1.67813513867973,1.,-3.68739360236505));
#52067=CARTESIAN_POINT('Ctrl Pts',(-1.67777320475872,1.,-3.6797272457918));
#52068=CARTESIAN_POINT('Ctrl Pts',(-1.67737217414901,1.,-3.67207136294639));
#52069=CARTESIAN_POINT('Ctrl Pts',(-1.67693128053153,1.,-3.66442538671018));
#52070=CARTESIAN_POINT('Ctrl Pts',(-1.67644983469459,1.,-3.65678894416442));
#52071=CARTESIAN_POINT('Ctrl Pts',(-1.6759273594669,1.,-3.64916213574663));
#52072=CARTESIAN_POINT('Ctrl Pts',(-1.67536373264839,1.,-3.6415458297232));
#52073=CARTESIAN_POINT('Ctrl Pts',(-1.67475929882962,1.,-3.63394189312902));
#52074=CARTESIAN_POINT('Ctrl Pts',(-1.67411452372265,1.,-3.62635249450908));
#52075=CARTESIAN_POINT('Ctrl Pts',(-1.67342968196223,1.,-3.61877947398179));
#52076=CARTESIAN_POINT('Ctrl Pts',(-1.67270452466968,1.,-3.61122367156182));
#52077=CARTESIAN_POINT('Ctrl Pts',(-1.67193797318598,1.,-3.60368430815203));
#52078=CARTESIAN_POINT('Ctrl Pts',(-1.67112775290706,1.,-3.59615824388808));
#52079=CARTESIAN_POINT('Ctrl Pts',(-1.67027110397601,1.,-3.5886414309783));
#52080=CARTESIAN_POINT('Ctrl Pts',(-1.66936552908228,1.,-3.58113044183823));
#52081=CARTESIAN_POINT('Ctrl Pts',(-1.66840957407299,1.,-3.57362406285884));
#52082=CARTESIAN_POINT('Ctrl Pts',(-1.66740349220308,1.,-3.56612465179429));
#52083=CARTESIAN_POINT('Ctrl Pts',(-1.66635023293121,1.,-3.55864015233617));
#52084=CARTESIAN_POINT('Ctrl Pts',(-1.66525401569004,1.,-3.5511812134288));
#52085=CARTESIAN_POINT('Ctrl Pts',(-1.66411849222334,1.,-3.5437574747503));
#52086=CARTESIAN_POINT('Ctrl Pts',(-1.66294490916113,1.,-3.53637385060225));
#52087=CARTESIAN_POINT('Ctrl Pts',(-1.66173058912365,1.,-3.52902746211081));
#52088=CARTESIAN_POINT('Ctrl Pts',(-1.66046645222266,1.,-3.52170261543787));
#52089=CARTESIAN_POINT('Ctrl Pts',(-1.65913971687324,1.,-3.51437632188903));
#52090=CARTESIAN_POINT('Ctrl Pts',(-1.65773832633617,1.,-3.5070273314651));
#52091=CARTESIAN_POINT('Ctrl Pts',(-1.65625517961583,1.,-3.49964476477929));
#52092=CARTESIAN_POINT('Ctrl Pts',(-1.65469162644476,1.,-3.49223525300194));
#52093=CARTESIAN_POINT('Ctrl Pts',(-1.65306335367762,1.,-3.48483492840942));
#52094=CARTESIAN_POINT('Ctrl Pts',(-1.65139534930353,1.,-3.47749926256543));
#52095=CARTESIAN_POINT('Ctrl Pts',(-1.64971118698285,1.,-3.47028140996055));
#52096=CARTESIAN_POINT('Ctrl Pts',(-1.64802323352752,1.,-3.46321237515029));
#52097=CARTESIAN_POINT('Ctrl Pts',(-1.64632429697506,1.,-3.4562842106239));
#52098=CARTESIAN_POINT('Ctrl Pts',(-1.64457408708059,1.,-3.44942242546693));
#52099=CARTESIAN_POINT('Ctrl Pts',(-1.64270733821042,1.,-3.44250337701736));
#52100=CARTESIAN_POINT('Ctrl Pts',(-1.64065778701952,1.,-3.43540451921397));
#52101=CARTESIAN_POINT('Ctrl Pts',(-1.6383787624689,1.,-3.42804772926213));
#52102=CARTESIAN_POINT('Ctrl Pts',(-1.63586250099804,1.,-3.4204397459095));
#52103=CARTESIAN_POINT('Ctrl Pts',(-1.63316667054156,1.,-3.41272817148719));
#52104=CARTESIAN_POINT('Ctrl Pts',(-1.63041148964996,1.,-3.40519422740596));
#52105=CARTESIAN_POINT('Ctrl Pts',(-1.62774916464571,1.,-3.39818605298342));
#52106=CARTESIAN_POINT('Ctrl Pts',(-1.62533996116793,1.,-3.39206617497078));
#52107=CARTESIAN_POINT('Ctrl Pts',(-1.62332788556183,1.,-3.38715832178929));
#52108=CARTESIAN_POINT('Ctrl Pts',(-1.62192472202795,1.,-3.3839428576331));
#52109=CARTESIAN_POINT('Ctrl Pts',(-1.62118047294574,1.,-3.38243080602536));
#52110=CARTESIAN_POINT('Ctrl Pts',(-1.62083271136059,1.,-3.38187506457001));
#52111=CARTESIAN_POINT('Ctrl Pts',(-1.62069086551626,1.,-3.38173802621243));
#52112=CARTESIAN_POINT('Ctrl Pts',(-1.62064718014256,1.,-3.38171594275687));
#52113=CARTESIAN_POINT('',(-1.67727921511438,0.,-3.85054988729471));
#52114=CARTESIAN_POINT('Ctrl Pts',(-1.24535988127942,-1.,-3.53717101171257));
#52115=CARTESIAN_POINT('Ctrl Pts',(-1.24535988127942,1.,-3.53717101171257));
#52116=CARTESIAN_POINT('Ctrl Pts',(-1.24528174185147,-1.,-3.53713269667534));
#52117=CARTESIAN_POINT('Ctrl Pts',(-1.24528174185147,1.,-3.53713269667534));
#52118=CARTESIAN_POINT('Ctrl Pts',(-1.2451970233558,-1.,-3.53720633058152));
#52119=CARTESIAN_POINT('Ctrl Pts',(-1.2451970233558,1.,-3.53720633058152));
#52120=CARTESIAN_POINT('Ctrl Pts',(-1.24528461333177,-1.,-3.53776753803428));
#52121=CARTESIAN_POINT('Ctrl Pts',(-1.24528461333177,1.,-3.53776753803428));
#52122=CARTESIAN_POINT('Ctrl Pts',(-1.24583101679199,-1.,-3.53941798196293));
#52123=CARTESIAN_POINT('Ctrl Pts',(-1.24583101679199,1.,-3.53941798196293));
#52124=CARTESIAN_POINT('Ctrl Pts',(-1.2472164623202,-1.,-3.54294877426113));
#52125=CARTESIAN_POINT('Ctrl Pts',(-1.2472164623202,1.,-3.54294877426113));
#52126=CARTESIAN_POINT('Ctrl Pts',(-1.24926408627938,-1.,-3.54784190282889));
#52127=CARTESIAN_POINT('Ctrl Pts',(-1.24926408627938,1.,-3.54784190282889));
#52128=CARTESIAN_POINT('Ctrl Pts',(-1.25188792940508,-1.,-3.5538728741862));
#52129=CARTESIAN_POINT('Ctrl Pts',(-1.25188792940508,1.,-3.5538728741862));
#52130=CARTESIAN_POINT('Ctrl Pts',(-1.25496090899873,-1.,-3.56071094990825));
#52131=CARTESIAN_POINT('Ctrl Pts',(-1.25496090899873,1.,-3.56071094990825));
#52132=CARTESIAN_POINT('Ctrl Pts',(-1.25834000485626,-1.,-3.56798645995025));
#52133=CARTESIAN_POINT('Ctrl Pts',(-1.25834000485626,1.,-3.56798645995025));
#52134=CARTESIAN_POINT('Ctrl Pts',(-1.26188667142784,-1.,-3.5753456065164));
#52135=CARTESIAN_POINT('Ctrl Pts',(-1.26188667142784,1.,-3.5753456065164));
#52136=CARTESIAN_POINT('Ctrl Pts',(-1.26548706249891,-1.,-3.58250452868699));
#52137=CARTESIAN_POINT('Ctrl Pts',(-1.26548706249891,1.,-3.58250452868699));
#52138=CARTESIAN_POINT('Ctrl Pts',(-1.26907758484766,-1.,-3.5893180784647));
#52139=CARTESIAN_POINT('Ctrl Pts',(-1.26907758484766,1.,-3.5893180784647));
#52140=CARTESIAN_POINT('Ctrl Pts',(-1.27264798379365,-1.,-3.59578698050164));
#52141=CARTESIAN_POINT('Ctrl Pts',(-1.27264798379365,1.,-3.59578698050164));
#52142=CARTESIAN_POINT('Ctrl Pts',(-1.27622049908664,-1.,-3.60199947736404));
#52143=CARTESIAN_POINT('Ctrl Pts',(-1.27622049908664,1.,-3.60199947736404));
#52144=CARTESIAN_POINT('Ctrl Pts',(-1.27983492861703,-1.,-3.60808907746372));
#52145=CARTESIAN_POINT('Ctrl Pts',(-1.27983492861703,1.,-3.60808907746372));
#52146=CARTESIAN_POINT('Ctrl Pts',(-1.28353255117754,-1.,-3.61418935913793));
#52147=CARTESIAN_POINT('Ctrl Pts',(-1.28353255117754,1.,-3.61418935913793));
#52148=CARTESIAN_POINT('Ctrl Pts',(-1.2873375502936,-1.,-3.62038148492295));
#52149=CARTESIAN_POINT('Ctrl Pts',(-1.2873375502936,1.,-3.62038148492295));
#52150=CARTESIAN_POINT('Ctrl Pts',(-1.29125046021853,-1.,-3.62667616004299));
#52151=CARTESIAN_POINT('Ctrl Pts',(-1.29125046021853,1.,-3.62667616004299));
#52152=CARTESIAN_POINT('Ctrl Pts',(-1.29525810207744,-1.,-3.63304271630995));
#52153=CARTESIAN_POINT('Ctrl Pts',(-1.29525810207744,1.,-3.63304271630995));
#52154=CARTESIAN_POINT('Ctrl Pts',(-1.29933955906463,-1.,-3.6394268987279));
#52155=CARTESIAN_POINT('Ctrl Pts',(-1.29933955906463,1.,-3.6394268987279));
#52156=CARTESIAN_POINT('Ctrl Pts',(-1.30347327603778,-1.,-3.64577181380125));
#52157=CARTESIAN_POINT('Ctrl Pts',(-1.30347327603778,1.,-3.64577181380125));
#52158=CARTESIAN_POINT('Ctrl Pts',(-1.30764479590051,-1.,-3.65204081987101));
#52159=CARTESIAN_POINT('Ctrl Pts',(-1.30764479590051,1.,-3.65204081987101));
#52160=CARTESIAN_POINT('Ctrl Pts',(-1.31185038411231,-1.,-3.65822827358655));
#52161=CARTESIAN_POINT('Ctrl Pts',(-1.31185038411231,1.,-3.65822827358655));
#52162=CARTESIAN_POINT('Ctrl Pts',(-1.31609271239922,-1.,-3.66434688899822));
#52163=CARTESIAN_POINT('Ctrl Pts',(-1.31609271239922,1.,-3.66434688899822));
#52164=CARTESIAN_POINT('Ctrl Pts',(-1.3203782813777,-1.,-3.67042021752668));
#52165=CARTESIAN_POINT('Ctrl Pts',(-1.3203782813777,1.,-3.67042021752668));
#52166=CARTESIAN_POINT('Ctrl Pts',(-1.32471430856413,-1.,-3.67647355257906));
#52167=CARTESIAN_POINT('Ctrl Pts',(-1.32471430856413,1.,-3.67647355257906));
#52168=CARTESIAN_POINT('Ctrl Pts',(-1.32910547072734,-1.,-3.68252441182534));
#52169=CARTESIAN_POINT('Ctrl Pts',(-1.32910547072734,1.,-3.68252441182534));
#52170=CARTESIAN_POINT('Ctrl Pts',(-1.33355191034515,-1.,-3.68857672413013));
#52171=CARTESIAN_POINT('Ctrl Pts',(-1.33355191034515,1.,-3.68857672413013));
#52172=CARTESIAN_POINT('Ctrl Pts',(-1.33805103398214,-1.,-3.69462613305692));
#52173=CARTESIAN_POINT('Ctrl Pts',(-1.33805103398214,1.,-3.69462613305692));
#52174=CARTESIAN_POINT('Ctrl Pts',(-1.3425986075293,-1.,-3.70066324015112));
#52175=CARTESIAN_POINT('Ctrl Pts',(-1.3425986075293,1.,-3.70066324015112));
#52176=CARTESIAN_POINT('Ctrl Pts',(-1.34719008463535,-1.,-3.7066775318825));
#52177=CARTESIAN_POINT('Ctrl Pts',(-1.34719008463535,1.,-3.7066775318825));
#52178=CARTESIAN_POINT('Ctrl Pts',(-1.35182193384426,-1.,-3.71266130563061));
#52179=CARTESIAN_POINT('Ctrl Pts',(-1.35182193384426,1.,-3.71266130563061));
#52180=CARTESIAN_POINT('Ctrl Pts',(-1.35649266705038,-1.,-3.71861271513318));
#52181=CARTESIAN_POINT('Ctrl Pts',(-1.35649266705038,1.,-3.71861271513318));
#52182=CARTESIAN_POINT('Ctrl Pts',(-1.36120211416353,-1.,-3.72453364678279));
#52183=CARTESIAN_POINT('Ctrl Pts',(-1.36120211416353,1.,-3.72453364678279));
#52184=CARTESIAN_POINT('Ctrl Pts',(-1.36595093298674,-1.,-3.73042829011293));
#52185=CARTESIAN_POINT('Ctrl Pts',(-1.36595093298674,1.,-3.73042829011293));
#52186=CARTESIAN_POINT('Ctrl Pts',(-1.37074003422739,-1.,-3.73630145885809));
#52187=CARTESIAN_POINT('Ctrl Pts',(-1.37074003422739,1.,-3.73630145885809));
#52188=CARTESIAN_POINT('Ctrl Pts',(-1.3755700297169,-1.,-3.7421569816256));
#52189=CARTESIAN_POINT('Ctrl Pts',(-1.3755700297169,1.,-3.7421569816256));
#52190=CARTESIAN_POINT('Ctrl Pts',(-1.38044070763302,-1.,-3.74799617204744));
#52191=CARTESIAN_POINT('Ctrl Pts',(-1.38044070763302,1.,-3.74799617204744));
#52192=CARTESIAN_POINT('Ctrl Pts',(-1.38535129801185,-1.,-3.75381861212728));
#52193=CARTESIAN_POINT('Ctrl Pts',(-1.38535129801185,1.,-3.75381861212728));
#52194=CARTESIAN_POINT('Ctrl Pts',(-1.39030069388926,-1.,-3.75962280650875));
#52195=CARTESIAN_POINT('Ctrl Pts',(-1.39030069388926,1.,-3.75962280650875));
#52196=CARTESIAN_POINT('Ctrl Pts',(-1.39528769118054,-1.,-3.76540689249078));
#52197=CARTESIAN_POINT('Ctrl Pts',(-1.39528769118054,1.,-3.76540689249078));
#52198=CARTESIAN_POINT('Ctrl Pts',(-1.40031121335495,-1.,-3.77116930621804));
#52199=CARTESIAN_POINT('Ctrl Pts',(-1.40031121335495,1.,-3.77116930621804));
#52200=CARTESIAN_POINT('Ctrl Pts',(-1.40537056004702,-1.,-3.77690952014209));
#52201=CARTESIAN_POINT('Ctrl Pts',(-1.40537056004702,1.,-3.77690952014209));
#52202=CARTESIAN_POINT('Ctrl Pts',(-1.41046532282567,-1.,-3.78262780065406));
#52203=CARTESIAN_POINT('Ctrl Pts',(-1.41046532282567,1.,-3.78262780065406));
#52204=CARTESIAN_POINT('Ctrl Pts',(-1.41559527803808,-1.,-3.78832489879369));
#52205=CARTESIAN_POINT('Ctrl Pts',(-1.41559527803808,1.,-3.78832489879369));
#52206=CARTESIAN_POINT('Ctrl Pts',(-1.42076028482828,-1.,-3.7940017574439));
#52207=CARTESIAN_POINT('Ctrl Pts',(-1.42076028482828,1.,-3.7940017574439));
#52208=CARTESIAN_POINT('Ctrl Pts',(-1.42596018777301,-1.,-3.79965923196365));
#52209=CARTESIAN_POINT('Ctrl Pts',(-1.42596018777301,1.,-3.79965923196365));
#52210=CARTESIAN_POINT('Ctrl Pts',(-1.43119469921364,-1.,-3.80529775429916));
#52211=CARTESIAN_POINT('Ctrl Pts',(-1.43119469921364,1.,-3.80529775429916));
#52212=CARTESIAN_POINT('Ctrl Pts',(-1.43646341556783,-1.,-3.81091737726965));
#52213=CARTESIAN_POINT('Ctrl Pts',(-1.43646341556783,1.,-3.81091737726965));
#52214=CARTESIAN_POINT('Ctrl Pts',(-1.44176587041401,-1.,-3.8165179239855));
#52215=CARTESIAN_POINT('Ctrl Pts',(-1.44176587041401,1.,-3.8165179239855));
#52216=CARTESIAN_POINT('Ctrl Pts',(-1.44710157648562,-1.,-3.82209910620591));
#52217=CARTESIAN_POINT('Ctrl Pts',(-1.44710157648562,1.,-3.82209910620591));
#52218=CARTESIAN_POINT('Ctrl Pts',(-1.45247006796807,-1.,-3.82766064519));
#52219=CARTESIAN_POINT('Ctrl Pts',(-1.45247006796807,1.,-3.82766064519));
#52220=CARTESIAN_POINT('Ctrl Pts',(-1.45787095220763,-1.,-3.83320241775199));
#52221=CARTESIAN_POINT('Ctrl Pts',(-1.45787095220763,1.,-3.83320241775199));
#52222=CARTESIAN_POINT('Ctrl Pts',(-1.46330391180621,-1.,-3.83872447159309));
#52223=CARTESIAN_POINT('Ctrl Pts',(-1.46330391180621,1.,-3.83872447159309));
#52224=CARTESIAN_POINT('Ctrl Pts',(-1.46876867426375,-1.,-3.84422695454469));
#52225=CARTESIAN_POINT('Ctrl Pts',(-1.46876867426375,1.,-3.84422695454469));
#52226=CARTESIAN_POINT('Ctrl Pts',(-1.47426499018467,-1.,-3.84971006847096));
#52227=CARTESIAN_POINT('Ctrl Pts',(-1.47426499018467,1.,-3.84971006847096));
#52228=CARTESIAN_POINT('Ctrl Pts',(-1.47979260991063,-1.,-3.85517401698952));
#52229=CARTESIAN_POINT('Ctrl Pts',(-1.47979260991063,1.,-3.85517401698952));
#52230=CARTESIAN_POINT('Ctrl Pts',(-1.48535125510102,-1.,-3.86061894706551));
#52231=CARTESIAN_POINT('Ctrl Pts',(-1.48535125510102,1.,-3.86061894706551));
#52232=CARTESIAN_POINT('Ctrl Pts',(-1.49094061164604,-1.,-3.86604492575933));
#52233=CARTESIAN_POINT('Ctrl Pts',(-1.49094061164604,1.,-3.86604492575933));
#52234=CARTESIAN_POINT('Ctrl Pts',(-1.4965603539944,-1.,-3.8714519699927));
#52235=CARTESIAN_POINT('Ctrl Pts',(-1.4965603539944,1.,-3.8714519699927));
#52236=CARTESIAN_POINT('Ctrl Pts',(-1.50221016176766,-1.,-3.87684006372665));
#52237=CARTESIAN_POINT('Ctrl Pts',(-1.50221016176766,1.,-3.87684006372665));
#52238=CARTESIAN_POINT('Ctrl Pts',(-1.50788973857719,-1.,-3.88220917950443));
#52239=CARTESIAN_POINT('Ctrl Pts',(-1.50788973857719,1.,-3.88220917950443));
#52240=CARTESIAN_POINT('Ctrl Pts',(-1.51359883110181,-1.,-3.88755930032927));
#52241=CARTESIAN_POINT('Ctrl Pts',(-1.51359883110181,1.,-3.88755930032927));
#52242=CARTESIAN_POINT('Ctrl Pts',(-1.51933724328609,-1.,-3.89289043531893));
#52243=CARTESIAN_POINT('Ctrl Pts',(-1.51933724328609,1.,-3.89289043531893));
#52244=CARTESIAN_POINT('Ctrl Pts',(-1.52510482990784,-1.,-3.8982026070607));
#52245=CARTESIAN_POINT('Ctrl Pts',(-1.52510482990784,1.,-3.8982026070607));
#52246=CARTESIAN_POINT('Ctrl Pts',(-1.5297421605556,-1.,-3.90243719629755));
#52247=CARTESIAN_POINT('Ctrl Pts',(-1.5297421605556,1.,-3.90243719629755));
#52248=CARTESIAN_POINT('Ctrl Pts',(-1.53323321827311,-1.,-3.90560462812846));
#52249=CARTESIAN_POINT('Ctrl Pts',(-1.53323321827311,1.,-3.90560462812846));
#52250=CARTESIAN_POINT('Ctrl Pts',(-1.53556639217742,-1.,-3.90771246854607));
#52251=CARTESIAN_POINT('Ctrl Pts',(-1.53556639217742,1.,-3.90771246854607));
#52252=CARTESIAN_POINT('Ctrl Pts',(-1.53673442965255,-1.,-3.90876544355381));
#52253=CARTESIAN_POINT('Ctrl Pts',(-1.53673442965255,1.,-3.90876544355381));
#52254=CARTESIAN_POINT('',(-1.24526366418208,1.,-3.5372048861591));
#52255=CARTESIAN_POINT('Ctrl Pts',(-1.24526366418208,-1.,-3.5372048861591));
#52256=CARTESIAN_POINT('Ctrl Pts',(-1.24526366418208,-0.666666666666667,
-3.5372048861591));
#52257=CARTESIAN_POINT('Ctrl Pts',(-1.24526366418208,-0.333333333333333,
-3.5372048861591));
#52258=CARTESIAN_POINT('Ctrl Pts',(-1.24526366418208,0.333333333333333,
-3.5372048861591));
#52259=CARTESIAN_POINT('Ctrl Pts',(-1.24526366418208,0.666666666666667,
-3.5372048861591));
#52260=CARTESIAN_POINT('Ctrl Pts',(-1.24526366418208,1.,-3.5372048861591));
#52261=CARTESIAN_POINT('',(-1.53673442965255,1.,-3.90876544355381));
#52262=CARTESIAN_POINT('',(-1.53673442965255,0.,-3.90876544355381));
#52263=CARTESIAN_POINT('Ctrl Pts',(-1.24526366418208,1.,-3.5372048861591));
#52264=CARTESIAN_POINT('Ctrl Pts',(-1.24524838931864,1.,-3.53725139174402));
#52265=CARTESIAN_POINT('Ctrl Pts',(-1.24524498991133,1.,-3.53744859265385));
#52266=CARTESIAN_POINT('Ctrl Pts',(-1.2453920538873,1.,-3.53808746578052));
#52267=CARTESIAN_POINT('Ctrl Pts',(-1.24593497225964,1.,-3.53968291129942));
#52268=CARTESIAN_POINT('Ctrl Pts',(-1.2472164623202,1.,-3.54294877426113));
#52269=CARTESIAN_POINT('Ctrl Pts',(-1.24926408627938,1.,-3.54784190282889));
#52270=CARTESIAN_POINT('Ctrl Pts',(-1.25188792940508,1.,-3.5538728741862));
#52271=CARTESIAN_POINT('Ctrl Pts',(-1.25496090899873,1.,-3.56071094990825));
#52272=CARTESIAN_POINT('Ctrl Pts',(-1.25834000485626,1.,-3.56798645995025));
#52273=CARTESIAN_POINT('Ctrl Pts',(-1.26188667142784,1.,-3.5753456065164));
#52274=CARTESIAN_POINT('Ctrl Pts',(-1.26548706249891,1.,-3.58250452868699));
#52275=CARTESIAN_POINT('Ctrl Pts',(-1.26907758484766,1.,-3.5893180784647));
#52276=CARTESIAN_POINT('Ctrl Pts',(-1.27264798379365,1.,-3.59578698050164));
#52277=CARTESIAN_POINT('Ctrl Pts',(-1.27622049908664,1.,-3.60199947736404));
#52278=CARTESIAN_POINT('Ctrl Pts',(-1.27983492861703,1.,-3.60808907746372));
#52279=CARTESIAN_POINT('Ctrl Pts',(-1.28353255117754,1.,-3.61418935913793));
#52280=CARTESIAN_POINT('Ctrl Pts',(-1.2873375502936,1.,-3.62038148492295));
#52281=CARTESIAN_POINT('Ctrl Pts',(-1.29125046021853,1.,-3.62667616004299));
#52282=CARTESIAN_POINT('Ctrl Pts',(-1.29525810207744,1.,-3.63304271630995));
#52283=CARTESIAN_POINT('Ctrl Pts',(-1.29933955906463,1.,-3.6394268987279));
#52284=CARTESIAN_POINT('Ctrl Pts',(-1.30347327603778,1.,-3.64577181380125));
#52285=CARTESIAN_POINT('Ctrl Pts',(-1.30764479590051,1.,-3.65204081987101));
#52286=CARTESIAN_POINT('Ctrl Pts',(-1.31185038411231,1.,-3.65822827358655));
#52287=CARTESIAN_POINT('Ctrl Pts',(-1.31609271239922,1.,-3.66434688899822));
#52288=CARTESIAN_POINT('Ctrl Pts',(-1.3203782813777,1.,-3.67042021752668));
#52289=CARTESIAN_POINT('Ctrl Pts',(-1.32471430856413,1.,-3.67647355257906));
#52290=CARTESIAN_POINT('Ctrl Pts',(-1.32910547072734,1.,-3.68252441182534));
#52291=CARTESIAN_POINT('Ctrl Pts',(-1.33355191034515,1.,-3.68857672413013));
#52292=CARTESIAN_POINT('Ctrl Pts',(-1.33805103398214,1.,-3.69462613305692));
#52293=CARTESIAN_POINT('Ctrl Pts',(-1.3425986075293,1.,-3.70066324015112));
#52294=CARTESIAN_POINT('Ctrl Pts',(-1.34719008463535,1.,-3.7066775318825));
#52295=CARTESIAN_POINT('Ctrl Pts',(-1.35182193384426,1.,-3.71266130563061));
#52296=CARTESIAN_POINT('Ctrl Pts',(-1.35649266705038,1.,-3.71861271513318));
#52297=CARTESIAN_POINT('Ctrl Pts',(-1.36120211416353,1.,-3.72453364678279));
#52298=CARTESIAN_POINT('Ctrl Pts',(-1.36595093298674,1.,-3.73042829011293));
#52299=CARTESIAN_POINT('Ctrl Pts',(-1.37074003422739,1.,-3.73630145885809));
#52300=CARTESIAN_POINT('Ctrl Pts',(-1.3755700297169,1.,-3.7421569816256));
#52301=CARTESIAN_POINT('Ctrl Pts',(-1.38044070763302,1.,-3.74799617204744));
#52302=CARTESIAN_POINT('Ctrl Pts',(-1.38535129801185,1.,-3.75381861212728));
#52303=CARTESIAN_POINT('Ctrl Pts',(-1.39030069388926,1.,-3.75962280650875));
#52304=CARTESIAN_POINT('Ctrl Pts',(-1.39528769118054,1.,-3.76540689249078));
#52305=CARTESIAN_POINT('Ctrl Pts',(-1.40031121335495,1.,-3.77116930621804));
#52306=CARTESIAN_POINT('Ctrl Pts',(-1.40537056004702,1.,-3.77690952014209));
#52307=CARTESIAN_POINT('Ctrl Pts',(-1.41046532282567,1.,-3.78262780065406));
#52308=CARTESIAN_POINT('Ctrl Pts',(-1.41559527803808,1.,-3.78832489879369));
#52309=CARTESIAN_POINT('Ctrl Pts',(-1.42076028482828,1.,-3.7940017574439));
#52310=CARTESIAN_POINT('Ctrl Pts',(-1.42596018777301,1.,-3.79965923196365));
#52311=CARTESIAN_POINT('Ctrl Pts',(-1.43119469921364,1.,-3.80529775429916));
#52312=CARTESIAN_POINT('Ctrl Pts',(-1.43646341556783,1.,-3.81091737726965));
#52313=CARTESIAN_POINT('Ctrl Pts',(-1.44176587041401,1.,-3.8165179239855));
#52314=CARTESIAN_POINT('Ctrl Pts',(-1.44710157648562,1.,-3.82209910620591));
#52315=CARTESIAN_POINT('Ctrl Pts',(-1.45247006796807,1.,-3.82766064519));
#52316=CARTESIAN_POINT('Ctrl Pts',(-1.45787095220763,1.,-3.83320241775199));
#52317=CARTESIAN_POINT('Ctrl Pts',(-1.46330391180621,1.,-3.83872447159309));
#52318=CARTESIAN_POINT('Ctrl Pts',(-1.46876867426375,1.,-3.84422695454469));
#52319=CARTESIAN_POINT('Ctrl Pts',(-1.47426499018467,1.,-3.84971006847096));
#52320=CARTESIAN_POINT('Ctrl Pts',(-1.47979260991063,1.,-3.85517401698952));
#52321=CARTESIAN_POINT('Ctrl Pts',(-1.48535125510102,1.,-3.86061894706551));
#52322=CARTESIAN_POINT('Ctrl Pts',(-1.49094061164604,1.,-3.86604492575933));
#52323=CARTESIAN_POINT('Ctrl Pts',(-1.4965603539944,1.,-3.8714519699927));
#52324=CARTESIAN_POINT('Ctrl Pts',(-1.50221016176766,1.,-3.87684006372665));
#52325=CARTESIAN_POINT('Ctrl Pts',(-1.50788973857719,1.,-3.88220917950443));
#52326=CARTESIAN_POINT('Ctrl Pts',(-1.51359883110181,1.,-3.88755930032927));
#52327=CARTESIAN_POINT('Ctrl Pts',(-1.51933724328609,1.,-3.89289043531893));
#52328=CARTESIAN_POINT('Ctrl Pts',(-1.52510482990784,1.,-3.8982026070607));
#52329=CARTESIAN_POINT('Ctrl Pts',(-1.5297421605556,1.,-3.90243719629755));
#52330=CARTESIAN_POINT('Ctrl Pts',(-1.53323321827311,1.,-3.90560462812846));
#52331=CARTESIAN_POINT('Ctrl Pts',(-1.53556639217742,1.,-3.90771246854607));
#52332=CARTESIAN_POINT('Ctrl Pts',(-1.53673442965255,1.,-3.90876544355381));
#52333=CARTESIAN_POINT('Origin',(-1.53673442965255,0.,-3.90876544355381));
#52334=CARTESIAN_POINT('',(-1.67727921511438,1.,-3.85054988729471));
#52335=CARTESIAN_POINT('Origin',(0.,0.,0.));
#52336=CARTESIAN_POINT('',(-1.071677399622,1.,-3.59360648251021));
#52337=CARTESIAN_POINT('Origin',(0.,1.,0.));
#52338=CARTESIAN_POINT('Ctrl Pts',(-1.071677399622,1.,-3.59360648251021));
#52339=CARTESIAN_POINT('Ctrl Pts',(-1.071677399622,0.666666666666667,-3.59360648251021));
#52340=CARTESIAN_POINT('Ctrl Pts',(-1.071677399622,0.333333333333333,-3.59360648251021));
#52341=CARTESIAN_POINT('Ctrl Pts',(-1.071677399622,-0.333333333333333,-3.59360648251021));
#52342=CARTESIAN_POINT('Ctrl Pts',(-1.071677399622,-0.666666666666667,-3.59360648251021));
#52343=CARTESIAN_POINT('Ctrl Pts',(-1.071677399622,-1.,-3.59360648251021));
#52344=CARTESIAN_POINT('Ctrl Pts',(-1.05427041296137,-1.,-4.06552750530042));
#52345=CARTESIAN_POINT('Ctrl Pts',(-1.05427041296137,1.,-4.06552750530042));
#52346=CARTESIAN_POINT('Ctrl Pts',(-1.05459645194934,-1.,-4.06398907542679));
#52347=CARTESIAN_POINT('Ctrl Pts',(-1.05459645194934,1.,-4.06398907542679));
#52348=CARTESIAN_POINT('Ctrl Pts',(-1.05524507177901,-1.,-4.06091239150293));
#52349=CARTESIAN_POINT('Ctrl Pts',(-1.05524507177901,1.,-4.06091239150293));
#52350=CARTESIAN_POINT('Ctrl Pts',(-1.0562076270849,-1.,-4.05629789308941));
#52351=CARTESIAN_POINT('Ctrl Pts',(-1.0562076270849,1.,-4.05629789308941));
#52352=CARTESIAN_POINT('Ctrl Pts',(-1.05747027728537,-1.,-4.05014628387112));
#52353=CARTESIAN_POINT('Ctrl Pts',(-1.05747027728537,1.,-4.05014628387112));
#52354=CARTESIAN_POINT('Ctrl Pts',(-1.05901393667039,-1.,-4.04245854429333));
#52355=CARTESIAN_POINT('Ctrl Pts',(-1.05901393667039,1.,-4.04245854429333));
#52356=CARTESIAN_POINT('Ctrl Pts',(-1.06052284712114,-1.,-4.03477261142549));
#52357=CARTESIAN_POINT('Ctrl Pts',(-1.06052284712114,1.,-4.03477261142549));
#52358=CARTESIAN_POINT('Ctrl Pts',(-1.06199687787488,-1.,-4.02708855235732));
#52359=CARTESIAN_POINT('Ctrl Pts',(-1.06199687787488,1.,-4.02708855235732));
#52360=CARTESIAN_POINT('Ctrl Pts',(-1.06343586496094,-1.,-4.0194064749539));
#52361=CARTESIAN_POINT('Ctrl Pts',(-1.06343586496094,1.,-4.0194064749539));
#52362=CARTESIAN_POINT('Ctrl Pts',(-1.06483961342894,-1.,-4.0117265418656));
#52363=CARTESIAN_POINT('Ctrl Pts',(-1.06483961342894,1.,-4.0117265418656));
#52364=CARTESIAN_POINT('Ctrl Pts',(-1.06620789963406,-1.,-4.00404894951804));
#52365=CARTESIAN_POINT('Ctrl Pts',(-1.06620789963406,1.,-4.00404894951804));
#52366=CARTESIAN_POINT('Ctrl Pts',(-1.06754047381188,-1.,-3.99637389919958));
#52367=CARTESIAN_POINT('Ctrl Pts',(-1.06754047381188,1.,-3.99637389919958));
#52368=CARTESIAN_POINT('Ctrl Pts',(-1.06883706263912,-1.,-3.98870156857298));
#52369=CARTESIAN_POINT('Ctrl Pts',(-1.06883706263912,1.,-3.98870156857298));
#52370=CARTESIAN_POINT('Ctrl Pts',(-1.07009737257815,-1.,-3.98103208801289));
#52371=CARTESIAN_POINT('Ctrl Pts',(-1.07009737257815,1.,-3.98103208801289));
#52372=CARTESIAN_POINT('Ctrl Pts',(-1.07132109206252,-1.,-3.97336550222571));
#52373=CARTESIAN_POINT('Ctrl Pts',(-1.07132109206252,1.,-3.97336550222571));
#52374=CARTESIAN_POINT('Ctrl Pts',(-1.07250789943095,-1.,-3.96570179322681));
#52375=CARTESIAN_POINT('Ctrl Pts',(-1.07250789943095,1.,-3.96570179322681));
#52376=CARTESIAN_POINT('Ctrl Pts',(-1.07365747426551,-1.,-3.95804094429606));
#52377=CARTESIAN_POINT('Ctrl Pts',(-1.07365747426551,1.,-3.95804094429606));
#52378=CARTESIAN_POINT('Ctrl Pts',(-1.07476950921607,-1.,-3.95038299600754));
#52379=CARTESIAN_POINT('Ctrl Pts',(-1.07476950921607,1.,-3.95038299600754));
#52380=CARTESIAN_POINT('Ctrl Pts',(-1.07584371946428,-1.,-3.94272809633271));
#52381=CARTESIAN_POINT('Ctrl Pts',(-1.07584371946428,1.,-3.94272809633271));
#52382=CARTESIAN_POINT('Ctrl Pts',(-1.07687985975348,-1.,-3.93507657572743));
#52383=CARTESIAN_POINT('Ctrl Pts',(-1.07687985975348,1.,-3.93507657572743));
#52384=CARTESIAN_POINT('Ctrl Pts',(-1.07787771707155,-1.,-3.92742893349684));
#52385=CARTESIAN_POINT('Ctrl Pts',(-1.07787771707155,1.,-3.92742893349684));
#52386=CARTESIAN_POINT('Ctrl Pts',(-1.07883706663524,-1.,-3.91978568924062));
#52387=CARTESIAN_POINT('Ctrl Pts',(-1.07883706663524,1.,-3.91978568924062));
#52388=CARTESIAN_POINT('Ctrl Pts',(-1.0797576350746,-1.,-3.91214726022096));
#52389=CARTESIAN_POINT('Ctrl Pts',(-1.0797576350746,1.,-3.91214726022096));
#52390=CARTESIAN_POINT('Ctrl Pts',(-1.08063906483822,-1.,-3.90451384092564));
#52391=CARTESIAN_POINT('Ctrl Pts',(-1.08063906483822,1.,-3.90451384092564));
#52392=CARTESIAN_POINT('Ctrl Pts',(-1.08148086931373,-1.,-3.89688525098408));
#52393=CARTESIAN_POINT('Ctrl Pts',(-1.08148086931373,1.,-3.89688525098408));
#52394=CARTESIAN_POINT('Ctrl Pts',(-1.08228241999363,-1.,-3.88926088975182));
#52395=CARTESIAN_POINT('Ctrl Pts',(-1.08228241999363,1.,-3.88926088975182));
#52396=CARTESIAN_POINT('Ctrl Pts',(-1.08304304871042,-1.,-3.88164007721365));
#52397=CARTESIAN_POINT('Ctrl Pts',(-1.08304304871042,1.,-3.88164007721365));
#52398=CARTESIAN_POINT('Ctrl Pts',(-1.0837621330751,-1.,-3.87402233722563));
#52399=CARTESIAN_POINT('Ctrl Pts',(-1.0837621330751,1.,-3.87402233722563));
#52400=CARTESIAN_POINT('Ctrl Pts',(-1.08443918607926,-1.,-3.86640769434269));
#52401=CARTESIAN_POINT('Ctrl Pts',(-1.08443918607926,1.,-3.86640769434269));
#52402=CARTESIAN_POINT('Ctrl Pts',(-1.08507395120054,-1.,-3.85879698702511));
#52403=CARTESIAN_POINT('Ctrl Pts',(-1.08507395120054,1.,-3.85879698702511));
#52404=CARTESIAN_POINT('Ctrl Pts',(-1.08566647671838,-1.,-3.85119211322732));
#52405=CARTESIAN_POINT('Ctrl Pts',(-1.08566647671838,1.,-3.85119211322732));
#52406=CARTESIAN_POINT('Ctrl Pts',(-1.08621688337601,-1.,-3.84359528764934));
#52407=CARTESIAN_POINT('Ctrl Pts',(-1.08621688337601,1.,-3.84359528764934));
#52408=CARTESIAN_POINT('Ctrl Pts',(-1.08672515456901,-1.,-3.83600837071702));
#52409=CARTESIAN_POINT('Ctrl Pts',(-1.08672515456901,1.,-3.83600837071702));
#52410=CARTESIAN_POINT('Ctrl Pts',(-1.08719091307558,-1.,-3.82843215316985));
#52411=CARTESIAN_POINT('Ctrl Pts',(-1.08719091307558,1.,-3.82843215316985));
#52412=CARTESIAN_POINT('Ctrl Pts',(-1.08761321539442,-1.,-3.82086569676321));
#52413=CARTESIAN_POINT('Ctrl Pts',(-1.08761321539442,1.,-3.82086569676321));
#52414=CARTESIAN_POINT('Ctrl Pts',(-1.08799030610861,-1.,-3.81330554446324));
#52415=CARTESIAN_POINT('Ctrl Pts',(-1.08799030610861,1.,-3.81330554446324));
#52416=CARTESIAN_POINT('Ctrl Pts',(-1.08832009255378,-1.,-3.80574726657656));
#52417=CARTESIAN_POINT('Ctrl Pts',(-1.08832009255378,1.,-3.80574726657656));
#52418=CARTESIAN_POINT('Ctrl Pts',(-1.08860064435776,-1.,-3.79818708705252));
#52419=CARTESIAN_POINT('Ctrl Pts',(-1.08860064435776,1.,-3.79818708705252));
#52420=CARTESIAN_POINT('Ctrl Pts',(-1.08883071512097,-1.,-3.79062357974401));
#52421=CARTESIAN_POINT('Ctrl Pts',(-1.08883071512097,1.,-3.79062357974401));
#52422=CARTESIAN_POINT('Ctrl Pts',(-1.08901018614638,-1.,-3.78305911299511));
#52423=CARTESIAN_POINT('Ctrl Pts',(-1.08901018614638,1.,-3.78305911299511));
#52424=CARTESIAN_POINT('Ctrl Pts',(-1.08914072791275,-1.,-3.7755019940944));
#52425=CARTESIAN_POINT('Ctrl Pts',(-1.08914072791275,1.,-3.7755019940944));
#52426=CARTESIAN_POINT('Ctrl Pts',(-1.08922484204263,-1.,-3.76796340094469));
#52427=CARTESIAN_POINT('Ctrl Pts',(-1.08922484204263,1.,-3.76796340094469));
#52428=CARTESIAN_POINT('Ctrl Pts',(-1.08926462734287,-1.,-3.76045342580226));
#52429=CARTESIAN_POINT('Ctrl Pts',(-1.08926462734287,1.,-3.76045342580226));
#52430=CARTESIAN_POINT('Ctrl Pts',(-1.08926054632927,-1.,-3.75297711748138));
#52431=CARTESIAN_POINT('Ctrl Pts',(-1.08926054632927,1.,-3.75297711748138));
#52432=CARTESIAN_POINT('Ctrl Pts',(-1.08921040494013,-1.,-3.74553121371745));
#52433=CARTESIAN_POINT('Ctrl Pts',(-1.08921040494013,1.,-3.74553121371745));
#52434=CARTESIAN_POINT('Ctrl Pts',(-1.08910769013288,-1.,-3.73809879348209));
#52435=CARTESIAN_POINT('Ctrl Pts',(-1.08910769013288,1.,-3.73809879348209));
#52436=CARTESIAN_POINT('Ctrl Pts',(-1.08894337390925,-1.,-3.73065515162949));
#52437=CARTESIAN_POINT('Ctrl Pts',(-1.08894337390925,1.,-3.73065515162949));
#52438=CARTESIAN_POINT('Ctrl Pts',(-1.08870887220072,-1.,-3.72317741369364));
#52439=CARTESIAN_POINT('Ctrl Pts',(-1.08870887220072,1.,-3.72317741369364));
#52440=CARTESIAN_POINT('Ctrl Pts',(-1.08839887334777,-1.,-3.71565372339063));
#52441=CARTESIAN_POINT('Ctrl Pts',(-1.08839887334777,1.,-3.71565372339063));
#52442=CARTESIAN_POINT('Ctrl Pts',(-1.0880136731219,-1.,-3.70809084139476));
#52443=CARTESIAN_POINT('Ctrl Pts',(-1.0880136731219,1.,-3.70809084139476));
#52444=CARTESIAN_POINT('Ctrl Pts',(-1.08756311291324,-1.,-3.70052690909884));
#52445=CARTESIAN_POINT('Ctrl Pts',(-1.08756311291324,1.,-3.70052690909884));
#52446=CARTESIAN_POINT('Ctrl Pts',(-1.08706319540292,-1.,-3.69302062410229));
#52447=CARTESIAN_POINT('Ctrl Pts',(-1.08706319540292,1.,-3.69302062410229));
#52448=CARTESIAN_POINT('Ctrl Pts',(-1.08652888882609,-1.,-3.68562817420864));
#52449=CARTESIAN_POINT('Ctrl Pts',(-1.08652888882609,1.,-3.68562817420864));
#52450=CARTESIAN_POINT('Ctrl Pts',(-1.08596755755768,-1.,-3.67838211685148));
#52451=CARTESIAN_POINT('Ctrl Pts',(-1.08596755755768,1.,-3.67838211685148));
#52452=CARTESIAN_POINT('Ctrl Pts',(-1.0853733414448,-1.,-3.67127347729632));
#52453=CARTESIAN_POINT('Ctrl Pts',(-1.0853733414448,1.,-3.67127347729632));
#52454=CARTESIAN_POINT('Ctrl Pts',(-1.0847180992287,-1.,-3.66422237895256));
#52455=CARTESIAN_POINT('Ctrl Pts',(-1.0847180992287,1.,-3.66422237895256));
#52456=CARTESIAN_POINT('Ctrl Pts',(-1.08395671077761,-1.,-3.65709649161004));
#52457=CARTESIAN_POINT('Ctrl Pts',(-1.08395671077761,1.,-3.65709649161004));
#52458=CARTESIAN_POINT('Ctrl Pts',(-1.08304289898577,-1.,-3.64976441208197));
#52459=CARTESIAN_POINT('Ctrl Pts',(-1.08304289898577,1.,-3.64976441208197));
#52460=CARTESIAN_POINT('Ctrl Pts',(-1.08194278850972,-1.,-3.64214167843595));
#52461=CARTESIAN_POINT('Ctrl Pts',(-1.08194278850972,1.,-3.64214167843595));
#52462=CARTESIAN_POINT('Ctrl Pts',(-1.08064765719887,-1.,-3.63423373196602));
#52463=CARTESIAN_POINT('Ctrl Pts',(-1.08064765719887,1.,-3.63423373196602));
#52464=CARTESIAN_POINT('Ctrl Pts',(-1.07919137290815,-1.,-3.62619537902616));
#52465=CARTESIAN_POINT('Ctrl Pts',(-1.07919137290815,1.,-3.62619537902616));
#52466=CARTESIAN_POINT('Ctrl Pts',(-1.07764868137729,-1.,-3.61832318504957));
#52467=CARTESIAN_POINT('Ctrl Pts',(-1.07764868137729,1.,-3.61832318504957));
#52468=CARTESIAN_POINT('Ctrl Pts',(-1.07611545402841,-1.,-3.61098481349577));
#52469=CARTESIAN_POINT('Ctrl Pts',(-1.07611545402841,1.,-3.61098481349577));
#52470=CARTESIAN_POINT('Ctrl Pts',(-1.0746932716863,-1.,-3.6045633988796));
#52471=CARTESIAN_POINT('Ctrl Pts',(-1.0746932716863,1.,-3.6045633988796));
#52472=CARTESIAN_POINT('Ctrl Pts',(-1.0734737254567,-1.,-3.59940121154383));
#52473=CARTESIAN_POINT('Ctrl Pts',(-1.0734737254567,1.,-3.59940121154383));
#52474=CARTESIAN_POINT('Ctrl Pts',(-1.07251922679108,-1.,-3.59573039611837));
#52475=CARTESIAN_POINT('Ctrl Pts',(-1.07251922679108,1.,-3.59573039611837));
#52476=CARTESIAN_POINT('Ctrl Pts',(-1.07199116987503,-1.,-3.59407399103556));
#52477=CARTESIAN_POINT('Ctrl Pts',(-1.07199116987503,1.,-3.59407399103556));
#52478=CARTESIAN_POINT('Ctrl Pts',(-1.07173216219041,-1.,-3.59356848057451));
#52479=CARTESIAN_POINT('Ctrl Pts',(-1.07173216219041,1.,-3.59356848057451));
#52480=CARTESIAN_POINT('Ctrl Pts',(-1.07162034256419,-1.,-3.59355870577763));
#52481=CARTESIAN_POINT('Ctrl Pts',(-1.07162034256419,1.,-3.59355870577763));
#52482=CARTESIAN_POINT('Ctrl Pts',(-1.07157964745328,-1.,-3.59363563249864));
#52483=CARTESIAN_POINT('Ctrl Pts',(-1.07157964745328,1.,-3.59363563249864));
#52484=CARTESIAN_POINT('',(-1.05427041296137,1.,-4.06552750530042));
#52485=CARTESIAN_POINT('Ctrl Pts',(-1.05427041296137,1.,-4.06552750530042));
#52486=CARTESIAN_POINT('Ctrl Pts',(-1.05459645194934,1.,-4.06398907542679));
#52487=CARTESIAN_POINT('Ctrl Pts',(-1.05524507177901,1.,-4.06091239150293));
#52488=CARTESIAN_POINT('Ctrl Pts',(-1.0562076270849,1.,-4.05629789308941));
#52489=CARTESIAN_POINT('Ctrl Pts',(-1.05747027728537,1.,-4.05014628387112));
#52490=CARTESIAN_POINT('Ctrl Pts',(-1.05901393667039,1.,-4.04245854429333));
#52491=CARTESIAN_POINT('Ctrl Pts',(-1.06052284712114,1.,-4.03477261142549));
#52492=CARTESIAN_POINT('Ctrl Pts',(-1.06199687787488,1.,-4.02708855235732));
#52493=CARTESIAN_POINT('Ctrl Pts',(-1.06343586496094,1.,-4.0194064749539));
#52494=CARTESIAN_POINT('Ctrl Pts',(-1.06483961342894,1.,-4.0117265418656));
#52495=CARTESIAN_POINT('Ctrl Pts',(-1.06620789963406,1.,-4.00404894951804));
#52496=CARTESIAN_POINT('Ctrl Pts',(-1.06754047381188,1.,-3.99637389919958));
#52497=CARTESIAN_POINT('Ctrl Pts',(-1.06883706263912,1.,-3.98870156857298));
#52498=CARTESIAN_POINT('Ctrl Pts',(-1.07009737257815,1.,-3.98103208801289));
#52499=CARTESIAN_POINT('Ctrl Pts',(-1.07132109206252,1.,-3.97336550222571));
#52500=CARTESIAN_POINT('Ctrl Pts',(-1.07250789943095,1.,-3.96570179322681));
#52501=CARTESIAN_POINT('Ctrl Pts',(-1.07365747426551,1.,-3.95804094429606));
#52502=CARTESIAN_POINT('Ctrl Pts',(-1.07476950921607,1.,-3.95038299600754));
#52503=CARTESIAN_POINT('Ctrl Pts',(-1.07584371946428,1.,-3.94272809633271));
#52504=CARTESIAN_POINT('Ctrl Pts',(-1.07687985975348,1.,-3.93507657572743));
#52505=CARTESIAN_POINT('Ctrl Pts',(-1.07787771707155,1.,-3.92742893349684));
#52506=CARTESIAN_POINT('Ctrl Pts',(-1.07883706663524,1.,-3.91978568924062));
#52507=CARTESIAN_POINT('Ctrl Pts',(-1.0797576350746,1.,-3.91214726022096));
#52508=CARTESIAN_POINT('Ctrl Pts',(-1.08063906483822,1.,-3.90451384092564));
#52509=CARTESIAN_POINT('Ctrl Pts',(-1.08148086931373,1.,-3.89688525098408));
#52510=CARTESIAN_POINT('Ctrl Pts',(-1.08228241999363,1.,-3.88926088975182));
#52511=CARTESIAN_POINT('Ctrl Pts',(-1.08304304871042,1.,-3.88164007721365));
#52512=CARTESIAN_POINT('Ctrl Pts',(-1.0837621330751,1.,-3.87402233722563));
#52513=CARTESIAN_POINT('Ctrl Pts',(-1.08443918607926,1.,-3.86640769434269));
#52514=CARTESIAN_POINT('Ctrl Pts',(-1.08507395120054,1.,-3.85879698702511));
#52515=CARTESIAN_POINT('Ctrl Pts',(-1.08566647671838,1.,-3.85119211322732));
#52516=CARTESIAN_POINT('Ctrl Pts',(-1.08621688337601,1.,-3.84359528764934));
#52517=CARTESIAN_POINT('Ctrl Pts',(-1.08672515456901,1.,-3.83600837071702));
#52518=CARTESIAN_POINT('Ctrl Pts',(-1.08719091307558,1.,-3.82843215316985));
#52519=CARTESIAN_POINT('Ctrl Pts',(-1.08761321539442,1.,-3.82086569676321));
#52520=CARTESIAN_POINT('Ctrl Pts',(-1.08799030610861,1.,-3.81330554446324));
#52521=CARTESIAN_POINT('Ctrl Pts',(-1.08832009255378,1.,-3.80574726657656));
#52522=CARTESIAN_POINT('Ctrl Pts',(-1.08860064435776,1.,-3.79818708705252));
#52523=CARTESIAN_POINT('Ctrl Pts',(-1.08883071512097,1.,-3.79062357974401));
#52524=CARTESIAN_POINT('Ctrl Pts',(-1.08901018614638,1.,-3.78305911299511));
#52525=CARTESIAN_POINT('Ctrl Pts',(-1.08914072791275,1.,-3.7755019940944));
#52526=CARTESIAN_POINT('Ctrl Pts',(-1.08922484204263,1.,-3.76796340094469));
#52527=CARTESIAN_POINT('Ctrl Pts',(-1.08926462734287,1.,-3.76045342580226));
#52528=CARTESIAN_POINT('Ctrl Pts',(-1.08926054632927,1.,-3.75297711748138));
#52529=CARTESIAN_POINT('Ctrl Pts',(-1.08921040494013,1.,-3.74553121371745));
#52530=CARTESIAN_POINT('Ctrl Pts',(-1.08910769013288,1.,-3.73809879348209));
#52531=CARTESIAN_POINT('Ctrl Pts',(-1.08894337390925,1.,-3.73065515162949));
#52532=CARTESIAN_POINT('Ctrl Pts',(-1.08870887220072,1.,-3.72317741369364));
#52533=CARTESIAN_POINT('Ctrl Pts',(-1.08839887334777,1.,-3.71565372339063));
#52534=CARTESIAN_POINT('Ctrl Pts',(-1.0880136731219,1.,-3.70809084139476));
#52535=CARTESIAN_POINT('Ctrl Pts',(-1.08756311291324,1.,-3.70052690909884));
#52536=CARTESIAN_POINT('Ctrl Pts',(-1.08706319540292,1.,-3.69302062410229));
#52537=CARTESIAN_POINT('Ctrl Pts',(-1.08652888882609,1.,-3.68562817420864));
#52538=CARTESIAN_POINT('Ctrl Pts',(-1.08596755755768,1.,-3.67838211685148));
#52539=CARTESIAN_POINT('Ctrl Pts',(-1.0853733414448,1.,-3.67127347729632));
#52540=CARTESIAN_POINT('Ctrl Pts',(-1.0847180992287,1.,-3.66422237895256));
#52541=CARTESIAN_POINT('Ctrl Pts',(-1.08395671077761,1.,-3.65709649161004));
#52542=CARTESIAN_POINT('Ctrl Pts',(-1.08304289898577,1.,-3.64976441208197));
#52543=CARTESIAN_POINT('Ctrl Pts',(-1.08194278850972,1.,-3.64214167843595));
#52544=CARTESIAN_POINT('Ctrl Pts',(-1.08064765719887,1.,-3.63423373196602));
#52545=CARTESIAN_POINT('Ctrl Pts',(-1.07919137290815,1.,-3.62619537902616));
#52546=CARTESIAN_POINT('Ctrl Pts',(-1.07764868137729,1.,-3.61832318504957));
#52547=CARTESIAN_POINT('Ctrl Pts',(-1.07611545402841,1.,-3.61098481349577));
#52548=CARTESIAN_POINT('Ctrl Pts',(-1.0746932716863,1.,-3.6045633988796));
#52549=CARTESIAN_POINT('Ctrl Pts',(-1.0734737254567,1.,-3.59940121154383));
#52550=CARTESIAN_POINT('Ctrl Pts',(-1.07259084660947,1.,-3.59600583195037));
#52551=CARTESIAN_POINT('Ctrl Pts',(-1.07209229745284,1.,-3.59439597));
#52552=CARTESIAN_POINT('Ctrl Pts',(-1.07183575450716,1.,-3.59379266874663));
#52553=CARTESIAN_POINT('Ctrl Pts',(-1.07171709254271,1.,-3.59363512797985));
#52554=CARTESIAN_POINT('Ctrl Pts',(-1.071677399622,1.,-3.59360648251021));
#52555=CARTESIAN_POINT('',(-1.05427041296137,0.,-4.06552750530042));
#52556=CARTESIAN_POINT('Ctrl Pts',(-0.676691979611561,-1.,-3.68843977377012));
#52557=CARTESIAN_POINT('Ctrl Pts',(-0.676691979611561,1.,-3.68843977377012));
#52558=CARTESIAN_POINT('Ctrl Pts',(-0.676620796001989,-1.,-3.68838970675497));
#52559=CARTESIAN_POINT('Ctrl Pts',(-0.676620796001989,1.,-3.68838970675497));
#52560=CARTESIAN_POINT('Ctrl Pts',(-0.676525601650856,-1.,-3.68844918121303));
#52561=CARTESIAN_POINT('Ctrl Pts',(-0.676525601650856,1.,-3.68844918121303));
#52562=CARTESIAN_POINT('Ctrl Pts',(-0.676524321061226,-1.,-3.68901718136181));
#52563=CARTESIAN_POINT('Ctrl Pts',(-0.676524321061226,1.,-3.68901718136181));
#52564=CARTESIAN_POINT('Ctrl Pts',(-0.676805811075091,-1.,-3.69073278191994));
#52565=CARTESIAN_POINT('Ctrl Pts',(-0.676805811075091,1.,-3.69073278191994));
#52566=CARTESIAN_POINT('Ctrl Pts',(-0.677621861865498,-1.,-3.69443683573598));
#52567=CARTESIAN_POINT('Ctrl Pts',(-0.677621861865498,1.,-3.69443683573598));
#52568=CARTESIAN_POINT('Ctrl Pts',(-0.678878822226026,-1.,-3.69959004073005));
#52569=CARTESIAN_POINT('Ctrl Pts',(-0.678878822226026,1.,-3.69959004073005));
#52570=CARTESIAN_POINT('Ctrl Pts',(-0.680526909710877,-1.,-3.70595722031785));
#52571=CARTESIAN_POINT('Ctrl Pts',(-0.680526909710877,1.,-3.70595722031785));
#52572=CARTESIAN_POINT('Ctrl Pts',(-0.68249234510893,-1.,-3.71319182789943));
#52573=CARTESIAN_POINT('Ctrl Pts',(-0.68249234510893,1.,-3.71319182789943));
#52574=CARTESIAN_POINT('Ctrl Pts',(-0.684691698167848,-1.,-3.7209063713926));
#52575=CARTESIAN_POINT('Ctrl Pts',(-0.684691698167848,1.,-3.7209063713926));
#52576=CARTESIAN_POINT('Ctrl Pts',(-0.687043475232355,-1.,-3.72872973554051));
#52577=CARTESIAN_POINT('Ctrl Pts',(-0.687043475232355,1.,-3.72872973554051));
#52578=CARTESIAN_POINT('Ctrl Pts',(-0.689479637354814,-1.,-3.73636374475077));
#52579=CARTESIAN_POINT('Ctrl Pts',(-0.689479637354814,1.,-3.73636374475077));
#52580=CARTESIAN_POINT('Ctrl Pts',(-0.69196008040082,-1.,-3.74365508986712));
#52581=CARTESIAN_POINT('Ctrl Pts',(-0.69196008040082,1.,-3.74365508986712));
#52582=CARTESIAN_POINT('Ctrl Pts',(-0.694474562581493,-1.,-3.75060288243455));
#52583=CARTESIAN_POINT('Ctrl Pts',(-0.694474562581493,1.,-3.75060288243455));
#52584=CARTESIAN_POINT('Ctrl Pts',(-0.697031245659744,-1.,-3.75729775767023));
#52585=CARTESIAN_POINT('Ctrl Pts',(-0.697031245659744,1.,-3.75729775767023));
#52586=CARTESIAN_POINT('Ctrl Pts',(-0.699648552230917,-1.,-3.76387780603759));
#52587=CARTESIAN_POINT('Ctrl Pts',(-0.699648552230917,1.,-3.76387780603759));
#52588=CARTESIAN_POINT('Ctrl Pts',(-0.702346356621552,-1.,-3.77048141872872));
#52589=CARTESIAN_POINT('Ctrl Pts',(-0.702346356621552,1.,-3.77048141872872));
#52590=CARTESIAN_POINT('Ctrl Pts',(-0.705135847999817,-1.,-3.77719254217129));
#52591=CARTESIAN_POINT('Ctrl Pts',(-0.705135847999817,1.,-3.77719254217129));
#52592=CARTESIAN_POINT('Ctrl Pts',(-0.708015879375459,-1.,-3.78402183336605));
#52593=CARTESIAN_POINT('Ctrl Pts',(-0.708015879375459,1.,-3.78402183336605));
#52594=CARTESIAN_POINT('Ctrl Pts',(-0.710978231689017,-1.,-3.79093694007094));
#52595=CARTESIAN_POINT('Ctrl Pts',(-0.710978231689017,1.,-3.79093694007094));
#52596=CARTESIAN_POINT('Ctrl Pts',(-0.714010733006641,-1.,-3.79788100314975));
#52597=CARTESIAN_POINT('Ctrl Pts',(-0.714010733006641,1.,-3.79788100314975));
#52598=CARTESIAN_POINT('Ctrl Pts',(-0.717100993669114,-1.,-3.80479445759309));
#52599=CARTESIAN_POINT('Ctrl Pts',(-0.717100993669114,1.,-3.80479445759309));
#52600=CARTESIAN_POINT('Ctrl Pts',(-0.720240466589236,-1.,-3.81163885127344));
#52601=CARTESIAN_POINT('Ctrl Pts',(-0.720240466589236,1.,-3.81163885127344));
#52602=CARTESIAN_POINT('Ctrl Pts',(-0.723426346019423,-1.,-3.81840802610835));
#52603=CARTESIAN_POINT('Ctrl Pts',(-0.723426346019423,1.,-3.81840802610835));
#52604=CARTESIAN_POINT('Ctrl Pts',(-0.726659281876664,-1.,-3.82511495756713));
#52605=CARTESIAN_POINT('Ctrl Pts',(-0.726659281876664,1.,-3.82511495756713));
#52606=CARTESIAN_POINT('Ctrl Pts',(-0.729942010490168,-1.,-3.83178392403383));
#52607=CARTESIAN_POINT('Ctrl Pts',(-0.729942010490168,1.,-3.83178392403383));
#52608=CARTESIAN_POINT('Ctrl Pts',(-0.733277703756078,-1.,-3.83844103658009));
#52609=CARTESIAN_POINT('Ctrl Pts',(-0.733277703756078,1.,-3.83844103658009));
#52610=CARTESIAN_POINT('Ctrl Pts',(-0.736668240497117,-1.,-3.84510432881213));
#52611=CARTESIAN_POINT('Ctrl Pts',(-0.736668240497117,1.,-3.84510432881213));
#52612=CARTESIAN_POINT('Ctrl Pts',(-0.740113146827137,-1.,-3.85177770351215));
#52613=CARTESIAN_POINT('Ctrl Pts',(-0.740113146827137,1.,-3.85177770351215));
#52614=CARTESIAN_POINT('Ctrl Pts',(-0.743610542737012,-1.,-3.85845645217594));
#52615=CARTESIAN_POINT('Ctrl Pts',(-0.743610542737012,1.,-3.85845645217594));
#52616=CARTESIAN_POINT('Ctrl Pts',(-0.747157716488871,-1.,-3.86513062969889));
#52617=CARTESIAN_POINT('Ctrl Pts',(-0.747157716488871,1.,-3.86513062969889));
#52618=CARTESIAN_POINT('Ctrl Pts',(-0.750751822383028,-1.,-3.87178914078374));
#52619=CARTESIAN_POINT('Ctrl Pts',(-0.750751822383028,1.,-3.87178914078374));
#52620=CARTESIAN_POINT('Ctrl Pts',(-0.754390577396856,-1.,-3.87842382520065));
#52621=CARTESIAN_POINT('Ctrl Pts',(-0.754390577396856,1.,-3.87842382520065));
#52622=CARTESIAN_POINT('Ctrl Pts',(-0.758072800564801,-1.,-3.88503262662689));
#52623=CARTESIAN_POINT('Ctrl Pts',(-0.758072800564801,1.,-3.88503262662689));
#52624=CARTESIAN_POINT('Ctrl Pts',(-0.76179802879397,-1.,-3.89161738162245));
#52625=CARTESIAN_POINT('Ctrl Pts',(-0.76179802879397,1.,-3.89161738162245));
#52626=CARTESIAN_POINT('Ctrl Pts',(-0.765566256401295,-1.,-3.89818233104378));
#52627=CARTESIAN_POINT('Ctrl Pts',(-0.765566256401295,1.,-3.89818233104378));
#52628=CARTESIAN_POINT('Ctrl Pts',(-0.769377629847874,-1.,-3.90473237182633));
#52629=CARTESIAN_POINT('Ctrl Pts',(-0.769377629847874,1.,-3.90473237182633));
#52630=CARTESIAN_POINT('Ctrl Pts',(-0.773232154506321,-1.,-3.91127138115243));
#52631=CARTESIAN_POINT('Ctrl Pts',(-0.773232154506321,1.,-3.91127138115243));
#52632=CARTESIAN_POINT('Ctrl Pts',(-0.777129415664956,-1.,-3.9178006233448));
#52633=CARTESIAN_POINT('Ctrl Pts',(-0.777129415664956,1.,-3.9178006233448));
#52634=CARTESIAN_POINT('Ctrl Pts',(-0.781068718228451,-1.,-3.92431956510441));
#52635=CARTESIAN_POINT('Ctrl Pts',(-0.781068718228451,1.,-3.92431956510441));
#52636=CARTESIAN_POINT('Ctrl Pts',(-0.785049202786507,-1.,-3.93082655631789));
#52637=CARTESIAN_POINT('Ctrl Pts',(-0.785049202786507,1.,-3.93082655631789));
#52638=CARTESIAN_POINT('Ctrl Pts',(-0.789069971469333,-1.,-3.93731956885676));
#52639=CARTESIAN_POINT('Ctrl Pts',(-0.789069971469333,1.,-3.93731956885676));
#52640=CARTESIAN_POINT('Ctrl Pts',(-0.793130205640961,-1.,-3.94379688971283));
#52641=CARTESIAN_POINT('Ctrl Pts',(-0.793130205640961,1.,-3.94379688971283));
#52642=CARTESIAN_POINT('Ctrl Pts',(-0.797229296085316,-1.,-3.95025788827136));
#52643=CARTESIAN_POINT('Ctrl Pts',(-0.797229296085316,1.,-3.95025788827136));
#52644=CARTESIAN_POINT('Ctrl Pts',(-0.801366797727049,-1.,-3.95670276375108));
#52645=CARTESIAN_POINT('Ctrl Pts',(-0.801366797727049,1.,-3.95670276375108));
#52646=CARTESIAN_POINT('Ctrl Pts',(-0.805542372178361,-1.,-3.96313222295815));
#52647=CARTESIAN_POINT('Ctrl Pts',(-0.805542372178361,1.,-3.96313222295815));
#52648=CARTESIAN_POINT('Ctrl Pts',(-0.809755732818091,-1.,-3.96954717513232));
#52649=CARTESIAN_POINT('Ctrl Pts',(-0.809755732818091,1.,-3.96954717513232));
#52650=CARTESIAN_POINT('Ctrl Pts',(-0.814006592328844,-1.,-3.97594844078811));
#52651=CARTESIAN_POINT('Ctrl Pts',(-0.814006592328844,1.,-3.97594844078811));
#52652=CARTESIAN_POINT('Ctrl Pts',(-0.818294599022293,-1.,-3.98233640155404));
#52653=CARTESIAN_POINT('Ctrl Pts',(-0.818294599022293,1.,-3.98233640155404));
#52654=CARTESIAN_POINT('Ctrl Pts',(-0.822619346022119,-1.,-3.98871104646485));
#52655=CARTESIAN_POINT('Ctrl Pts',(-0.822619346022119,1.,-3.98871104646485));
#52656=CARTESIAN_POINT('Ctrl Pts',(-0.826980400320789,-1.,-3.99507212784431));
#52657=CARTESIAN_POINT('Ctrl Pts',(-0.826980400320789,1.,-3.99507212784431));
#52658=CARTESIAN_POINT('Ctrl Pts',(-0.831377325741622,-1.,-4.00141928477507));
#52659=CARTESIAN_POINT('Ctrl Pts',(-0.831377325741622,1.,-4.00141928477507));
#52660=CARTESIAN_POINT('Ctrl Pts',(-0.835809705809646,-1.,-4.00775216907856));
#52661=CARTESIAN_POINT('Ctrl Pts',(-0.835809705809646,1.,-4.00775216907856));
#52662=CARTESIAN_POINT('Ctrl Pts',(-0.840277171975855,-1.,-4.01407059766103));
#52663=CARTESIAN_POINT('Ctrl Pts',(-0.840277171975855,1.,-4.01407059766103));
#52664=CARTESIAN_POINT('Ctrl Pts',(-0.844779403287745,-1.,-4.02037456798441));
#52665=CARTESIAN_POINT('Ctrl Pts',(-0.844779403287745,1.,-4.02037456798441));
#52666=CARTESIAN_POINT('Ctrl Pts',(-0.849316107474245,-1.,-4.02666418343164));
#52667=CARTESIAN_POINT('Ctrl Pts',(-0.849316107474245,1.,-4.02666418343164));
#52668=CARTESIAN_POINT('Ctrl Pts',(-0.853887006631755,-1.,-4.03293960436756));
#52669=CARTESIAN_POINT('Ctrl Pts',(-0.853887006631755,1.,-4.03293960436756));
#52670=CARTESIAN_POINT('Ctrl Pts',(-0.858491822322827,-1.,-4.03920099284773));
#52671=CARTESIAN_POINT('Ctrl Pts',(-0.858491822322827,1.,-4.03920099284773));
#52672=CARTESIAN_POINT('Ctrl Pts',(-0.863130256643259,-1.,-4.04544845048584));
#52673=CARTESIAN_POINT('Ctrl Pts',(-0.863130256643259,1.,-4.04544845048584));
#52674=CARTESIAN_POINT('Ctrl Pts',(-0.867801988859917,-1.,-4.05168199437909));
#52675=CARTESIAN_POINT('Ctrl Pts',(-0.867801988859917,1.,-4.05168199437909));
#52676=CARTESIAN_POINT('Ctrl Pts',(-0.872506694782446,-1.,-4.0579015903134));
#52677=CARTESIAN_POINT('Ctrl Pts',(-0.872506694782446,1.,-4.0579015903134));
#52678=CARTESIAN_POINT('Ctrl Pts',(-0.877244060485837,-1.,-4.06410717232905));
#52679=CARTESIAN_POINT('Ctrl Pts',(-0.877244060485837,1.,-4.06410717232905));
#52680=CARTESIAN_POINT('Ctrl Pts',(-0.882013797525692,-1.,-4.07029866694192));
#52681=CARTESIAN_POINT('Ctrl Pts',(-0.882013797525692,1.,-4.07029866694192));
#52682=CARTESIAN_POINT('Ctrl Pts',(-0.886815658358501,-1.,-4.07647601773635));
#52683=CARTESIAN_POINT('Ctrl Pts',(-0.886815658358501,1.,-4.07647601773635));
#52684=CARTESIAN_POINT('Ctrl Pts',(-0.891649447916278,-1.,-4.08263920304799));
#52685=CARTESIAN_POINT('Ctrl Pts',(-0.891649447916278,1.,-4.08263920304799));
#52686=CARTESIAN_POINT('Ctrl Pts',(-0.896515019231333,-1.,-4.08878822246833));
#52687=CARTESIAN_POINT('Ctrl Pts',(-0.896515019231333,1.,-4.08878822246833));
#52688=CARTESIAN_POINT('Ctrl Pts',(-0.900432820941675,-1.,-4.09369611522387));
#52689=CARTESIAN_POINT('Ctrl Pts',(-0.900432820941675,1.,-4.09369611522387));
#52690=CARTESIAN_POINT('Ctrl Pts',(-0.903385402441587,-1.,-4.09737067245935));
#52691=CARTESIAN_POINT('Ctrl Pts',(-0.903385402441587,1.,-4.09737067245935));
#52692=CARTESIAN_POINT('Ctrl Pts',(-0.905360112215337,-1.,-4.09981755067523));
#52693=CARTESIAN_POINT('Ctrl Pts',(-0.905360112215337,1.,-4.09981755067523));
#52694=CARTESIAN_POINT('Ctrl Pts',(-0.906349047628866,-1.,-4.10104028313088));
#52695=CARTESIAN_POINT('Ctrl Pts',(-0.906349047628866,1.,-4.10104028313088));
#52696=CARTESIAN_POINT('',(-0.676591647975427,1.,-3.68845817949586));
#52697=CARTESIAN_POINT('Ctrl Pts',(-0.676591647975428,-1.,-3.68845817949586));
#52698=CARTESIAN_POINT('Ctrl Pts',(-0.676591647975428,-0.666666666666667,
-3.68845817949586));
#52699=CARTESIAN_POINT('Ctrl Pts',(-0.676591647975428,-0.333333333333333,
-3.68845817949586));
#52700=CARTESIAN_POINT('Ctrl Pts',(-0.676591647975428,0.333333333333333,
-3.68845817949586));
#52701=CARTESIAN_POINT('Ctrl Pts',(-0.676591647975429,0.666666666666667,
-3.68845817949586));
#52702=CARTESIAN_POINT('Ctrl Pts',(-0.676591647975429,1.,-3.68845817949586));
#52703=CARTESIAN_POINT('',(-0.906349047628866,1.,-4.10104028313088));
#52704=CARTESIAN_POINT('',(-0.906349047628866,0.,-4.10104028313088));
#52705=CARTESIAN_POINT('Ctrl Pts',(-0.676591647975428,1.,-3.68845817949586));
#52706=CARTESIAN_POINT('Ctrl Pts',(-0.676569286094606,1.,-3.68850172300477));
#52707=CARTESIAN_POINT('Ctrl Pts',(-0.676535079520807,1.,-3.68869596425969));
#52708=CARTESIAN_POINT('Ctrl Pts',(-0.676580391119396,1.,-3.68934997767243));
#52709=CARTESIAN_POINT('Ctrl Pts',(-0.676867042599402,1.,-3.69101071175464));
#52710=CARTESIAN_POINT('Ctrl Pts',(-0.677621861865498,1.,-3.69443683573598));
#52711=CARTESIAN_POINT('Ctrl Pts',(-0.678878822226026,1.,-3.69959004073005));
#52712=CARTESIAN_POINT('Ctrl Pts',(-0.680526909710877,1.,-3.70595722031785));
#52713=CARTESIAN_POINT('Ctrl Pts',(-0.68249234510893,1.,-3.71319182789943));
#52714=CARTESIAN_POINT('Ctrl Pts',(-0.684691698167848,1.,-3.7209063713926));
#52715=CARTESIAN_POINT('Ctrl Pts',(-0.687043475232355,1.,-3.72872973554051));
#52716=CARTESIAN_POINT('Ctrl Pts',(-0.689479637354814,1.,-3.73636374475077));
#52717=CARTESIAN_POINT('Ctrl Pts',(-0.69196008040082,1.,-3.74365508986712));
#52718=CARTESIAN_POINT('Ctrl Pts',(-0.694474562581493,1.,-3.75060288243455));
#52719=CARTESIAN_POINT('Ctrl Pts',(-0.697031245659744,1.,-3.75729775767023));
#52720=CARTESIAN_POINT('Ctrl Pts',(-0.699648552230917,1.,-3.76387780603759));
#52721=CARTESIAN_POINT('Ctrl Pts',(-0.702346356621552,1.,-3.77048141872872));
#52722=CARTESIAN_POINT('Ctrl Pts',(-0.705135847999817,1.,-3.77719254217129));
#52723=CARTESIAN_POINT('Ctrl Pts',(-0.708015879375459,1.,-3.78402183336605));
#52724=CARTESIAN_POINT('Ctrl Pts',(-0.710978231689017,1.,-3.79093694007094));
#52725=CARTESIAN_POINT('Ctrl Pts',(-0.714010733006641,1.,-3.79788100314975));
#52726=CARTESIAN_POINT('Ctrl Pts',(-0.717100993669114,1.,-3.80479445759309));
#52727=CARTESIAN_POINT('Ctrl Pts',(-0.720240466589236,1.,-3.81163885127344));
#52728=CARTESIAN_POINT('Ctrl Pts',(-0.723426346019423,1.,-3.81840802610835));
#52729=CARTESIAN_POINT('Ctrl Pts',(-0.726659281876664,1.,-3.82511495756713));
#52730=CARTESIAN_POINT('Ctrl Pts',(-0.729942010490168,1.,-3.83178392403383));
#52731=CARTESIAN_POINT('Ctrl Pts',(-0.733277703756078,1.,-3.83844103658009));
#52732=CARTESIAN_POINT('Ctrl Pts',(-0.736668240497117,1.,-3.84510432881213));
#52733=CARTESIAN_POINT('Ctrl Pts',(-0.740113146827137,1.,-3.85177770351215));
#52734=CARTESIAN_POINT('Ctrl Pts',(-0.743610542737012,1.,-3.85845645217594));
#52735=CARTESIAN_POINT('Ctrl Pts',(-0.747157716488871,1.,-3.86513062969889));
#52736=CARTESIAN_POINT('Ctrl Pts',(-0.750751822383028,1.,-3.87178914078374));
#52737=CARTESIAN_POINT('Ctrl Pts',(-0.754390577396856,1.,-3.87842382520065));
#52738=CARTESIAN_POINT('Ctrl Pts',(-0.758072800564801,1.,-3.88503262662689));
#52739=CARTESIAN_POINT('Ctrl Pts',(-0.76179802879397,1.,-3.89161738162245));
#52740=CARTESIAN_POINT('Ctrl Pts',(-0.765566256401295,1.,-3.89818233104378));
#52741=CARTESIAN_POINT('Ctrl Pts',(-0.769377629847874,1.,-3.90473237182633));
#52742=CARTESIAN_POINT('Ctrl Pts',(-0.773232154506321,1.,-3.91127138115243));
#52743=CARTESIAN_POINT('Ctrl Pts',(-0.777129415664956,1.,-3.9178006233448));
#52744=CARTESIAN_POINT('Ctrl Pts',(-0.781068718228451,1.,-3.92431956510441));
#52745=CARTESIAN_POINT('Ctrl Pts',(-0.785049202786507,1.,-3.93082655631789));
#52746=CARTESIAN_POINT('Ctrl Pts',(-0.789069971469333,1.,-3.93731956885676));
#52747=CARTESIAN_POINT('Ctrl Pts',(-0.793130205640961,1.,-3.94379688971283));
#52748=CARTESIAN_POINT('Ctrl Pts',(-0.797229296085316,1.,-3.95025788827136));
#52749=CARTESIAN_POINT('Ctrl Pts',(-0.801366797727049,1.,-3.95670276375108));
#52750=CARTESIAN_POINT('Ctrl Pts',(-0.805542372178361,1.,-3.96313222295815));
#52751=CARTESIAN_POINT('Ctrl Pts',(-0.809755732818091,1.,-3.96954717513232));
#52752=CARTESIAN_POINT('Ctrl Pts',(-0.814006592328844,1.,-3.97594844078811));
#52753=CARTESIAN_POINT('Ctrl Pts',(-0.818294599022293,1.,-3.98233640155404));
#52754=CARTESIAN_POINT('Ctrl Pts',(-0.822619346022119,1.,-3.98871104646485));
#52755=CARTESIAN_POINT('Ctrl Pts',(-0.826980400320789,1.,-3.99507212784431));
#52756=CARTESIAN_POINT('Ctrl Pts',(-0.831377325741622,1.,-4.00141928477507));
#52757=CARTESIAN_POINT('Ctrl Pts',(-0.835809705809646,1.,-4.00775216907856));
#52758=CARTESIAN_POINT('Ctrl Pts',(-0.840277171975855,1.,-4.01407059766103));
#52759=CARTESIAN_POINT('Ctrl Pts',(-0.844779403287745,1.,-4.02037456798441));
#52760=CARTESIAN_POINT('Ctrl Pts',(-0.849316107474245,1.,-4.02666418343164));
#52761=CARTESIAN_POINT('Ctrl Pts',(-0.853887006631755,1.,-4.03293960436756));
#52762=CARTESIAN_POINT('Ctrl Pts',(-0.858491822322827,1.,-4.03920099284773));
#52763=CARTESIAN_POINT('Ctrl Pts',(-0.863130256643259,1.,-4.04544845048584));
#52764=CARTESIAN_POINT('Ctrl Pts',(-0.867801988859917,1.,-4.05168199437909));
#52765=CARTESIAN_POINT('Ctrl Pts',(-0.872506694782446,1.,-4.0579015903134));
#52766=CARTESIAN_POINT('Ctrl Pts',(-0.877244060485837,1.,-4.06410717232905));
#52767=CARTESIAN_POINT('Ctrl Pts',(-0.882013797525692,1.,-4.07029866694192));
#52768=CARTESIAN_POINT('Ctrl Pts',(-0.886815658358501,1.,-4.07647601773635));
#52769=CARTESIAN_POINT('Ctrl Pts',(-0.891649447916278,1.,-4.08263920304799));
#52770=CARTESIAN_POINT('Ctrl Pts',(-0.896515019231333,1.,-4.08878822246833));
#52771=CARTESIAN_POINT('Ctrl Pts',(-0.900432820941675,1.,-4.09369611522387));
#52772=CARTESIAN_POINT('Ctrl Pts',(-0.903385402441587,1.,-4.09737067245935));
#52773=CARTESIAN_POINT('Ctrl Pts',(-0.905360112215337,1.,-4.09981755067523));
#52774=CARTESIAN_POINT('Ctrl Pts',(-0.906349047628866,1.,-4.10104028313088));
#52775=CARTESIAN_POINT('Origin',(-0.906349047628866,0.,-4.10104028313088));
#52776=CARTESIAN_POINT('',(-1.05427041296137,1.,-4.06552750530042));
#52777=CARTESIAN_POINT('Origin',(0.,0.,0.));
#52778=CARTESIAN_POINT('',(-0.496319364829374,1.,-3.71701050416802));
#52779=CARTESIAN_POINT('Origin',(0.,1.,0.));
#52780=CARTESIAN_POINT('Ctrl Pts',(-0.496319364829374,1.,-3.71701050416802));
#52781=CARTESIAN_POINT('Ctrl Pts',(-0.496319364829374,0.666666666666667,
-3.71701050416802));
#52782=CARTESIAN_POINT('Ctrl Pts',(-0.496319364829374,0.333333333333333,
-3.71701050416802));
#52783=CARTESIAN_POINT('Ctrl Pts',(-0.496319364829374,-0.333333333333333,
-3.71701050416802));
#52784=CARTESIAN_POINT('Ctrl Pts',(-0.496319364829374,-0.666666666666667,
-3.71701050416802));
#52785=CARTESIAN_POINT('Ctrl Pts',(-0.496319364829374,-1.,-3.71701050416802));
#52786=CARTESIAN_POINT('Ctrl Pts',(-0.405301974318349,-1.,-4.18039834341342));
#52787=CARTESIAN_POINT('Ctrl Pts',(-0.405301974318349,1.,-4.18039834341342));
#52788=CARTESIAN_POINT('Ctrl Pts',(-0.405864662679631,-1.,-4.17892985789908));
#52789=CARTESIAN_POINT('Ctrl Pts',(-0.405864662679631,1.,-4.17892985789908));
#52790=CARTESIAN_POINT('Ctrl Pts',(-0.406986596326602,-1.,-4.17599251955585));
#52791=CARTESIAN_POINT('Ctrl Pts',(-0.406986596326602,1.,-4.17599251955585));
#52792=CARTESIAN_POINT('Ctrl Pts',(-0.408659167570153,-1.,-4.17158541009947));
#52793=CARTESIAN_POINT('Ctrl Pts',(-0.408659167570153,1.,-4.17158541009947));
#52794=CARTESIAN_POINT('Ctrl Pts',(-0.410868596148614,-1.,-4.16570705940731));
#52795=CARTESIAN_POINT('Ctrl Pts',(-0.410868596148614,1.,-4.16570705940731));
#52796=CARTESIAN_POINT('Ctrl Pts',(-0.413595877953269,-1.,-4.1583554501909));
#52797=CARTESIAN_POINT('Ctrl Pts',(-0.413595877953269,1.,-4.1583554501909));
#52798=CARTESIAN_POINT('Ctrl Pts',(-0.416288556008986,-1.,-4.15100018950989));
#52799=CARTESIAN_POINT('Ctrl Pts',(-0.416288556008986,1.,-4.15100018950989));
#52800=CARTESIAN_POINT('Ctrl Pts',(-0.4189464906678,-1.,-4.14364132317223));
#52801=CARTESIAN_POINT('Ctrl Pts',(-0.4189464906678,1.,-4.14364132317223));
#52802=CARTESIAN_POINT('Ctrl Pts',(-0.421569503103971,-1.,-4.13627893206433));
#52803=CARTESIAN_POINT('Ctrl Pts',(-0.421569503103971,1.,-4.13627893206433));
#52804=CARTESIAN_POINT('Ctrl Pts',(-0.424157375323155,-1.,-4.1289131463371));
#52805=CARTESIAN_POINT('Ctrl Pts',(-0.424157375323155,1.,-4.1289131463371));
#52806=CARTESIAN_POINT('Ctrl Pts',(-0.426709855706243,-1.,-4.1215441250121));
#52807=CARTESIAN_POINT('Ctrl Pts',(-0.426709855706243,1.,-4.1215441250121));
#52808=CARTESIAN_POINT('Ctrl Pts',(-0.429226666075372,-1.,-4.1141720278277));
#52809=CARTESIAN_POINT('Ctrl Pts',(-0.429226666075372,1.,-4.1141720278277));
#52810=CARTESIAN_POINT('Ctrl Pts',(-0.431707508679772,-1.,-4.10679698750219));
#52811=CARTESIAN_POINT('Ctrl Pts',(-0.431707508679772,1.,-4.10679698750219));
#52812=CARTESIAN_POINT('Ctrl Pts',(-0.434152073200643,-1.,-4.09941908688567));
#52813=CARTESIAN_POINT('Ctrl Pts',(-0.434152073200643,1.,-4.09941908688567));
#52814=CARTESIAN_POINT('Ctrl Pts',(-0.436560044913814,-1.,-4.09203832139439));
#52815=CARTESIAN_POINT('Ctrl Pts',(-0.436560044913814,1.,-4.09203832139439));
#52816=CARTESIAN_POINT('Ctrl Pts',(-0.438931108931613,-1.,-4.08465462294625));
#52817=CARTESIAN_POINT('Ctrl Pts',(-0.438931108931613,1.,-4.08465462294625));
#52818=CARTESIAN_POINT('Ctrl Pts',(-0.441264951396587,-1.,-4.07726792490256));
#52819=CARTESIAN_POINT('Ctrl Pts',(-0.441264951396587,1.,-4.07726792490256));
#52820=CARTESIAN_POINT('Ctrl Pts',(-0.443561262395408,-1.,-4.0698782192577));
#52821=CARTESIAN_POINT('Ctrl Pts',(-0.443561262395408,1.,-4.0698782192577));
#52822=CARTESIAN_POINT('Ctrl Pts',(-0.445819737468478,-1.,-4.06248560760596));
#52823=CARTESIAN_POINT('Ctrl Pts',(-0.445819737468478,1.,-4.06248560760596));
#52824=CARTESIAN_POINT('Ctrl Pts',(-0.448040082683976,-1.,-4.05509037796815));
#52825=CARTESIAN_POINT('Ctrl Pts',(-0.448040082683976,1.,-4.05509037796815));
#52826=CARTESIAN_POINT('Ctrl Pts',(-0.450222009543774,-1.,-4.0476929901797));
#52827=CARTESIAN_POINT('Ctrl Pts',(-0.450222009543774,1.,-4.0476929901797));
#52828=CARTESIAN_POINT('Ctrl Pts',(-0.452365214748779,-1.,-4.0402939222793));
#52829=CARTESIAN_POINT('Ctrl Pts',(-0.452365214748779,1.,-4.0402939222793));
#52830=CARTESIAN_POINT('Ctrl Pts',(-0.454469363020495,-1.,-4.03289354362745));
#52831=CARTESIAN_POINT('Ctrl Pts',(-0.454469363020495,1.,-4.03289354362745));
#52832=CARTESIAN_POINT('Ctrl Pts',(-0.456534070784968,-1.,-4.02549199038414));
#52833=CARTESIAN_POINT('Ctrl Pts',(-0.456534070784968,1.,-4.02549199038414));
#52834=CARTESIAN_POINT('Ctrl Pts',(-0.458558885637001,-1.,-4.01808900827647));
#52835=CARTESIAN_POINT('Ctrl Pts',(-0.458558885637001,1.,-4.01808900827647));
#52836=CARTESIAN_POINT('Ctrl Pts',(-0.460543280768577,-1.,-4.01068390573469));
#52837=CARTESIAN_POINT('Ctrl Pts',(-0.460543280768577,1.,-4.01068390573469));
#52838=CARTESIAN_POINT('Ctrl Pts',(-0.462486702616252,-1.,-4.00327590659129));
#52839=CARTESIAN_POINT('Ctrl Pts',(-0.462486702616252,1.,-4.00327590659129));
#52840=CARTESIAN_POINT('Ctrl Pts',(-0.464388610938995,-1.,-3.99586444320134));
#52841=CARTESIAN_POINT('Ctrl Pts',(-0.464388610938995,1.,-3.99586444320134));
#52842=CARTESIAN_POINT('Ctrl Pts',(-0.466248520883034,-1.,-3.98844946363258));
#52843=CARTESIAN_POINT('Ctrl Pts',(-0.466248520883034,1.,-3.98844946363258));
#52844=CARTESIAN_POINT('Ctrl Pts',(-0.46806604792014,-1.,-3.98103175589349));
#52845=CARTESIAN_POINT('Ctrl Pts',(-0.46806604792014,1.,-3.98103175589349));
#52846=CARTESIAN_POINT('Ctrl Pts',(-0.469840942829878,-1.,-3.97361320212413));
#52847=CARTESIAN_POINT('Ctrl Pts',(-0.469840942829878,1.,-3.97361320212413));
#52848=CARTESIAN_POINT('Ctrl Pts',(-0.471572978413493,-1.,-3.96619600864626));
#52849=CARTESIAN_POINT('Ctrl Pts',(-0.471572978413493,1.,-3.96619600864626));
#52850=CARTESIAN_POINT('Ctrl Pts',(-0.473261847236296,-1.,-3.95878201038332));
#52851=CARTESIAN_POINT('Ctrl Pts',(-0.473261847236296,1.,-3.95878201038332));
#52852=CARTESIAN_POINT('Ctrl Pts',(-0.47490705302179,-1.,-3.95137192932898));
#52853=CARTESIAN_POINT('Ctrl Pts',(-0.47490705302179,1.,-3.95137192932898));
#52854=CARTESIAN_POINT('Ctrl Pts',(-0.476507810658535,-1.,-3.94396469119385));
#52855=CARTESIAN_POINT('Ctrl Pts',(-0.476507810658535,1.,-3.94396469119385));
#52856=CARTESIAN_POINT('Ctrl Pts',(-0.478062927140957,-1.,-3.93655660689819));
#52857=CARTESIAN_POINT('Ctrl Pts',(-0.478062927140957,1.,-3.93655660689819));
#52858=CARTESIAN_POINT('Ctrl Pts',(-0.479571028525566,-1.,-3.92914297392067));
#52859=CARTESIAN_POINT('Ctrl Pts',(-0.479571028525566,1.,-3.92914297392067));
#52860=CARTESIAN_POINT('Ctrl Pts',(-0.481030798910735,-1.,-3.92171976072334));
#52861=CARTESIAN_POINT('Ctrl Pts',(-0.481030798910735,1.,-3.92171976072334));
#52862=CARTESIAN_POINT('Ctrl Pts',(-0.482441230340709,-1.,-3.91428536373749));
#52863=CARTESIAN_POINT('Ctrl Pts',(-0.482441230340709,1.,-3.91428536373749));
#52864=CARTESIAN_POINT('Ctrl Pts',(-0.483801835089161,-1.,-3.90684210358063));
#52865=CARTESIAN_POINT('Ctrl Pts',(-0.483801835089161,1.,-3.90684210358063));
#52866=CARTESIAN_POINT('Ctrl Pts',(-0.485112963522246,-1.,-3.89939844658529));
#52867=CARTESIAN_POINT('Ctrl Pts',(-0.485112963522246,1.,-3.89939844658529));
#52868=CARTESIAN_POINT('Ctrl Pts',(-0.486375337854133,-1.,-3.89196582437574));
#52869=CARTESIAN_POINT('Ctrl Pts',(-0.486375337854133,1.,-3.89196582437574));
#52870=CARTESIAN_POINT('Ctrl Pts',(-0.487589452275179,-1.,-3.88455453328156));
#52871=CARTESIAN_POINT('Ctrl Pts',(-0.487589452275179,1.,-3.88455453328156));
#52872=CARTESIAN_POINT('Ctrl Pts',(-0.488754973798281,-1.,-3.87716963231115));
#52873=CARTESIAN_POINT('Ctrl Pts',(-0.488754973798281,1.,-3.87716963231115));
#52874=CARTESIAN_POINT('Ctrl Pts',(-0.489870245704899,-1.,-3.86980755613694));
#52875=CARTESIAN_POINT('Ctrl Pts',(-0.489870245704899,1.,-3.86980755613694));
#52876=CARTESIAN_POINT('Ctrl Pts',(-0.490931482170849,-1.,-3.86245057319215));
#52877=CARTESIAN_POINT('Ctrl Pts',(-0.490931482170849,1.,-3.86245057319215));
#52878=CARTESIAN_POINT('Ctrl Pts',(-0.49193363108376,-1.,-3.85507287020223));
#52879=CARTESIAN_POINT('Ctrl Pts',(-0.49193363108376,1.,-3.85507287020223));
#52880=CARTESIAN_POINT('Ctrl Pts',(-0.492871792414095,-1.,-3.84765051147965));
#52881=CARTESIAN_POINT('Ctrl Pts',(-0.492871792414095,1.,-3.84765051147965));
#52882=CARTESIAN_POINT('Ctrl Pts',(-0.493742574629117,-1.,-3.84017095578438));
#52883=CARTESIAN_POINT('Ctrl Pts',(-0.493742574629117,1.,-3.84017095578438));
#52884=CARTESIAN_POINT('Ctrl Pts',(-0.494545212256425,-1.,-3.8326409268245));
#52885=CARTESIAN_POINT('Ctrl Pts',(-0.494545212256425,1.,-3.8326409268245));
#52886=CARTESIAN_POINT('Ctrl Pts',(-0.495283458893903,-1.,-3.82509963594156));
#52887=CARTESIAN_POINT('Ctrl Pts',(-0.495283458893903,1.,-3.82509963594156));
#52888=CARTESIAN_POINT('Ctrl Pts',(-0.495963937875572,-1.,-3.81760756144099));
#52889=CARTESIAN_POINT('Ctrl Pts',(-0.495963937875572,1.,-3.81760756144099));
#52890=CARTESIAN_POINT('Ctrl Pts',(-0.496592643443789,-1.,-3.81022254090909));
#52891=CARTESIAN_POINT('Ctrl Pts',(-0.496592643443789,1.,-3.81022254090909));
#52892=CARTESIAN_POINT('Ctrl Pts',(-0.497171756201091,-1.,-3.80297788298545));
#52893=CARTESIAN_POINT('Ctrl Pts',(-0.497171756201091,1.,-3.80297788298545));
#52894=CARTESIAN_POINT('Ctrl Pts',(-0.49769689210058,-1.,-3.79586380669959));
#52895=CARTESIAN_POINT('Ctrl Pts',(-0.49769689210058,1.,-3.79586380669959));
#52896=CARTESIAN_POINT('Ctrl Pts',(-0.498152751800819,-1.,-3.78879701661152));
#52897=CARTESIAN_POINT('Ctrl Pts',(-0.498152751800819,1.,-3.78879701661152));
#52898=CARTESIAN_POINT('Ctrl Pts',(-0.498515471679378,-1.,-3.78163975337189));
#52899=CARTESIAN_POINT('Ctrl Pts',(-0.498515471679378,1.,-3.78163975337189));
#52900=CARTESIAN_POINT('Ctrl Pts',(-0.498759900365687,-1.,-3.77425499225089));
#52901=CARTESIAN_POINT('Ctrl Pts',(-0.498759900365687,1.,-3.77425499225089));
#52902=CARTESIAN_POINT('Ctrl Pts',(-0.498865792335185,-1.,-3.76655401191144));
#52903=CARTESIAN_POINT('Ctrl Pts',(-0.498865792335185,1.,-3.76655401191144));
#52904=CARTESIAN_POINT('Ctrl Pts',(-0.498823681615513,-1.,-3.75854082221127));
#52905=CARTESIAN_POINT('Ctrl Pts',(-0.498823681615513,1.,-3.75854082221127));
#52906=CARTESIAN_POINT('Ctrl Pts',(-0.498642802042929,-1.,-3.75037362168103));
#52907=CARTESIAN_POINT('Ctrl Pts',(-0.498642802042929,1.,-3.75037362168103));
#52908=CARTESIAN_POINT('Ctrl Pts',(-0.498350586058176,-1.,-3.74235701735109));
#52909=CARTESIAN_POINT('Ctrl Pts',(-0.498350586058176,1.,-3.74235701735109));
#52910=CARTESIAN_POINT('Ctrl Pts',(-0.497984209510495,-1.,-3.73486914372834));
#52911=CARTESIAN_POINT('Ctrl Pts',(-0.497984209510495,1.,-3.73486914372834));
#52912=CARTESIAN_POINT('Ctrl Pts',(-0.497584067153279,-1.,-3.72830430904794));
#52913=CARTESIAN_POINT('Ctrl Pts',(-0.497584067153279,1.,-3.72830430904794));
#52914=CARTESIAN_POINT('Ctrl Pts',(-0.497187079575794,-1.,-3.72301489774241));
#52915=CARTESIAN_POINT('Ctrl Pts',(-0.497187079575794,1.,-3.72301489774241));
#52916=CARTESIAN_POINT('Ctrl Pts',(-0.496818574419989,-1.,-3.71923995965807));
#52917=CARTESIAN_POINT('Ctrl Pts',(-0.496818574419989,1.,-3.71923995965807));
#52918=CARTESIAN_POINT('Ctrl Pts',(-0.496556137603856,-1.,-3.71752134136931));
#52919=CARTESIAN_POINT('Ctrl Pts',(-0.496556137603856,1.,-3.71752134136931));
#52920=CARTESIAN_POINT('Ctrl Pts',(-0.496379397992182,-1.,-3.71698153685229));
#52921=CARTESIAN_POINT('Ctrl Pts',(-0.496379397992182,1.,-3.71698153685229));
#52922=CARTESIAN_POINT('Ctrl Pts',(-0.496270484166233,-1.,-3.71695438995598));
#52923=CARTESIAN_POINT('Ctrl Pts',(-0.496270484166233,1.,-3.71695438995598));
#52924=CARTESIAN_POINT('Ctrl Pts',(-0.496218256089212,-1.,-3.71702400346349));
#52925=CARTESIAN_POINT('Ctrl Pts',(-0.496218256089212,1.,-3.71702400346349));
#52926=CARTESIAN_POINT('',(-0.405301974318349,1.,-4.18039834341342));
#52927=CARTESIAN_POINT('Ctrl Pts',(-0.405301974318349,1.,-4.18039834341342));
#52928=CARTESIAN_POINT('Ctrl Pts',(-0.405864662679631,1.,-4.17892985789908));
#52929=CARTESIAN_POINT('Ctrl Pts',(-0.406986596326602,1.,-4.17599251955585));
#52930=CARTESIAN_POINT('Ctrl Pts',(-0.408659167570153,1.,-4.17158541009947));
#52931=CARTESIAN_POINT('Ctrl Pts',(-0.410868596148614,1.,-4.16570705940731));
#52932=CARTESIAN_POINT('Ctrl Pts',(-0.413595877953269,1.,-4.1583554501909));
#52933=CARTESIAN_POINT('Ctrl Pts',(-0.416288556008986,1.,-4.15100018950989));
#52934=CARTESIAN_POINT('Ctrl Pts',(-0.4189464906678,1.,-4.14364132317223));
#52935=CARTESIAN_POINT('Ctrl Pts',(-0.421569503103971,1.,-4.13627893206433));
#52936=CARTESIAN_POINT('Ctrl Pts',(-0.424157375323155,1.,-4.1289131463371));
#52937=CARTESIAN_POINT('Ctrl Pts',(-0.426709855706243,1.,-4.1215441250121));
#52938=CARTESIAN_POINT('Ctrl Pts',(-0.429226666075372,1.,-4.1141720278277));
#52939=CARTESIAN_POINT('Ctrl Pts',(-0.431707508679772,1.,-4.10679698750219));
#52940=CARTESIAN_POINT('Ctrl Pts',(-0.434152073200643,1.,-4.09941908688567));
#52941=CARTESIAN_POINT('Ctrl Pts',(-0.436560044913814,1.,-4.09203832139439));
#52942=CARTESIAN_POINT('Ctrl Pts',(-0.438931108931613,1.,-4.08465462294625));
#52943=CARTESIAN_POINT('Ctrl Pts',(-0.441264951396587,1.,-4.07726792490256));
#52944=CARTESIAN_POINT('Ctrl Pts',(-0.443561262395408,1.,-4.0698782192577));
#52945=CARTESIAN_POINT('Ctrl Pts',(-0.445819737468478,1.,-4.06248560760596));
#52946=CARTESIAN_POINT('Ctrl Pts',(-0.448040082683976,1.,-4.05509037796815));
#52947=CARTESIAN_POINT('Ctrl Pts',(-0.450222009543774,1.,-4.0476929901797));
#52948=CARTESIAN_POINT('Ctrl Pts',(-0.452365214748779,1.,-4.0402939222793));
#52949=CARTESIAN_POINT('Ctrl Pts',(-0.454469363020495,1.,-4.03289354362745));
#52950=CARTESIAN_POINT('Ctrl Pts',(-0.456534070784968,1.,-4.02549199038414));
#52951=CARTESIAN_POINT('Ctrl Pts',(-0.458558885637001,1.,-4.01808900827647));
#52952=CARTESIAN_POINT('Ctrl Pts',(-0.460543280768577,1.,-4.01068390573469));
#52953=CARTESIAN_POINT('Ctrl Pts',(-0.462486702616252,1.,-4.00327590659129));
#52954=CARTESIAN_POINT('Ctrl Pts',(-0.464388610938995,1.,-3.99586444320134));
#52955=CARTESIAN_POINT('Ctrl Pts',(-0.466248520883034,1.,-3.98844946363258));
#52956=CARTESIAN_POINT('Ctrl Pts',(-0.46806604792014,1.,-3.98103175589349));
#52957=CARTESIAN_POINT('Ctrl Pts',(-0.469840942829878,1.,-3.97361320212413));
#52958=CARTESIAN_POINT('Ctrl Pts',(-0.471572978413493,1.,-3.96619600864626));
#52959=CARTESIAN_POINT('Ctrl Pts',(-0.473261847236296,1.,-3.95878201038332));
#52960=CARTESIAN_POINT('Ctrl Pts',(-0.47490705302179,1.,-3.95137192932898));
#52961=CARTESIAN_POINT('Ctrl Pts',(-0.476507810658535,1.,-3.94396469119385));
#52962=CARTESIAN_POINT('Ctrl Pts',(-0.478062927140957,1.,-3.93655660689819));
#52963=CARTESIAN_POINT('Ctrl Pts',(-0.479571028525566,1.,-3.92914297392067));
#52964=CARTESIAN_POINT('Ctrl Pts',(-0.481030798910735,1.,-3.92171976072334));
#52965=CARTESIAN_POINT('Ctrl Pts',(-0.482441230340709,1.,-3.91428536373749));
#52966=CARTESIAN_POINT('Ctrl Pts',(-0.483801835089161,1.,-3.90684210358063));
#52967=CARTESIAN_POINT('Ctrl Pts',(-0.485112963522246,1.,-3.89939844658529));
#52968=CARTESIAN_POINT('Ctrl Pts',(-0.486375337854133,1.,-3.89196582437574));
#52969=CARTESIAN_POINT('Ctrl Pts',(-0.487589452275179,1.,-3.88455453328156));
#52970=CARTESIAN_POINT('Ctrl Pts',(-0.488754973798281,1.,-3.87716963231115));
#52971=CARTESIAN_POINT('Ctrl Pts',(-0.489870245704899,1.,-3.86980755613694));
#52972=CARTESIAN_POINT('Ctrl Pts',(-0.490931482170849,1.,-3.86245057319215));
#52973=CARTESIAN_POINT('Ctrl Pts',(-0.49193363108376,1.,-3.85507287020223));
#52974=CARTESIAN_POINT('Ctrl Pts',(-0.492871792414095,1.,-3.84765051147965));
#52975=CARTESIAN_POINT('Ctrl Pts',(-0.493742574629117,1.,-3.84017095578438));
#52976=CARTESIAN_POINT('Ctrl Pts',(-0.494545212256425,1.,-3.8326409268245));
#52977=CARTESIAN_POINT('Ctrl Pts',(-0.495283458893903,1.,-3.82509963594156));
#52978=CARTESIAN_POINT('Ctrl Pts',(-0.495963937875572,1.,-3.81760756144099));
#52979=CARTESIAN_POINT('Ctrl Pts',(-0.496592643443789,1.,-3.81022254090909));
#52980=CARTESIAN_POINT('Ctrl Pts',(-0.497171756201091,1.,-3.80297788298545));
#52981=CARTESIAN_POINT('Ctrl Pts',(-0.49769689210058,1.,-3.79586380669959));
#52982=CARTESIAN_POINT('Ctrl Pts',(-0.498152751800819,1.,-3.78879701661152));
#52983=CARTESIAN_POINT('Ctrl Pts',(-0.498515471679378,1.,-3.78163975337189));
#52984=CARTESIAN_POINT('Ctrl Pts',(-0.498759900365687,1.,-3.77425499225089));
#52985=CARTESIAN_POINT('Ctrl Pts',(-0.498865792335185,1.,-3.76655401191144));
#52986=CARTESIAN_POINT('Ctrl Pts',(-0.498823681615513,1.,-3.75854082221127));
#52987=CARTESIAN_POINT('Ctrl Pts',(-0.498642802042929,1.,-3.75037362168103));
#52988=CARTESIAN_POINT('Ctrl Pts',(-0.498350586058176,1.,-3.74235701735109));
#52989=CARTESIAN_POINT('Ctrl Pts',(-0.497984209510495,1.,-3.73486914372834));
#52990=CARTESIAN_POINT('Ctrl Pts',(-0.497584067153279,1.,-3.72830430904794));
#52991=CARTESIAN_POINT('Ctrl Pts',(-0.497187079575794,1.,-3.72301489774241));
#52992=CARTESIAN_POINT('Ctrl Pts',(-0.496846224822535,1.,-3.7195232082259));
#52993=CARTESIAN_POINT('Ctrl Pts',(-0.496605651526314,1.,-3.71785517607694));
#52994=CARTESIAN_POINT('Ctrl Pts',(-0.496446644158827,1.,-3.71721917030465));
#52995=CARTESIAN_POINT('Ctrl Pts',(-0.496354087925646,1.,-3.71704500630521));
#52996=CARTESIAN_POINT('Ctrl Pts',(-0.496319364829374,1.,-3.71701050416802));
#52997=CARTESIAN_POINT('',(-0.405301974318349,0.,-4.18039834341342));
#52998=CARTESIAN_POINT('Ctrl Pts',(-0.0913616755937422,-1.,-3.74888690736767));
#52999=CARTESIAN_POINT('Ctrl Pts',(-0.0913616755937422,1.,-3.74888690736767));
#53000=CARTESIAN_POINT('Ctrl Pts',(-0.0912992005792586,-1.,-3.74882632119067));
#53001=CARTESIAN_POINT('Ctrl Pts',(-0.0912992005792586,1.,-3.74882632119067));
#53002=CARTESIAN_POINT('Ctrl Pts',(-0.0911958743735236,-1.,-3.74887017174206));
#53003=CARTESIAN_POINT('Ctrl Pts',(-0.0911958743735236,1.,-3.74887017174206));
#53004=CARTESIAN_POINT('Ctrl Pts',(-0.0911057547506601,-1.,-3.74943097853811));
#53005=CARTESIAN_POINT('Ctrl Pts',(-0.0911057547506601,1.,-3.74943097853811));
#53006=CARTESIAN_POINT('Ctrl Pts',(-0.0911154000998143,-1.,-3.75116949194623));
#53007=CARTESIAN_POINT('Ctrl Pts',(-0.0911154000998143,1.,-3.75116949194623));
#53008=CARTESIAN_POINT('Ctrl Pts',(-0.09134196227364,-1.,-3.75495560118212));
#53009=CARTESIAN_POINT('Ctrl Pts',(-0.09134196227364,1.,-3.75495560118212));
#53010=CARTESIAN_POINT('Ctrl Pts',(-0.0917773084998337,-1.,-3.76024199359303));
#53011=CARTESIAN_POINT('Ctrl Pts',(-0.0917773084998337,1.,-3.76024199359303));
#53012=CARTESIAN_POINT('Ctrl Pts',(-0.0924090589602692,-1.,-3.76678860031841));
#53013=CARTESIAN_POINT('Ctrl Pts',(-0.0924090589602692,1.,-3.76678860031841));
#53014=CARTESIAN_POINT('Ctrl Pts',(-0.093218554620318,-1.,-3.77424159971059));
#53015=CARTESIAN_POINT('Ctrl Pts',(-0.093218554620318,1.,-3.77424159971059));
#53016=CARTESIAN_POINT('Ctrl Pts',(-0.0941840095090815,-1.,-3.782205218991));
#53017=CARTESIAN_POINT('Ctrl Pts',(-0.0941840095090815,1.,-3.782205218991));
#53018=CARTESIAN_POINT('Ctrl Pts',(-0.0952829885100802,-1.,-3.79030016353111));
#53019=CARTESIAN_POINT('Ctrl Pts',(-0.0952829885100802,1.,-3.79030016353111));
#53020=CARTESIAN_POINT('Ctrl Pts',(-0.0964949352873133,-1.,-3.79822128513845));
#53021=CARTESIAN_POINT('Ctrl Pts',(-0.0964949352873133,1.,-3.79822128513845));
#53022=CARTESIAN_POINT('Ctrl Pts',(-0.0978042222906645,-1.,-3.80581088847809));
#53023=CARTESIAN_POINT('Ctrl Pts',(-0.0978042222906645,1.,-3.80581088847809));
#53024=CARTESIAN_POINT('Ctrl Pts',(-0.0992008728096516,-1.,-3.81306649386461));
#53025=CARTESIAN_POINT('Ctrl Pts',(-0.0992008728096516,1.,-3.81306649386461));
#53026=CARTESIAN_POINT('Ctrl Pts',(-0.100678769650632,-1.,-3.82007889742625));
#53027=CARTESIAN_POINT('Ctrl Pts',(-0.100678769650632,1.,-3.82007889742625));
#53028=CARTESIAN_POINT('Ctrl Pts',(-0.102234506488456,-1.,-3.82698737143255));
#53029=CARTESIAN_POINT('Ctrl Pts',(-0.102234506488456,1.,-3.82698737143255));
#53030=CARTESIAN_POINT('Ctrl Pts',(-0.103866063811623,-1.,-3.83393171228002));
#53031=CARTESIAN_POINT('Ctrl Pts',(-0.103866063811623,1.,-3.83393171228002));
#53032=CARTESIAN_POINT('Ctrl Pts',(-0.105571360916569,-1.,-3.84099658324803));
#53033=CARTESIAN_POINT('Ctrl Pts',(-0.105571360916569,1.,-3.84099658324803));
#53034=CARTESIAN_POINT('Ctrl Pts',(-0.107347597812184,-1.,-3.84819233070317));
#53035=CARTESIAN_POINT('Ctrl Pts',(-0.107347597812184,1.,-3.84819233070317));
#53036=CARTESIAN_POINT('Ctrl Pts',(-0.109191717634944,-1.,-3.855485714969));
#53037=CARTESIAN_POINT('Ctrl Pts',(-0.109191717634944,1.,-3.855485714969));
#53038=CARTESIAN_POINT('Ctrl Pts',(-0.11110059303626,-1.,-3.86281867282965));
#53039=CARTESIAN_POINT('Ctrl Pts',(-0.11110059303626,1.,-3.86281867282965));
#53040=CARTESIAN_POINT('Ctrl Pts',(-0.113071304914562,-1.,-3.87013043445014));
#53041=CARTESIAN_POINT('Ctrl Pts',(-0.113071304914562,1.,-3.87013043445014));
#53042=CARTESIAN_POINT('Ctrl Pts',(-0.11510142664947,-1.,-3.87738168405343));
#53043=CARTESIAN_POINT('Ctrl Pts',(-0.11510142664947,1.,-3.87738168405343));
#53044=CARTESIAN_POINT('Ctrl Pts',(-0.117189150373144,-1.,-3.88456590045767));
#53045=CARTESIAN_POINT('Ctrl Pts',(-0.117189150373144,1.,-3.88456590045767));
#53046=CARTESIAN_POINT('Ctrl Pts',(-0.119333088190417,-1.,-3.89169600105201));
#53047=CARTESIAN_POINT('Ctrl Pts',(-0.119333088190417,1.,-3.89169600105201));
#53048=CARTESIAN_POINT('Ctrl Pts',(-0.121532144765723,-1.,-3.89879639336952));
#53049=CARTESIAN_POINT('Ctrl Pts',(-0.121532144765723,1.,-3.89879639336952));
#53050=CARTESIAN_POINT('Ctrl Pts',(-0.123785368272377,-1.,-3.90589336320508));
#53051=CARTESIAN_POINT('Ctrl Pts',(-0.123785368272377,1.,-3.90589336320508));
#53052=CARTESIAN_POINT('Ctrl Pts',(-0.126091793324137,-1.,-3.91300501605392));
#53053=CARTESIAN_POINT('Ctrl Pts',(-0.126091793324137,1.,-3.91300501605392));
#53054=CARTESIAN_POINT('Ctrl Pts',(-0.128450341339528,-1.,-3.92013513251642));
#53055=CARTESIAN_POINT('Ctrl Pts',(-0.128450341339528,1.,-3.92013513251642));
#53056=CARTESIAN_POINT('Ctrl Pts',(-0.130859892027799,-1.,-3.9272787679596));
#53057=CARTESIAN_POINT('Ctrl Pts',(-0.130859892027799,1.,-3.9272787679596));
#53058=CARTESIAN_POINT('Ctrl Pts',(-0.13331932279419,-1.,-3.93442567551035));
#53059=CARTESIAN_POINT('Ctrl Pts',(-0.13331932279419,1.,-3.93442567551035));
#53060=CARTESIAN_POINT('Ctrl Pts',(-0.135827558661188,-1.,-3.94156445130744));
#53061=CARTESIAN_POINT('Ctrl Pts',(-0.135827558661188,1.,-3.94156445130744));
#53062=CARTESIAN_POINT('Ctrl Pts',(-0.138383621255159,-1.,-3.94868667844355));
#53063=CARTESIAN_POINT('Ctrl Pts',(-0.138383621255159,1.,-3.94868667844355));
#53064=CARTESIAN_POINT('Ctrl Pts',(-0.140986665829937,-1.,-3.95579014116899));
#53065=CARTESIAN_POINT('Ctrl Pts',(-0.140986665829937,1.,-3.95579014116899));
#53066=CARTESIAN_POINT('Ctrl Pts',(-0.143635947692791,-1.,-3.96287658098896));
#53067=CARTESIAN_POINT('Ctrl Pts',(-0.143635947692791,1.,-3.96287658098896));
#53068=CARTESIAN_POINT('Ctrl Pts',(-0.146330797814513,-1.,-3.96995018565891));
#53069=CARTESIAN_POINT('Ctrl Pts',(-0.146330797814513,1.,-3.96995018565891));
#53070=CARTESIAN_POINT('Ctrl Pts',(-0.149070594803544,-1.,-3.97701581473643));
#53071=CARTESIAN_POINT('Ctrl Pts',(-0.149070594803544,1.,-3.97701581473643));
#53072=CARTESIAN_POINT('Ctrl Pts',(-0.151854737441405,-1.,-3.9840772985098));
#53073=CARTESIAN_POINT('Ctrl Pts',(-0.151854737441405,1.,-3.9840772985098));
#53074=CARTESIAN_POINT('Ctrl Pts',(-0.154682618338563,-1.,-3.99113582086059));
#53075=CARTESIAN_POINT('Ctrl Pts',(-0.154682618338563,1.,-3.99113582086059));
#53076=CARTESIAN_POINT('Ctrl Pts',(-0.15755363438381,-1.,-3.99819074631874));
#53077=CARTESIAN_POINT('Ctrl Pts',(-0.15755363438381,1.,-3.99819074631874));
#53078=CARTESIAN_POINT('Ctrl Pts',(-0.160467194882219,-1.,-4.00524031064509));
#53079=CARTESIAN_POINT('Ctrl Pts',(-0.160467194882219,1.,-4.00524031064509));
#53080=CARTESIAN_POINT('Ctrl Pts',(-0.163422730287459,-1.,-4.01228237022301));
#53081=CARTESIAN_POINT('Ctrl Pts',(-0.163422730287459,1.,-4.01228237022301));
#53082=CARTESIAN_POINT('Ctrl Pts',(-0.166419700015847,-1.,-4.01931510507143));
#53083=CARTESIAN_POINT('Ctrl Pts',(-0.166419700015847,1.,-4.01931510507143));
#53084=CARTESIAN_POINT('Ctrl Pts',(-0.169457601001653,-1.,-4.0263377970371));
#53085=CARTESIAN_POINT('Ctrl Pts',(-0.169457601001653,1.,-4.0263377970371));
#53086=CARTESIAN_POINT('Ctrl Pts',(-0.172535962484466,-1.,-4.03335057326093));
#53087=CARTESIAN_POINT('Ctrl Pts',(-0.172535962484466,1.,-4.03335057326093));
#53088=CARTESIAN_POINT('Ctrl Pts',(-0.175654339673757,-1.,-4.04035407891161));
#53089=CARTESIAN_POINT('Ctrl Pts',(-0.175654339673757,1.,-4.04035407891161));
#53090=CARTESIAN_POINT('Ctrl Pts',(-0.178812307240716,-1.,-4.04734916719722));
#53091=CARTESIAN_POINT('Ctrl Pts',(-0.178812307240716,1.,-4.04734916719722));
#53092=CARTESIAN_POINT('Ctrl Pts',(-0.18200945304855,-1.,-4.05433660358402));
#53093=CARTESIAN_POINT('Ctrl Pts',(-0.18200945304855,1.,-4.05433660358402));
#53094=CARTESIAN_POINT('Ctrl Pts',(-0.185245370038948,-1.,-4.06131670998589));
#53095=CARTESIAN_POINT('Ctrl Pts',(-0.185245370038948,1.,-4.06131670998589));
#53096=CARTESIAN_POINT('Ctrl Pts',(-0.188519658060255,-1.,-4.06828941192308));
#53097=CARTESIAN_POINT('Ctrl Pts',(-0.188519658060255,1.,-4.06828941192308));
#53098=CARTESIAN_POINT('Ctrl Pts',(-0.191831928181081,-1.,-4.07525439703137));
#53099=CARTESIAN_POINT('Ctrl Pts',(-0.191831928181081,1.,-4.07525439703137));
#53100=CARTESIAN_POINT('Ctrl Pts',(-0.195181806054714,-1.,-4.08221124060385));
#53101=CARTESIAN_POINT('Ctrl Pts',(-0.195181806054714,1.,-4.08221124060385));
#53102=CARTESIAN_POINT('Ctrl Pts',(-0.198568934800811,-1.,-4.08915953359753));
#53103=CARTESIAN_POINT('Ctrl Pts',(-0.198568934800811,1.,-4.08915953359753));
#53104=CARTESIAN_POINT('Ctrl Pts',(-0.201992979049984,-1.,-4.09609903751912));
#53105=CARTESIAN_POINT('Ctrl Pts',(-0.201992979049984,1.,-4.09609903751912));
#53106=CARTESIAN_POINT('Ctrl Pts',(-0.205453622198233,-1.,-4.10302969965374));
#53107=CARTESIAN_POINT('Ctrl Pts',(-0.205453622198233,1.,-4.10302969965374));
#53108=CARTESIAN_POINT('Ctrl Pts',(-0.208950559400172,-1.,-4.10995157639026));
#53109=CARTESIAN_POINT('Ctrl Pts',(-0.208950559400172,1.,-4.10995157639026));
#53110=CARTESIAN_POINT('Ctrl Pts',(-0.212483491087068,-1.,-4.11686478264545));
#53111=CARTESIAN_POINT('Ctrl Pts',(-0.212483491087068,1.,-4.11686478264545));
#53112=CARTESIAN_POINT('Ctrl Pts',(-0.216052116898425,-1.,-4.12376943492249));
#53113=CARTESIAN_POINT('Ctrl Pts',(-0.216052116898425,1.,-4.12376943492249));
#53114=CARTESIAN_POINT('Ctrl Pts',(-0.219656126701852,-1.,-4.13066558698156));
#53115=CARTESIAN_POINT('Ctrl Pts',(-0.219656126701852,1.,-4.13066558698156));
#53116=CARTESIAN_POINT('Ctrl Pts',(-0.223295201038383,-1.,-4.13755320553563));
#53117=CARTESIAN_POINT('Ctrl Pts',(-0.223295201038383,1.,-4.13755320553563));
#53118=CARTESIAN_POINT('Ctrl Pts',(-0.226969025061243,-1.,-4.14443220607733));
#53119=CARTESIAN_POINT('Ctrl Pts',(-0.226969025061243,1.,-4.14443220607733));
#53120=CARTESIAN_POINT('Ctrl Pts',(-0.230677299028738,-1.,-4.15130247435029));
#53121=CARTESIAN_POINT('Ctrl Pts',(-0.230677299028738,1.,-4.15130247435029));
#53122=CARTESIAN_POINT('Ctrl Pts',(-0.234419749543143,-1.,-4.1581638926525));
#53123=CARTESIAN_POINT('Ctrl Pts',(-0.234419749543143,1.,-4.1581638926525));
#53124=CARTESIAN_POINT('Ctrl Pts',(-0.238196140933977,-1.,-4.1650163665385));
#53125=CARTESIAN_POINT('Ctrl Pts',(-0.238196140933977,1.,-4.1650163665385));
#53126=CARTESIAN_POINT('Ctrl Pts',(-0.242006283923912,-1.,-4.17185984409533));
#53127=CARTESIAN_POINT('Ctrl Pts',(-0.242006283923912,1.,-4.17185984409533));
#53128=CARTESIAN_POINT('Ctrl Pts',(-0.245850033418583,-1.,-4.17869430192868));
#53129=CARTESIAN_POINT('Ctrl Pts',(-0.245850033418583,1.,-4.17869430192868));
#53130=CARTESIAN_POINT('Ctrl Pts',(-0.248951836910964,-1.,-4.18415464959491));
#53131=CARTESIAN_POINT('Ctrl Pts',(-0.248951836910964,1.,-4.18415464959491));
#53132=CARTESIAN_POINT('Ctrl Pts',(-0.251293239837693,-1.,-4.18824585244066));
#53133=CARTESIAN_POINT('Ctrl Pts',(-0.251293239837693,1.,-4.18824585244066));
#53134=CARTESIAN_POINT('Ctrl Pts',(-0.252860861572565,-1.,-4.19097151819241));
#53135=CARTESIAN_POINT('Ctrl Pts',(-0.252860861572565,1.,-4.19097151819241));
#53136=CARTESIAN_POINT('Ctrl Pts',(-0.253646344052521,-1.,-4.1923339003649));
#53137=CARTESIAN_POINT('Ctrl Pts',(-0.253646344052521,1.,-4.1923339003649));
#53138=CARTESIAN_POINT('',(-0.091259699916681,1.,-3.74888939116255));
#53139=CARTESIAN_POINT('Ctrl Pts',(-0.0912596999166824,-1.,-3.74888939116255));
#53140=CARTESIAN_POINT('Ctrl Pts',(-0.0912596999166824,-0.666666666666667,
-3.74888939116255));
#53141=CARTESIAN_POINT('Ctrl Pts',(-0.0912596999166824,-0.333333333333333,
-3.74888939116255));
#53142=CARTESIAN_POINT('Ctrl Pts',(-0.0912596999166824,0.333333333333333,
-3.74888939116255));
#53143=CARTESIAN_POINT('Ctrl Pts',(-0.0912596999166821,0.666666666666667,
-3.74888939116255));
#53144=CARTESIAN_POINT('Ctrl Pts',(-0.0912596999166821,1.,-3.74888939116255));
#53145=CARTESIAN_POINT('',(-0.253646344052521,1.,-4.1923339003649));
#53146=CARTESIAN_POINT('',(-0.253646344052521,0.,-4.1923339003649));
#53147=CARTESIAN_POINT('Ctrl Pts',(-0.0912596999166819,1.,-3.74888939116255));
#53148=CARTESIAN_POINT('Ctrl Pts',(-0.0912308016421982,1.,-3.74892890040975));
#53149=CARTESIAN_POINT('Ctrl Pts',(-0.0911666301812818,1.,-3.74911539914543));
#53150=CARTESIAN_POINT('Ctrl Pts',(-0.0911090736805512,1.,-3.74976844886347));
#53151=CARTESIAN_POINT('Ctrl Pts',(-0.0911323999574429,1.,-3.75145357872422));
#53152=CARTESIAN_POINT('Ctrl Pts',(-0.09134196227364,1.,-3.75495560118212));
#53153=CARTESIAN_POINT('Ctrl Pts',(-0.0917773084998337,1.,-3.76024199359303));
#53154=CARTESIAN_POINT('Ctrl Pts',(-0.0924090589602692,1.,-3.76678860031841));
#53155=CARTESIAN_POINT('Ctrl Pts',(-0.093218554620318,1.,-3.77424159971059));
#53156=CARTESIAN_POINT('Ctrl Pts',(-0.0941840095090815,1.,-3.782205218991));
#53157=CARTESIAN_POINT('Ctrl Pts',(-0.0952829885100802,1.,-3.79030016353111));
#53158=CARTESIAN_POINT('Ctrl Pts',(-0.0964949352873133,1.,-3.79822128513845));
#53159=CARTESIAN_POINT('Ctrl Pts',(-0.0978042222906645,1.,-3.80581088847809));
#53160=CARTESIAN_POINT('Ctrl Pts',(-0.0992008728096516,1.,-3.81306649386461));
#53161=CARTESIAN_POINT('Ctrl Pts',(-0.100678769650632,1.,-3.82007889742625));
#53162=CARTESIAN_POINT('Ctrl Pts',(-0.102234506488456,1.,-3.82698737143255));
#53163=CARTESIAN_POINT('Ctrl Pts',(-0.103866063811623,1.,-3.83393171228002));
#53164=CARTESIAN_POINT('Ctrl Pts',(-0.105571360916569,1.,-3.84099658324803));
#53165=CARTESIAN_POINT('Ctrl Pts',(-0.107347597812184,1.,-3.84819233070317));
#53166=CARTESIAN_POINT('Ctrl Pts',(-0.109191717634944,1.,-3.855485714969));
#53167=CARTESIAN_POINT('Ctrl Pts',(-0.11110059303626,1.,-3.86281867282965));
#53168=CARTESIAN_POINT('Ctrl Pts',(-0.113071304914562,1.,-3.87013043445014));
#53169=CARTESIAN_POINT('Ctrl Pts',(-0.11510142664947,1.,-3.87738168405343));
#53170=CARTESIAN_POINT('Ctrl Pts',(-0.117189150373144,1.,-3.88456590045767));
#53171=CARTESIAN_POINT('Ctrl Pts',(-0.119333088190417,1.,-3.89169600105201));
#53172=CARTESIAN_POINT('Ctrl Pts',(-0.121532144765723,1.,-3.89879639336952));
#53173=CARTESIAN_POINT('Ctrl Pts',(-0.123785368272377,1.,-3.90589336320508));
#53174=CARTESIAN_POINT('Ctrl Pts',(-0.126091793324137,1.,-3.91300501605392));
#53175=CARTESIAN_POINT('Ctrl Pts',(-0.128450341339528,1.,-3.92013513251642));
#53176=CARTESIAN_POINT('Ctrl Pts',(-0.130859892027799,1.,-3.9272787679596));
#53177=CARTESIAN_POINT('Ctrl Pts',(-0.13331932279419,1.,-3.93442567551035));
#53178=CARTESIAN_POINT('Ctrl Pts',(-0.135827558661188,1.,-3.94156445130744));
#53179=CARTESIAN_POINT('Ctrl Pts',(-0.138383621255159,1.,-3.94868667844355));
#53180=CARTESIAN_POINT('Ctrl Pts',(-0.140986665829937,1.,-3.95579014116899));
#53181=CARTESIAN_POINT('Ctrl Pts',(-0.143635947692791,1.,-3.96287658098896));
#53182=CARTESIAN_POINT('Ctrl Pts',(-0.146330797814513,1.,-3.96995018565891));
#53183=CARTESIAN_POINT('Ctrl Pts',(-0.149070594803544,1.,-3.97701581473643));
#53184=CARTESIAN_POINT('Ctrl Pts',(-0.151854737441405,1.,-3.9840772985098));
#53185=CARTESIAN_POINT('Ctrl Pts',(-0.154682618338563,1.,-3.99113582086059));
#53186=CARTESIAN_POINT('Ctrl Pts',(-0.15755363438381,1.,-3.99819074631874));
#53187=CARTESIAN_POINT('Ctrl Pts',(-0.160467194882219,1.,-4.00524031064509));
#53188=CARTESIAN_POINT('Ctrl Pts',(-0.163422730287459,1.,-4.01228237022301));
#53189=CARTESIAN_POINT('Ctrl Pts',(-0.166419700015847,1.,-4.01931510507143));
#53190=CARTESIAN_POINT('Ctrl Pts',(-0.169457601001653,1.,-4.0263377970371));
#53191=CARTESIAN_POINT('Ctrl Pts',(-0.172535962484466,1.,-4.03335057326093));
#53192=CARTESIAN_POINT('Ctrl Pts',(-0.175654339673757,1.,-4.04035407891161));
#53193=CARTESIAN_POINT('Ctrl Pts',(-0.178812307240716,1.,-4.04734916719722));
#53194=CARTESIAN_POINT('Ctrl Pts',(-0.18200945304855,1.,-4.05433660358402));
#53195=CARTESIAN_POINT('Ctrl Pts',(-0.185245370038948,1.,-4.06131670998589));
#53196=CARTESIAN_POINT('Ctrl Pts',(-0.188519658060255,1.,-4.06828941192308));
#53197=CARTESIAN_POINT('Ctrl Pts',(-0.191831928181081,1.,-4.07525439703137));
#53198=CARTESIAN_POINT('Ctrl Pts',(-0.195181806054714,1.,-4.08221124060385));
#53199=CARTESIAN_POINT('Ctrl Pts',(-0.198568934800811,1.,-4.08915953359753));
#53200=CARTESIAN_POINT('Ctrl Pts',(-0.201992979049984,1.,-4.09609903751912));
#53201=CARTESIAN_POINT('Ctrl Pts',(-0.205453622198233,1.,-4.10302969965374));
#53202=CARTESIAN_POINT('Ctrl Pts',(-0.208950559400172,1.,-4.10995157639026));
#53203=CARTESIAN_POINT('Ctrl Pts',(-0.212483491087068,1.,-4.11686478264545));
#53204=CARTESIAN_POINT('Ctrl Pts',(-0.216052116898425,1.,-4.12376943492249));
#53205=CARTESIAN_POINT('Ctrl Pts',(-0.219656126701852,1.,-4.13066558698156));
#53206=CARTESIAN_POINT('Ctrl Pts',(-0.223295201038383,1.,-4.13755320553563));
#53207=CARTESIAN_POINT('Ctrl Pts',(-0.226969025061243,1.,-4.14443220607733));
#53208=CARTESIAN_POINT('Ctrl Pts',(-0.230677299028738,1.,-4.15130247435029));
#53209=CARTESIAN_POINT('Ctrl Pts',(-0.234419749543143,1.,-4.1581638926525));
#53210=CARTESIAN_POINT('Ctrl Pts',(-0.238196140933977,1.,-4.1650163665385));
#53211=CARTESIAN_POINT('Ctrl Pts',(-0.242006283923912,1.,-4.17185984409533));
#53212=CARTESIAN_POINT('Ctrl Pts',(-0.245850033418583,1.,-4.17869430192868));
#53213=CARTESIAN_POINT('Ctrl Pts',(-0.248951836910964,1.,-4.18415464959491));
#53214=CARTESIAN_POINT('Ctrl Pts',(-0.251293239837693,1.,-4.18824585244066));
#53215=CARTESIAN_POINT('Ctrl Pts',(-0.252860861572565,1.,-4.19097151819241));
#53216=CARTESIAN_POINT('Ctrl Pts',(-0.253646344052521,1.,-4.1923339003649));
#53217=CARTESIAN_POINT('Origin',(-0.253646344052521,0.,-4.1923339003649));
#53218=CARTESIAN_POINT('',(-0.405301974318349,1.,-4.18039834341342));
#53219=CARTESIAN_POINT('Origin',(0.,0.,0.));
#53220=CARTESIAN_POINT('',(0.0912596999148849,1.,-3.74888939116259));
#53221=CARTESIAN_POINT('Origin',(0.,1.,0.));
#53222=CARTESIAN_POINT('Ctrl Pts',(0.0912596999148859,1.,-3.74888939116259));
#53223=CARTESIAN_POINT('Ctrl Pts',(0.0912596999148859,0.666666666666667,
-3.74888939116259));
#53224=CARTESIAN_POINT('Ctrl Pts',(0.091259699914886,0.333333333333333,
-3.74888939116259));
#53225=CARTESIAN_POINT('Ctrl Pts',(0.091259699914886,-0.333333333333333,
-3.74888939116259));
#53226=CARTESIAN_POINT('Ctrl Pts',(0.091259699914886,-0.666666666666667,
-3.74888939116259));
#53227=CARTESIAN_POINT('Ctrl Pts',(0.091259699914886,-1.,-3.74888939116259));
#53228=CARTESIAN_POINT('Ctrl Pts',(0.253646344052522,-1.,-4.1923339003649));
#53229=CARTESIAN_POINT('Ctrl Pts',(0.253646344052522,1.,-4.1923339003649));
#53230=CARTESIAN_POINT('Ctrl Pts',(0.25286086157284,-1.,-4.19097151819684));
#53231=CARTESIAN_POINT('Ctrl Pts',(0.25286086157284,1.,-4.19097151819684));
#53232=CARTESIAN_POINT('Ctrl Pts',(0.25129323983844,-1.,-4.18824585245272));
#53233=CARTESIAN_POINT('Ctrl Pts',(0.25129323983844,1.,-4.18824585245272));
#53234=CARTESIAN_POINT('Ctrl Pts',(0.248951836912189,-1.,-4.18415464961466));
#53235=CARTESIAN_POINT('Ctrl Pts',(0.248951836912189,1.,-4.18415464961466));
#53236=CARTESIAN_POINT('Ctrl Pts',(0.245850033420019,-1.,-4.1786943019518));
#53237=CARTESIAN_POINT('Ctrl Pts',(0.245850033420019,1.,-4.1786943019518));
#53238=CARTESIAN_POINT('Ctrl Pts',(0.242006283925088,-1.,-4.17185984411426));
#53239=CARTESIAN_POINT('Ctrl Pts',(0.242006283925088,1.,-4.17185984411426));
#53240=CARTESIAN_POINT('Ctrl Pts',(0.238196140934616,-1.,-4.16501636654877));
#53241=CARTESIAN_POINT('Ctrl Pts',(0.238196140934616,1.,-4.16501636654877));
#53242=CARTESIAN_POINT('Ctrl Pts',(0.234419749543207,-1.,-4.15816389265352));
#53243=CARTESIAN_POINT('Ctrl Pts',(0.234419749543207,1.,-4.15816389265352));
#53244=CARTESIAN_POINT('Ctrl Pts',(0.230677299028383,-1.,-4.15130247434459));
#53245=CARTESIAN_POINT('Ctrl Pts',(0.230677299028383,1.,-4.15130247434459));
#53246=CARTESIAN_POINT('Ctrl Pts',(0.226969025060705,-1.,-4.14443220606869));
#53247=CARTESIAN_POINT('Ctrl Pts',(0.226969025060705,1.,-4.14443220606869));
#53248=CARTESIAN_POINT('Ctrl Pts',(0.223295201037885,-1.,-4.13755320552764));
#53249=CARTESIAN_POINT('Ctrl Pts',(0.223295201037885,1.,-4.13755320552764));
#53250=CARTESIAN_POINT('Ctrl Pts',(0.219656126701541,-1.,-4.13066558697658));
#53251=CARTESIAN_POINT('Ctrl Pts',(0.219656126701541,1.,-4.13066558697658));
#53252=CARTESIAN_POINT('Ctrl Pts',(0.216052116898351,-1.,-4.12376943492132));
#53253=CARTESIAN_POINT('Ctrl Pts',(0.216052116898351,1.,-4.12376943492132));
#53254=CARTESIAN_POINT('Ctrl Pts',(0.212483491087189,-1.,-4.11686478264739));
#53255=CARTESIAN_POINT('Ctrl Pts',(0.212483491087189,1.,-4.11686478264739));
#53256=CARTESIAN_POINT('Ctrl Pts',(0.208950559400392,-1.,-4.10995157639377));
#53257=CARTESIAN_POINT('Ctrl Pts',(0.208950559400392,1.,-4.10995157639377));
#53258=CARTESIAN_POINT('Ctrl Pts',(0.205453622198454,-1.,-4.10302969965728));
#53259=CARTESIAN_POINT('Ctrl Pts',(0.205453622198454,1.,-4.10302969965728));
#53260=CARTESIAN_POINT('Ctrl Pts',(0.201992979050135,-1.,-4.09609903752152));
#53261=CARTESIAN_POINT('Ctrl Pts',(0.201992979050135,1.,-4.09609903752152));
#53262=CARTESIAN_POINT('Ctrl Pts',(0.198568934800861,-1.,-4.08915953359833));
#53263=CARTESIAN_POINT('Ctrl Pts',(0.198568934800861,1.,-4.08915953359833));
#53264=CARTESIAN_POINT('Ctrl Pts',(0.195181806054675,-1.,-4.08221124060322));
#53265=CARTESIAN_POINT('Ctrl Pts',(0.195181806054675,1.,-4.08221124060322));
#53266=CARTESIAN_POINT('Ctrl Pts',(0.19183192818099,-1.,-4.07525439702992));
#53267=CARTESIAN_POINT('Ctrl Pts',(0.19183192818099,1.,-4.07525439702992));
#53268=CARTESIAN_POINT('Ctrl Pts',(0.188519658060155,-1.,-4.06828941192147));
#53269=CARTESIAN_POINT('Ctrl Pts',(0.188519658060155,1.,-4.06828941192147));
#53270=CARTESIAN_POINT('Ctrl Pts',(0.185245370038873,-1.,-4.06131670998469));
#53271=CARTESIAN_POINT('Ctrl Pts',(0.185245370038873,1.,-4.06131670998469));
#53272=CARTESIAN_POINT('Ctrl Pts',(0.182009453048519,-1.,-4.05433660358353));
#53273=CARTESIAN_POINT('Ctrl Pts',(0.182009453048519,1.,-4.05433660358353));
#53274=CARTESIAN_POINT('Ctrl Pts',(0.178812307240728,-1.,-4.04734916719741));
#53275=CARTESIAN_POINT('Ctrl Pts',(0.178812307240728,1.,-4.04734916719741));
#53276=CARTESIAN_POINT('Ctrl Pts',(0.175654339673797,-1.,-4.04035407891222));
#53277=CARTESIAN_POINT('Ctrl Pts',(0.175654339673797,1.,-4.04035407891222));
#53278=CARTESIAN_POINT('Ctrl Pts',(0.172535962484514,-1.,-4.03335057326163));
#53279=CARTESIAN_POINT('Ctrl Pts',(0.172535962484514,1.,-4.03335057326163));
#53280=CARTESIAN_POINT('Ctrl Pts',(0.169457601001691,-1.,-4.02633779703764));
#53281=CARTESIAN_POINT('Ctrl Pts',(0.169457601001691,1.,-4.02633779703764));
#53282=CARTESIAN_POINT('Ctrl Pts',(0.166419700015865,-1.,-4.01931510507167));
#53283=CARTESIAN_POINT('Ctrl Pts',(0.166419700015865,1.,-4.01931510507167));
#53284=CARTESIAN_POINT('Ctrl Pts',(0.163422730287456,-1.,-4.01228237022296));
#53285=CARTESIAN_POINT('Ctrl Pts',(0.163422730287456,1.,-4.01228237022296));
#53286=CARTESIAN_POINT('Ctrl Pts',(0.160467194882202,-1.,-4.00524031064487));
#53287=CARTESIAN_POINT('Ctrl Pts',(0.160467194882202,1.,-4.00524031064487));
#53288=CARTESIAN_POINT('Ctrl Pts',(0.15755363438379,-1.,-3.9981907463185));
#53289=CARTESIAN_POINT('Ctrl Pts',(0.15755363438379,1.,-3.9981907463185));
#53290=CARTESIAN_POINT('Ctrl Pts',(0.154682618338547,-1.,-3.99113582086043));
#53291=CARTESIAN_POINT('Ctrl Pts',(0.154682618338547,1.,-3.99113582086043));
#53292=CARTESIAN_POINT('Ctrl Pts',(0.151854737441398,-1.,-3.98407729850975));
#53293=CARTESIAN_POINT('Ctrl Pts',(0.151854737441398,1.,-3.98407729850975));
#53294=CARTESIAN_POINT('Ctrl Pts',(0.149070594803544,-1.,-3.97701581473644));
#53295=CARTESIAN_POINT('Ctrl Pts',(0.149070594803544,1.,-3.97701581473644));
#53296=CARTESIAN_POINT('Ctrl Pts',(0.14633079781452,-1.,-3.96995018565893));
#53297=CARTESIAN_POINT('Ctrl Pts',(0.14633079781452,1.,-3.96995018565893));
#53298=CARTESIAN_POINT('Ctrl Pts',(0.143635947692798,-1.,-3.96287658098896));
#53299=CARTESIAN_POINT('Ctrl Pts',(0.143635947692798,1.,-3.96287658098896));
#53300=CARTESIAN_POINT('Ctrl Pts',(0.140986665829942,-1.,-3.95579014116894));
#53301=CARTESIAN_POINT('Ctrl Pts',(0.140986665829942,1.,-3.95579014116894));
#53302=CARTESIAN_POINT('Ctrl Pts',(0.138383621255161,-1.,-3.94868667844347));
#53303=CARTESIAN_POINT('Ctrl Pts',(0.138383621255161,1.,-3.94868667844347));
#53304=CARTESIAN_POINT('Ctrl Pts',(0.135827558661188,-1.,-3.94156445130741));
#53305=CARTESIAN_POINT('Ctrl Pts',(0.135827558661188,1.,-3.94156445130741));
#53306=CARTESIAN_POINT('Ctrl Pts',(0.13331932279419,-1.,-3.93442567551042));
#53307=CARTESIAN_POINT('Ctrl Pts',(0.13331932279419,1.,-3.93442567551042));
#53308=CARTESIAN_POINT('Ctrl Pts',(0.130859892027801,-1.,-3.92727876795977));
#53309=CARTESIAN_POINT('Ctrl Pts',(0.130859892027801,1.,-3.92727876795977));
#53310=CARTESIAN_POINT('Ctrl Pts',(0.128450341339532,-1.,-3.92013513251664));
#53311=CARTESIAN_POINT('Ctrl Pts',(0.128450341339532,1.,-3.92013513251664));
#53312=CARTESIAN_POINT('Ctrl Pts',(0.126091793324141,-1.,-3.91300501605411));
#53313=CARTESIAN_POINT('Ctrl Pts',(0.126091793324141,1.,-3.91300501605411));
#53314=CARTESIAN_POINT('Ctrl Pts',(0.123785368272379,-1.,-3.90589336320515));
#53315=CARTESIAN_POINT('Ctrl Pts',(0.123785368272379,1.,-3.90589336320515));
#53316=CARTESIAN_POINT('Ctrl Pts',(0.121532144765721,-1.,-3.89879639336939));
#53317=CARTESIAN_POINT('Ctrl Pts',(0.121532144765721,1.,-3.89879639336939));
#53318=CARTESIAN_POINT('Ctrl Pts',(0.11933308819041,-1.,-3.8916960010517));
#53319=CARTESIAN_POINT('Ctrl Pts',(0.11933308819041,1.,-3.8916960010517));
#53320=CARTESIAN_POINT('Ctrl Pts',(0.117189150373134,-1.,-3.88456590045726));
#53321=CARTESIAN_POINT('Ctrl Pts',(0.117189150373134,1.,-3.88456590045726));
#53322=CARTESIAN_POINT('Ctrl Pts',(0.11510142664946,-1.,-3.87738168405308));
#53323=CARTESIAN_POINT('Ctrl Pts',(0.11510142664946,1.,-3.87738168405308));
#53324=CARTESIAN_POINT('Ctrl Pts',(0.113071304914558,-1.,-3.87013043445001));
#53325=CARTESIAN_POINT('Ctrl Pts',(0.113071304914558,1.,-3.87013043445001));
#53326=CARTESIAN_POINT('Ctrl Pts',(0.111100593036266,-1.,-3.86281867282984));
#53327=CARTESIAN_POINT('Ctrl Pts',(0.111100593036266,1.,-3.86281867282984));
#53328=CARTESIAN_POINT('Ctrl Pts',(0.10919171763496,-1.,-3.85548571496953));
#53329=CARTESIAN_POINT('Ctrl Pts',(0.10919171763496,1.,-3.85548571496953));
#53330=CARTESIAN_POINT('Ctrl Pts',(0.107347597812208,-1.,-3.84819233070391));
#53331=CARTESIAN_POINT('Ctrl Pts',(0.107347597812208,1.,-3.84819233070391));
#53332=CARTESIAN_POINT('Ctrl Pts',(0.105571360916593,-1.,-3.84099658324873));
#53333=CARTESIAN_POINT('Ctrl Pts',(0.105571360916593,1.,-3.84099658324873));
#53334=CARTESIAN_POINT('Ctrl Pts',(0.103866063811634,-1.,-3.83393171228034));
#53335=CARTESIAN_POINT('Ctrl Pts',(0.103866063811634,1.,-3.83393171228034));
#53336=CARTESIAN_POINT('Ctrl Pts',(0.102234506488445,-1.,-3.8269873714322));
#53337=CARTESIAN_POINT('Ctrl Pts',(0.102234506488445,1.,-3.8269873714322));
#53338=CARTESIAN_POINT('Ctrl Pts',(0.100678769650594,-1.,-3.82007889742512));
#53339=CARTESIAN_POINT('Ctrl Pts',(0.100678769650594,1.,-3.82007889742512));
#53340=CARTESIAN_POINT('Ctrl Pts',(0.099200872809594,-1.,-3.81306649386293));
#53341=CARTESIAN_POINT('Ctrl Pts',(0.099200872809594,1.,-3.81306649386293));
#53342=CARTESIAN_POINT('Ctrl Pts',(0.0978042222906071,-1.,-3.80581088847642));
#53343=CARTESIAN_POINT('Ctrl Pts',(0.0978042222906071,1.,-3.80581088847642));
#53344=CARTESIAN_POINT('Ctrl Pts',(0.0964949352872842,-1.,-3.7982212851376));
#53345=CARTESIAN_POINT('Ctrl Pts',(0.0964949352872842,1.,-3.7982212851376));
#53346=CARTESIAN_POINT('Ctrl Pts',(0.0952829885101065,-1.,-3.79030016353186));
#53347=CARTESIAN_POINT('Ctrl Pts',(0.0952829885101065,1.,-3.79030016353186));
#53348=CARTESIAN_POINT('Ctrl Pts',(0.094184009509174,-1.,-3.78220521899366));
#53349=CARTESIAN_POINT('Ctrl Pts',(0.094184009509174,1.,-3.78220521899366));
#53350=CARTESIAN_POINT('Ctrl Pts',(0.0932185546204571,-1.,-3.77424159971456));
#53351=CARTESIAN_POINT('Ctrl Pts',(0.0932185546204571,1.,-3.77424159971456));
#53352=CARTESIAN_POINT('Ctrl Pts',(0.0924090589604052,-1.,-3.76678860032228));
#53353=CARTESIAN_POINT('Ctrl Pts',(0.0924090589604052,1.,-3.76678860032228));
#53354=CARTESIAN_POINT('Ctrl Pts',(0.0917773084999005,-1.,-3.76024199359493));
#53355=CARTESIAN_POINT('Ctrl Pts',(0.0917773084999005,1.,-3.76024199359493));
#53356=CARTESIAN_POINT('Ctrl Pts',(0.0913419622735849,-1.,-3.75495560118053));
#53357=CARTESIAN_POINT('Ctrl Pts',(0.0913419622735849,1.,-3.75495560118053));
#53358=CARTESIAN_POINT('Ctrl Pts',(0.0911154000996403,-1.,-3.75116949194125));
#53359=CARTESIAN_POINT('Ctrl Pts',(0.0911154000996403,1.,-3.75116949194125));
#53360=CARTESIAN_POINT('Ctrl Pts',(0.0911057547504657,-1.,-3.74943097853257));
#53361=CARTESIAN_POINT('Ctrl Pts',(0.0911057547504657,1.,-3.74943097853257));
#53362=CARTESIAN_POINT('Ctrl Pts',(0.0911958743733922,-1.,-3.7488701717383));
#53363=CARTESIAN_POINT('Ctrl Pts',(0.0911958743733922,1.,-3.7488701717383));
#53364=CARTESIAN_POINT('Ctrl Pts',(0.0912992005792088,-1.,-3.74882632118923));
#53365=CARTESIAN_POINT('Ctrl Pts',(0.0912992005792088,1.,-3.74882632118923));
#53366=CARTESIAN_POINT('Ctrl Pts',(0.0913616755937425,-1.,-3.74888690736767));
#53367=CARTESIAN_POINT('Ctrl Pts',(0.0913616755937425,1.,-3.74888690736767));
#53368=CARTESIAN_POINT('',(0.253646344052522,1.,-4.1923339003649));
#53369=CARTESIAN_POINT('Ctrl Pts',(0.253646344052522,1.,-4.1923339003649));
#53370=CARTESIAN_POINT('Ctrl Pts',(0.25286086157284,1.,-4.19097151819684));
#53371=CARTESIAN_POINT('Ctrl Pts',(0.25129323983844,1.,-4.18824585245272));
#53372=CARTESIAN_POINT('Ctrl Pts',(0.248951836912189,1.,-4.18415464961466));
#53373=CARTESIAN_POINT('Ctrl Pts',(0.245850033420019,1.,-4.1786943019518));
#53374=CARTESIAN_POINT('Ctrl Pts',(0.242006283925088,1.,-4.17185984411426));
#53375=CARTESIAN_POINT('Ctrl Pts',(0.238196140934616,1.,-4.16501636654877));
#53376=CARTESIAN_POINT('Ctrl Pts',(0.234419749543207,1.,-4.15816389265352));
#53377=CARTESIAN_POINT('Ctrl Pts',(0.230677299028383,1.,-4.15130247434459));
#53378=CARTESIAN_POINT('Ctrl Pts',(0.226969025060705,1.,-4.14443220606869));
#53379=CARTESIAN_POINT('Ctrl Pts',(0.223295201037885,1.,-4.13755320552764));
#53380=CARTESIAN_POINT('Ctrl Pts',(0.219656126701541,1.,-4.13066558697658));
#53381=CARTESIAN_POINT('Ctrl Pts',(0.216052116898351,1.,-4.12376943492132));
#53382=CARTESIAN_POINT('Ctrl Pts',(0.212483491087189,1.,-4.11686478264739));
#53383=CARTESIAN_POINT('Ctrl Pts',(0.208950559400392,1.,-4.10995157639377));
#53384=CARTESIAN_POINT('Ctrl Pts',(0.205453622198454,1.,-4.10302969965728));
#53385=CARTESIAN_POINT('Ctrl Pts',(0.201992979050135,1.,-4.09609903752152));
#53386=CARTESIAN_POINT('Ctrl Pts',(0.198568934800861,1.,-4.08915953359833));
#53387=CARTESIAN_POINT('Ctrl Pts',(0.195181806054675,1.,-4.08221124060322));
#53388=CARTESIAN_POINT('Ctrl Pts',(0.19183192818099,1.,-4.07525439702992));
#53389=CARTESIAN_POINT('Ctrl Pts',(0.188519658060155,1.,-4.06828941192147));
#53390=CARTESIAN_POINT('Ctrl Pts',(0.185245370038873,1.,-4.06131670998469));
#53391=CARTESIAN_POINT('Ctrl Pts',(0.182009453048519,1.,-4.05433660358353));
#53392=CARTESIAN_POINT('Ctrl Pts',(0.178812307240728,1.,-4.04734916719741));
#53393=CARTESIAN_POINT('Ctrl Pts',(0.175654339673797,1.,-4.04035407891222));
#53394=CARTESIAN_POINT('Ctrl Pts',(0.172535962484514,1.,-4.03335057326163));
#53395=CARTESIAN_POINT('Ctrl Pts',(0.169457601001691,1.,-4.02633779703764));
#53396=CARTESIAN_POINT('Ctrl Pts',(0.166419700015865,1.,-4.01931510507167));
#53397=CARTESIAN_POINT('Ctrl Pts',(0.163422730287456,1.,-4.01228237022296));
#53398=CARTESIAN_POINT('Ctrl Pts',(0.160467194882202,1.,-4.00524031064487));
#53399=CARTESIAN_POINT('Ctrl Pts',(0.15755363438379,1.,-3.9981907463185));
#53400=CARTESIAN_POINT('Ctrl Pts',(0.154682618338547,1.,-3.99113582086043));
#53401=CARTESIAN_POINT('Ctrl Pts',(0.151854737441398,1.,-3.98407729850975));
#53402=CARTESIAN_POINT('Ctrl Pts',(0.149070594803544,1.,-3.97701581473644));
#53403=CARTESIAN_POINT('Ctrl Pts',(0.14633079781452,1.,-3.96995018565893));
#53404=CARTESIAN_POINT('Ctrl Pts',(0.143635947692798,1.,-3.96287658098896));
#53405=CARTESIAN_POINT('Ctrl Pts',(0.140986665829942,1.,-3.95579014116894));
#53406=CARTESIAN_POINT('Ctrl Pts',(0.138383621255161,1.,-3.94868667844347));
#53407=CARTESIAN_POINT('Ctrl Pts',(0.135827558661188,1.,-3.94156445130741));
#53408=CARTESIAN_POINT('Ctrl Pts',(0.13331932279419,1.,-3.93442567551042));
#53409=CARTESIAN_POINT('Ctrl Pts',(0.130859892027801,1.,-3.92727876795977));
#53410=CARTESIAN_POINT('Ctrl Pts',(0.128450341339532,1.,-3.92013513251664));
#53411=CARTESIAN_POINT('Ctrl Pts',(0.126091793324141,1.,-3.91300501605411));
#53412=CARTESIAN_POINT('Ctrl Pts',(0.123785368272379,1.,-3.90589336320515));
#53413=CARTESIAN_POINT('Ctrl Pts',(0.121532144765721,1.,-3.89879639336939));
#53414=CARTESIAN_POINT('Ctrl Pts',(0.11933308819041,1.,-3.8916960010517));
#53415=CARTESIAN_POINT('Ctrl Pts',(0.117189150373134,1.,-3.88456590045726));
#53416=CARTESIAN_POINT('Ctrl Pts',(0.11510142664946,1.,-3.87738168405308));
#53417=CARTESIAN_POINT('Ctrl Pts',(0.113071304914558,1.,-3.87013043445001));
#53418=CARTESIAN_POINT('Ctrl Pts',(0.111100593036266,1.,-3.86281867282984));
#53419=CARTESIAN_POINT('Ctrl Pts',(0.10919171763496,1.,-3.85548571496953));
#53420=CARTESIAN_POINT('Ctrl Pts',(0.107347597812208,1.,-3.84819233070391));
#53421=CARTESIAN_POINT('Ctrl Pts',(0.105571360916593,1.,-3.84099658324873));
#53422=CARTESIAN_POINT('Ctrl Pts',(0.103866063811634,1.,-3.83393171228034));
#53423=CARTESIAN_POINT('Ctrl Pts',(0.102234506488445,1.,-3.8269873714322));
#53424=CARTESIAN_POINT('Ctrl Pts',(0.100678769650594,1.,-3.82007889742512));
#53425=CARTESIAN_POINT('Ctrl Pts',(0.099200872809594,1.,-3.81306649386293));
#53426=CARTESIAN_POINT('Ctrl Pts',(0.0978042222906071,1.,-3.80581088847642));
#53427=CARTESIAN_POINT('Ctrl Pts',(0.0964949352872842,1.,-3.7982212851376));
#53428=CARTESIAN_POINT('Ctrl Pts',(0.0952829885101065,1.,-3.79030016353186));
#53429=CARTESIAN_POINT('Ctrl Pts',(0.094184009509174,1.,-3.78220521899366));
#53430=CARTESIAN_POINT('Ctrl Pts',(0.0932185546204571,1.,-3.77424159971456));
#53431=CARTESIAN_POINT('Ctrl Pts',(0.0924090589604052,1.,-3.76678860032228));
#53432=CARTESIAN_POINT('Ctrl Pts',(0.0917773084999005,1.,-3.76024199359493));
#53433=CARTESIAN_POINT('Ctrl Pts',(0.0913419622735849,1.,-3.75495560118053));
#53434=CARTESIAN_POINT('Ctrl Pts',(0.0911323999576141,1.,-3.75145357872511));
#53435=CARTESIAN_POINT('Ctrl Pts',(0.0911090736804567,1.,-3.74976844886495));
#53436=CARTESIAN_POINT('Ctrl Pts',(0.0911666301806421,1.,-3.74911539914664));
#53437=CARTESIAN_POINT('Ctrl Pts',(0.0912308016409228,1.,-3.74892890041021));
#53438=CARTESIAN_POINT('Ctrl Pts',(0.0912596999148853,1.,-3.74888939116259));
#53439=CARTESIAN_POINT('',(0.253646344052522,0.,-4.1923339003649));
#53440=CARTESIAN_POINT('Ctrl Pts',(0.496218256089212,-1.,-3.71702400346349));
#53441=CARTESIAN_POINT('Ctrl Pts',(0.496218256089212,1.,-3.71702400346349));
#53442=CARTESIAN_POINT('Ctrl Pts',(0.496270484166408,-1.,-3.7169543899574));
#53443=CARTESIAN_POINT('Ctrl Pts',(0.496270484166408,1.,-3.7169543899574));
#53444=CARTESIAN_POINT('Ctrl Pts',(0.496379397992639,-1.,-3.71698153685602));
#53445=CARTESIAN_POINT('Ctrl Pts',(0.496379397992639,1.,-3.71698153685602));
#53446=CARTESIAN_POINT('Ctrl Pts',(0.496556137604532,-1.,-3.71752134137482));
#53447=CARTESIAN_POINT('Ctrl Pts',(0.496556137604532,1.,-3.71752134137482));
#53448=CARTESIAN_POINT('Ctrl Pts',(0.496818574420595,-1.,-3.71923995966302));
#53449=CARTESIAN_POINT('Ctrl Pts',(0.496818574420595,1.,-3.71923995966302));
#53450=CARTESIAN_POINT('Ctrl Pts',(0.497187079575988,-1.,-3.72301489774398));
#53451=CARTESIAN_POINT('Ctrl Pts',(0.497187079575988,1.,-3.72301489774398));
#53452=CARTESIAN_POINT('Ctrl Pts',(0.497584067153049,-1.,-3.72830430904606));
#53453=CARTESIAN_POINT('Ctrl Pts',(0.497584067153049,1.,-3.72830430904606));
#53454=CARTESIAN_POINT('Ctrl Pts',(0.497984209510024,-1.,-3.73486914372449));
#53455=CARTESIAN_POINT('Ctrl Pts',(0.497984209510024,1.,-3.73486914372449));
#53456=CARTESIAN_POINT('Ctrl Pts',(0.498350586057692,-1.,-3.74235701734714));
#53457=CARTESIAN_POINT('Ctrl Pts',(0.498350586057692,1.,-3.74235701734714));
#53458=CARTESIAN_POINT('Ctrl Pts',(0.498642802042605,-1.,-3.75037362167839));
#53459=CARTESIAN_POINT('Ctrl Pts',(0.498642802042605,1.,-3.75037362167839));
#53460=CARTESIAN_POINT('Ctrl Pts',(0.498823681615421,-1.,-3.75854082221052));
#53461=CARTESIAN_POINT('Ctrl Pts',(0.498823681615421,1.,-3.75854082221052));
#53462=CARTESIAN_POINT('Ctrl Pts',(0.49886579233529,-1.,-3.76655401191229));
#53463=CARTESIAN_POINT('Ctrl Pts',(0.49886579233529,1.,-3.76655401191229));
#53464=CARTESIAN_POINT('Ctrl Pts',(0.498759900365891,-1.,-3.77425499225255));
#53465=CARTESIAN_POINT('Ctrl Pts',(0.498759900365891,1.,-3.77425499225255));
#53466=CARTESIAN_POINT('Ctrl Pts',(0.498515471679584,-1.,-3.78163975337356));
#53467=CARTESIAN_POINT('Ctrl Pts',(0.498515471679584,1.,-3.78163975337356));
#53468=CARTESIAN_POINT('Ctrl Pts',(0.498152751800958,-1.,-3.78879701661264));
#53469=CARTESIAN_POINT('Ctrl Pts',(0.498152751800958,1.,-3.78879701661264));
#53470=CARTESIAN_POINT('Ctrl Pts',(0.497696892100624,-1.,-3.79586380669994));
#53471=CARTESIAN_POINT('Ctrl Pts',(0.497696892100624,1.,-3.79586380669994));
#53472=CARTESIAN_POINT('Ctrl Pts',(0.497171756201051,-1.,-3.80297788298514));
#53473=CARTESIAN_POINT('Ctrl Pts',(0.497171756201051,1.,-3.80297788298514));
#53474=CARTESIAN_POINT('Ctrl Pts',(0.496592643443704,-1.,-3.81022254090839));
#53475=CARTESIAN_POINT('Ctrl Pts',(0.496592643443704,1.,-3.81022254090839));
#53476=CARTESIAN_POINT('Ctrl Pts',(0.495963937875479,-1.,-3.81760756144025));
#53477=CARTESIAN_POINT('Ctrl Pts',(0.495963937875479,1.,-3.81760756144025));
#53478=CARTESIAN_POINT('Ctrl Pts',(0.495283458893837,-1.,-3.82509963594103));
#53479=CARTESIAN_POINT('Ctrl Pts',(0.495283458893837,1.,-3.82509963594103));
#53480=CARTESIAN_POINT('Ctrl Pts',(0.494545212256401,-1.,-3.83264092682431));
#53481=CARTESIAN_POINT('Ctrl Pts',(0.494545212256401,1.,-3.83264092682431));
#53482=CARTESIAN_POINT('Ctrl Pts',(0.493742574629134,-1.,-3.84017095578451));
#53483=CARTESIAN_POINT('Ctrl Pts',(0.493742574629134,1.,-3.84017095578451));
#53484=CARTESIAN_POINT('Ctrl Pts',(0.49287179241414,-1.,-3.84765051147999));
#53485=CARTESIAN_POINT('Ctrl Pts',(0.49287179241414,1.,-3.84765051147999));
#53486=CARTESIAN_POINT('Ctrl Pts',(0.491933631083813,-1.,-3.85507287020263));
#53487=CARTESIAN_POINT('Ctrl Pts',(0.491933631083813,1.,-3.85507287020263));
#53488=CARTESIAN_POINT('Ctrl Pts',(0.490931482170891,-1.,-3.86245057319246));
#53489=CARTESIAN_POINT('Ctrl Pts',(0.490931482170891,1.,-3.86245057319246));
#53490=CARTESIAN_POINT('Ctrl Pts',(0.489870245704917,-1.,-3.86980755613707));
#53491=CARTESIAN_POINT('Ctrl Pts',(0.489870245704917,1.,-3.86980755613707));
#53492=CARTESIAN_POINT('Ctrl Pts',(0.488754973798273,-1.,-3.87716963231109));
#53493=CARTESIAN_POINT('Ctrl Pts',(0.488754973798273,1.,-3.87716963231109));
#53494=CARTESIAN_POINT('Ctrl Pts',(0.487589452275154,-1.,-3.88455453328138));
#53495=CARTESIAN_POINT('Ctrl Pts',(0.487589452275154,1.,-3.88455453328138));
#53496=CARTESIAN_POINT('Ctrl Pts',(0.486375337854103,-1.,-3.89196582437552));
#53497=CARTESIAN_POINT('Ctrl Pts',(0.486375337854103,1.,-3.89196582437552));
#53498=CARTESIAN_POINT('Ctrl Pts',(0.485112963522222,-1.,-3.89939844658513));
#53499=CARTESIAN_POINT('Ctrl Pts',(0.485112963522222,1.,-3.89939844658513));
#53500=CARTESIAN_POINT('Ctrl Pts',(0.48380183508915,-1.,-3.90684210358056));
#53501=CARTESIAN_POINT('Ctrl Pts',(0.48380183508915,1.,-3.90684210358056));
#53502=CARTESIAN_POINT('Ctrl Pts',(0.482441230340713,-1.,-3.91428536373751));
#53503=CARTESIAN_POINT('Ctrl Pts',(0.482441230340713,1.,-3.91428536373751));
#53504=CARTESIAN_POINT('Ctrl Pts',(0.481030798910748,-1.,-3.92171976072341));
#53505=CARTESIAN_POINT('Ctrl Pts',(0.481030798910748,1.,-3.92171976072341));
#53506=CARTESIAN_POINT('Ctrl Pts',(0.479571028525578,-1.,-3.92914297392071));
#53507=CARTESIAN_POINT('Ctrl Pts',(0.479571028525578,1.,-3.92914297392071));
#53508=CARTESIAN_POINT('Ctrl Pts',(0.478062927140964,-1.,-3.93655660689819));
#53509=CARTESIAN_POINT('Ctrl Pts',(0.478062927140964,1.,-3.93655660689819));
#53510=CARTESIAN_POINT('Ctrl Pts',(0.476507810658537,-1.,-3.94396469119383));
#53511=CARTESIAN_POINT('Ctrl Pts',(0.476507810658537,1.,-3.94396469119383));
#53512=CARTESIAN_POINT('Ctrl Pts',(0.47490705302179,-1.,-3.95137192932897));
#53513=CARTESIAN_POINT('Ctrl Pts',(0.47490705302179,1.,-3.95137192932897));
#53514=CARTESIAN_POINT('Ctrl Pts',(0.473261847236297,-1.,-3.95878201038338));
#53515=CARTESIAN_POINT('Ctrl Pts',(0.473261847236297,1.,-3.95878201038338));
#53516=CARTESIAN_POINT('Ctrl Pts',(0.471572978413503,-1.,-3.96619600864643));
#53517=CARTESIAN_POINT('Ctrl Pts',(0.471572978413503,1.,-3.96619600864643));
#53518=CARTESIAN_POINT('Ctrl Pts',(0.469840942829895,-1.,-3.97361320212436));
#53519=CARTESIAN_POINT('Ctrl Pts',(0.469840942829895,1.,-3.97361320212436));
#53520=CARTESIAN_POINT('Ctrl Pts',(0.468066047920157,-1.,-3.98103175589371));
#53521=CARTESIAN_POINT('Ctrl Pts',(0.468066047920157,1.,-3.98103175589371));
#53522=CARTESIAN_POINT('Ctrl Pts',(0.466248520883039,-1.,-3.98844946363262));
#53523=CARTESIAN_POINT('Ctrl Pts',(0.466248520883039,1.,-3.98844946363262));
#53524=CARTESIAN_POINT('Ctrl Pts',(0.464388610938975,-1.,-3.9958644432011));
#53525=CARTESIAN_POINT('Ctrl Pts',(0.464388610938975,1.,-3.9958644432011));
#53526=CARTESIAN_POINT('Ctrl Pts',(0.462486702616204,-1.,-4.00327590659075));
#53527=CARTESIAN_POINT('Ctrl Pts',(0.462486702616204,1.,-4.00327590659075));
#53528=CARTESIAN_POINT('Ctrl Pts',(0.460543280768514,-1.,-4.01068390573399));
#53529=CARTESIAN_POINT('Ctrl Pts',(0.460543280768514,1.,-4.01068390573399));
#53530=CARTESIAN_POINT('Ctrl Pts',(0.458558885636945,-1.,-4.01808900827587));
#53531=CARTESIAN_POINT('Ctrl Pts',(0.458558885636945,1.,-4.01808900827587));
#53532=CARTESIAN_POINT('Ctrl Pts',(0.45653407078495,-1.,-4.02549199038394));
#53533=CARTESIAN_POINT('Ctrl Pts',(0.45653407078495,1.,-4.02549199038394));
#53534=CARTESIAN_POINT('Ctrl Pts',(0.454469363020541,-1.,-4.03289354362794));
#53535=CARTESIAN_POINT('Ctrl Pts',(0.454469363020541,1.,-4.03289354362794));
#53536=CARTESIAN_POINT('Ctrl Pts',(0.452365214748892,-1.,-4.04029392228049));
#53537=CARTESIAN_POINT('Ctrl Pts',(0.452365214748892,1.,-4.04029392228049));
#53538=CARTESIAN_POINT('Ctrl Pts',(0.450222009543926,-1.,-4.0476929901813));
#53539=CARTESIAN_POINT('Ctrl Pts',(0.450222009543926,1.,-4.0476929901813));
#53540=CARTESIAN_POINT('Ctrl Pts',(0.448040082684114,-1.,-4.0550903779696));
#53541=CARTESIAN_POINT('Ctrl Pts',(0.448040082684114,1.,-4.0550903779696));
#53542=CARTESIAN_POINT('Ctrl Pts',(0.445819737468537,-1.,-4.06248560760659));
#53543=CARTESIAN_POINT('Ctrl Pts',(0.445819737468537,1.,-4.06248560760659));
#53544=CARTESIAN_POINT('Ctrl Pts',(0.443561262395332,-1.,-4.0698782192569));
#53545=CARTESIAN_POINT('Ctrl Pts',(0.443561262395332,1.,-4.0698782192569));
#53546=CARTESIAN_POINT('Ctrl Pts',(0.44126495139636,-1.,-4.07726792490016));
#53547=CARTESIAN_POINT('Ctrl Pts',(0.44126495139636,1.,-4.07726792490016));
#53548=CARTESIAN_POINT('Ctrl Pts',(0.438931108931279,-1.,-4.08465462294273));
#53549=CARTESIAN_POINT('Ctrl Pts',(0.438931108931279,1.,-4.08465462294273));
#53550=CARTESIAN_POINT('Ctrl Pts',(0.436560044913482,-1.,-4.09203832139089));
#53551=CARTESIAN_POINT('Ctrl Pts',(0.436560044913482,1.,-4.09203832139089));
#53552=CARTESIAN_POINT('Ctrl Pts',(0.43415207320046,-1.,-4.09941908688373));
#53553=CARTESIAN_POINT('Ctrl Pts',(0.43415207320046,1.,-4.09941908688373));
#53554=CARTESIAN_POINT('Ctrl Pts',(0.431707508679883,-1.,-4.10679698750336));
#53555=CARTESIAN_POINT('Ctrl Pts',(0.431707508679883,1.,-4.10679698750336));
#53556=CARTESIAN_POINT('Ctrl Pts',(0.429226666075844,-1.,-4.11417202783267));
#53557=CARTESIAN_POINT('Ctrl Pts',(0.429226666075844,1.,-4.11417202783267));
#53558=CARTESIAN_POINT('Ctrl Pts',(0.426709855707,-1.,-4.12154412502007));
#53559=CARTESIAN_POINT('Ctrl Pts',(0.426709855707,1.,-4.12154412502007));
#53560=CARTESIAN_POINT('Ctrl Pts',(0.424157375323975,-1.,-4.12891314634572));
#53561=CARTESIAN_POINT('Ctrl Pts',(0.424157375323975,1.,-4.12891314634572));
#53562=CARTESIAN_POINT('Ctrl Pts',(0.421569503104512,-1.,-4.13627893207002));
#53563=CARTESIAN_POINT('Ctrl Pts',(0.421569503104512,1.,-4.13627893207002));
#53564=CARTESIAN_POINT('Ctrl Pts',(0.418946490667702,-1.,-4.14364132317121));
#53565=CARTESIAN_POINT('Ctrl Pts',(0.418946490667702,1.,-4.14364132317121));
#53566=CARTESIAN_POINT('Ctrl Pts',(0.416288556008011,-1.,-4.15100018949965));
#53567=CARTESIAN_POINT('Ctrl Pts',(0.416288556008011,1.,-4.15100018949965));
#53568=CARTESIAN_POINT('Ctrl Pts',(0.41359587795147,-1.,-4.15835545017202));
#53569=CARTESIAN_POINT('Ctrl Pts',(0.41359587795147,1.,-4.15835545017202));
#53570=CARTESIAN_POINT('Ctrl Pts',(0.410868596146414,-1.,-4.16570705938425));
#53571=CARTESIAN_POINT('Ctrl Pts',(0.410868596146414,1.,-4.16570705938425));
#53572=CARTESIAN_POINT('Ctrl Pts',(0.408659167568273,-1.,-4.17158541007977));
#53573=CARTESIAN_POINT('Ctrl Pts',(0.408659167568273,1.,-4.17158541007977));
#53574=CARTESIAN_POINT('Ctrl Pts',(0.406986596325454,-1.,-4.17599251954382));
#53575=CARTESIAN_POINT('Ctrl Pts',(0.406986596325454,1.,-4.17599251954382));
#53576=CARTESIAN_POINT('Ctrl Pts',(0.405864662679209,-1.,-4.17892985789466));
#53577=CARTESIAN_POINT('Ctrl Pts',(0.405864662679209,1.,-4.17892985789466));
#53578=CARTESIAN_POINT('Ctrl Pts',(0.40530197431835,-1.,-4.18039834341342));
#53579=CARTESIAN_POINT('Ctrl Pts',(0.40530197431835,1.,-4.18039834341342));
#53580=CARTESIAN_POINT('',(0.496319364827593,1.,-3.71701050416825));
#53581=CARTESIAN_POINT('Ctrl Pts',(0.496319364827592,-1.,-3.71701050416825));
#53582=CARTESIAN_POINT('Ctrl Pts',(0.496319364827592,-0.666666666666667,
-3.71701050416825));
#53583=CARTESIAN_POINT('Ctrl Pts',(0.496319364827592,-0.333333333333333,
-3.71701050416825));
#53584=CARTESIAN_POINT('Ctrl Pts',(0.496319364827592,0.333333333333333,
-3.71701050416825));
#53585=CARTESIAN_POINT('Ctrl Pts',(0.496319364827592,0.666666666666667,
-3.71701050416825));
#53586=CARTESIAN_POINT('Ctrl Pts',(0.496319364827592,1.,-3.71701050416825));
#53587=CARTESIAN_POINT('',(0.40530197431835,1.,-4.18039834341342));
#53588=CARTESIAN_POINT('',(0.40530197431835,0.,-4.18039834341342));
#53589=CARTESIAN_POINT('Ctrl Pts',(0.496319364827593,1.,-3.71701050416825));
#53590=CARTESIAN_POINT('Ctrl Pts',(0.496354087924312,1.,-3.71704500630495));
#53591=CARTESIAN_POINT('Ctrl Pts',(0.496446644158005,1.,-3.71721917030355));
#53592=CARTESIAN_POINT('Ctrl Pts',(0.496605651525989,1.,-3.71785517607549));
#53593=CARTESIAN_POINT('Ctrl Pts',(0.496846224822564,1.,-3.71952320822499));
#53594=CARTESIAN_POINT('Ctrl Pts',(0.497187079575988,1.,-3.72301489774398));
#53595=CARTESIAN_POINT('Ctrl Pts',(0.497584067153049,1.,-3.72830430904606));
#53596=CARTESIAN_POINT('Ctrl Pts',(0.497984209510024,1.,-3.73486914372449));
#53597=CARTESIAN_POINT('Ctrl Pts',(0.498350586057692,1.,-3.74235701734714));
#53598=CARTESIAN_POINT('Ctrl Pts',(0.498642802042605,1.,-3.75037362167839));
#53599=CARTESIAN_POINT('Ctrl Pts',(0.498823681615421,1.,-3.75854082221052));
#53600=CARTESIAN_POINT('Ctrl Pts',(0.49886579233529,1.,-3.76655401191229));
#53601=CARTESIAN_POINT('Ctrl Pts',(0.498759900365891,1.,-3.77425499225255));
#53602=CARTESIAN_POINT('Ctrl Pts',(0.498515471679584,1.,-3.78163975337356));
#53603=CARTESIAN_POINT('Ctrl Pts',(0.498152751800958,1.,-3.78879701661264));
#53604=CARTESIAN_POINT('Ctrl Pts',(0.497696892100624,1.,-3.79586380669994));
#53605=CARTESIAN_POINT('Ctrl Pts',(0.497171756201051,1.,-3.80297788298514));
#53606=CARTESIAN_POINT('Ctrl Pts',(0.496592643443704,1.,-3.81022254090839));
#53607=CARTESIAN_POINT('Ctrl Pts',(0.495963937875479,1.,-3.81760756144025));
#53608=CARTESIAN_POINT('Ctrl Pts',(0.495283458893837,1.,-3.82509963594103));
#53609=CARTESIAN_POINT('Ctrl Pts',(0.494545212256401,1.,-3.83264092682431));
#53610=CARTESIAN_POINT('Ctrl Pts',(0.493742574629134,1.,-3.84017095578451));
#53611=CARTESIAN_POINT('Ctrl Pts',(0.49287179241414,1.,-3.84765051147999));
#53612=CARTESIAN_POINT('Ctrl Pts',(0.491933631083813,1.,-3.85507287020263));
#53613=CARTESIAN_POINT('Ctrl Pts',(0.490931482170891,1.,-3.86245057319246));
#53614=CARTESIAN_POINT('Ctrl Pts',(0.489870245704917,1.,-3.86980755613707));
#53615=CARTESIAN_POINT('Ctrl Pts',(0.488754973798273,1.,-3.87716963231109));
#53616=CARTESIAN_POINT('Ctrl Pts',(0.487589452275154,1.,-3.88455453328138));
#53617=CARTESIAN_POINT('Ctrl Pts',(0.486375337854103,1.,-3.89196582437552));
#53618=CARTESIAN_POINT('Ctrl Pts',(0.485112963522222,1.,-3.89939844658513));
#53619=CARTESIAN_POINT('Ctrl Pts',(0.48380183508915,1.,-3.90684210358056));
#53620=CARTESIAN_POINT('Ctrl Pts',(0.482441230340713,1.,-3.91428536373751));
#53621=CARTESIAN_POINT('Ctrl Pts',(0.481030798910748,1.,-3.92171976072341));
#53622=CARTESIAN_POINT('Ctrl Pts',(0.479571028525578,1.,-3.92914297392071));
#53623=CARTESIAN_POINT('Ctrl Pts',(0.478062927140964,1.,-3.93655660689819));
#53624=CARTESIAN_POINT('Ctrl Pts',(0.476507810658537,1.,-3.94396469119383));
#53625=CARTESIAN_POINT('Ctrl Pts',(0.47490705302179,1.,-3.95137192932897));
#53626=CARTESIAN_POINT('Ctrl Pts',(0.473261847236297,1.,-3.95878201038338));
#53627=CARTESIAN_POINT('Ctrl Pts',(0.471572978413503,1.,-3.96619600864643));
#53628=CARTESIAN_POINT('Ctrl Pts',(0.469840942829895,1.,-3.97361320212436));
#53629=CARTESIAN_POINT('Ctrl Pts',(0.468066047920157,1.,-3.98103175589371));
#53630=CARTESIAN_POINT('Ctrl Pts',(0.466248520883039,1.,-3.98844946363262));
#53631=CARTESIAN_POINT('Ctrl Pts',(0.464388610938975,1.,-3.9958644432011));
#53632=CARTESIAN_POINT('Ctrl Pts',(0.462486702616204,1.,-4.00327590659075));
#53633=CARTESIAN_POINT('Ctrl Pts',(0.460543280768514,1.,-4.01068390573399));
#53634=CARTESIAN_POINT('Ctrl Pts',(0.458558885636945,1.,-4.01808900827587));
#53635=CARTESIAN_POINT('Ctrl Pts',(0.45653407078495,1.,-4.02549199038394));
#53636=CARTESIAN_POINT('Ctrl Pts',(0.454469363020541,1.,-4.03289354362794));
#53637=CARTESIAN_POINT('Ctrl Pts',(0.452365214748892,1.,-4.04029392228049));
#53638=CARTESIAN_POINT('Ctrl Pts',(0.450222009543926,1.,-4.0476929901813));
#53639=CARTESIAN_POINT('Ctrl Pts',(0.448040082684114,1.,-4.0550903779696));
#53640=CARTESIAN_POINT('Ctrl Pts',(0.445819737468537,1.,-4.06248560760659));
#53641=CARTESIAN_POINT('Ctrl Pts',(0.443561262395332,1.,-4.0698782192569));
#53642=CARTESIAN_POINT('Ctrl Pts',(0.44126495139636,1.,-4.07726792490016));
#53643=CARTESIAN_POINT('Ctrl Pts',(0.438931108931279,1.,-4.08465462294273));
#53644=CARTESIAN_POINT('Ctrl Pts',(0.436560044913482,1.,-4.09203832139089));
#53645=CARTESIAN_POINT('Ctrl Pts',(0.43415207320046,1.,-4.09941908688373));
#53646=CARTESIAN_POINT('Ctrl Pts',(0.431707508679883,1.,-4.10679698750336));
#53647=CARTESIAN_POINT('Ctrl Pts',(0.429226666075844,1.,-4.11417202783267));
#53648=CARTESIAN_POINT('Ctrl Pts',(0.426709855707,1.,-4.12154412502007));
#53649=CARTESIAN_POINT('Ctrl Pts',(0.424157375323975,1.,-4.12891314634572));
#53650=CARTESIAN_POINT('Ctrl Pts',(0.421569503104512,1.,-4.13627893207002));
#53651=CARTESIAN_POINT('Ctrl Pts',(0.418946490667702,1.,-4.14364132317121));
#53652=CARTESIAN_POINT('Ctrl Pts',(0.416288556008011,1.,-4.15100018949965));
#53653=CARTESIAN_POINT('Ctrl Pts',(0.41359587795147,1.,-4.15835545017202));
#53654=CARTESIAN_POINT('Ctrl Pts',(0.410868596146414,1.,-4.16570705938425));
#53655=CARTESIAN_POINT('Ctrl Pts',(0.408659167568273,1.,-4.17158541007977));
#53656=CARTESIAN_POINT('Ctrl Pts',(0.406986596325454,1.,-4.17599251954382));
#53657=CARTESIAN_POINT('Ctrl Pts',(0.405864662679209,1.,-4.17892985789466));
#53658=CARTESIAN_POINT('Ctrl Pts',(0.40530197431835,1.,-4.18039834341342));
#53659=CARTESIAN_POINT('Origin',(0.40530197431835,0.,-4.18039834341342));
#53660=CARTESIAN_POINT('',(0.253646344052522,1.,-4.1923339003649));
#53661=CARTESIAN_POINT('Origin',(0.,0.,0.));
#53662=CARTESIAN_POINT('',(0.67659164797366,1.,-3.68845817949618));
#53663=CARTESIAN_POINT('Origin',(0.,1.,0.));
#53664=CARTESIAN_POINT('Ctrl Pts',(0.67659164797366,1.,-3.68845817949618));
#53665=CARTESIAN_POINT('Ctrl Pts',(0.67659164797366,0.666666666666667,-3.68845817949618));
#53666=CARTESIAN_POINT('Ctrl Pts',(0.67659164797366,0.333333333333333,-3.68845817949618));
#53667=CARTESIAN_POINT('Ctrl Pts',(0.67659164797366,-0.333333333333333,
-3.68845817949618));
#53668=CARTESIAN_POINT('Ctrl Pts',(0.676591647973661,-0.666666666666667,
-3.68845817949618));
#53669=CARTESIAN_POINT('Ctrl Pts',(0.676591647973661,-1.,-3.68845817949618));
#53670=CARTESIAN_POINT('Ctrl Pts',(0.906349047628866,-1.,-4.10104028313088));
#53671=CARTESIAN_POINT('Ctrl Pts',(0.906349047628866,1.,-4.10104028313088));
#53672=CARTESIAN_POINT('Ctrl Pts',(0.905360112216302,-1.,-4.09981755067956));
#53673=CARTESIAN_POINT('Ctrl Pts',(0.905360112216302,1.,-4.09981755067956));
#53674=CARTESIAN_POINT('Ctrl Pts',(0.903385402444212,-1.,-4.09737067247114));
#53675=CARTESIAN_POINT('Ctrl Pts',(0.903385402444212,1.,-4.09737067247114));
#53676=CARTESIAN_POINT('Ctrl Pts',(0.900432820945975,-1.,-4.09369611524319));
#53677=CARTESIAN_POINT('Ctrl Pts',(0.900432820945975,1.,-4.09369611524319));
#53678=CARTESIAN_POINT('Ctrl Pts',(0.896515019236368,-1.,-4.08878822249095));
#53679=CARTESIAN_POINT('Ctrl Pts',(0.896515019236368,1.,-4.08878822249095));
#53680=CARTESIAN_POINT('Ctrl Pts',(0.891649447920401,-1.,-4.08263920306651));
#53681=CARTESIAN_POINT('Ctrl Pts',(0.891649447920401,1.,-4.08263920306651));
#53682=CARTESIAN_POINT('Ctrl Pts',(0.886815658360739,-1.,-4.07647601774639));
#53683=CARTESIAN_POINT('Ctrl Pts',(0.886815658360739,1.,-4.07647601774639));
#53684=CARTESIAN_POINT('Ctrl Pts',(0.882013797525916,-1.,-4.07029866694292));
#53685=CARTESIAN_POINT('Ctrl Pts',(0.882013797525916,1.,-4.07029866694292));
#53686=CARTESIAN_POINT('Ctrl Pts',(0.877244060484595,-1.,-4.06410717232347));
#53687=CARTESIAN_POINT('Ctrl Pts',(0.877244060484595,1.,-4.06410717232347));
#53688=CARTESIAN_POINT('Ctrl Pts',(0.872506694780563,-1.,-4.05790159030495));
#53689=CARTESIAN_POINT('Ctrl Pts',(0.872506694780563,1.,-4.05790159030495));
#53690=CARTESIAN_POINT('Ctrl Pts',(0.867801988858176,-1.,-4.05168199437128));
#53691=CARTESIAN_POINT('Ctrl Pts',(0.867801988858176,1.,-4.05168199437128));
#53692=CARTESIAN_POINT('Ctrl Pts',(0.863130256642173,-1.,-4.04544845048097));
#53693=CARTESIAN_POINT('Ctrl Pts',(0.863130256642173,1.,-4.04544845048097));
#53694=CARTESIAN_POINT('Ctrl Pts',(0.858491822322571,-1.,-4.03920099284658));
#53695=CARTESIAN_POINT('Ctrl Pts',(0.858491822322571,1.,-4.03920099284658));
#53696=CARTESIAN_POINT('Ctrl Pts',(0.853887006632178,-1.,-4.03293960436946));
#53697=CARTESIAN_POINT('Ctrl Pts',(0.853887006632178,1.,-4.03293960436946));
#53698=CARTESIAN_POINT('Ctrl Pts',(0.849316107475012,-1.,-4.02666418343508));
#53699=CARTESIAN_POINT('Ctrl Pts',(0.849316107475012,1.,-4.02666418343508));
#53700=CARTESIAN_POINT('Ctrl Pts',(0.844779403288517,-1.,-4.02037456798787));
#53701=CARTESIAN_POINT('Ctrl Pts',(0.844779403288517,1.,-4.02037456798787));
#53702=CARTESIAN_POINT('Ctrl Pts',(0.84027717197638,-1.,-4.01407059766338));
#53703=CARTESIAN_POINT('Ctrl Pts',(0.84027717197638,1.,-4.01407059766338));
#53704=CARTESIAN_POINT('Ctrl Pts',(0.835809705809821,-1.,-4.00775216907934));
#53705=CARTESIAN_POINT('Ctrl Pts',(0.835809705809821,1.,-4.00775216907934));
#53706=CARTESIAN_POINT('Ctrl Pts',(0.831377325741487,-1.,-4.00141928477447));
#53707=CARTESIAN_POINT('Ctrl Pts',(0.831377325741487,1.,-4.00141928477447));
#53708=CARTESIAN_POINT('Ctrl Pts',(0.826980400320473,-1.,-3.99507212784289));
#53709=CARTESIAN_POINT('Ctrl Pts',(0.826980400320473,1.,-3.99507212784289));
#53710=CARTESIAN_POINT('Ctrl Pts',(0.822619346021769,-1.,-3.98871104646328));
#53711=CARTESIAN_POINT('Ctrl Pts',(0.822619346021769,1.,-3.98871104646328));
#53712=CARTESIAN_POINT('Ctrl Pts',(0.818294599022033,-1.,-3.98233640155287));
#53713=CARTESIAN_POINT('Ctrl Pts',(0.818294599022033,1.,-3.98233640155287));
#53714=CARTESIAN_POINT('Ctrl Pts',(0.814006592328737,-1.,-3.97594844078763));
#53715=CARTESIAN_POINT('Ctrl Pts',(0.814006592328737,1.,-3.97594844078763));
#53716=CARTESIAN_POINT('Ctrl Pts',(0.809755732818134,-1.,-3.96954717513251));
#53717=CARTESIAN_POINT('Ctrl Pts',(0.809755732818134,1.,-3.96954717513251));
#53718=CARTESIAN_POINT('Ctrl Pts',(0.805542372178495,-1.,-3.96313222295874));
#53719=CARTESIAN_POINT('Ctrl Pts',(0.805542372178495,1.,-3.96313222295874));
#53720=CARTESIAN_POINT('Ctrl Pts',(0.801366797727206,-1.,-3.95670276375176));
#53721=CARTESIAN_POINT('Ctrl Pts',(0.801366797727206,1.,-3.95670276375176));
#53722=CARTESIAN_POINT('Ctrl Pts',(0.797229296085438,-1.,-3.95025788827189));
#53723=CARTESIAN_POINT('Ctrl Pts',(0.797229296085438,1.,-3.95025788827189));
#53724=CARTESIAN_POINT('Ctrl Pts',(0.793130205641017,-1.,-3.94379688971307));
#53725=CARTESIAN_POINT('Ctrl Pts',(0.793130205641017,1.,-3.94379688971307));
#53726=CARTESIAN_POINT('Ctrl Pts',(0.789069971469323,-1.,-3.93731956885671));
#53727=CARTESIAN_POINT('Ctrl Pts',(0.789069971469323,1.,-3.93731956885671));
#53728=CARTESIAN_POINT('Ctrl Pts',(0.785049202786458,-1.,-3.93082655631769));
#53729=CARTESIAN_POINT('Ctrl Pts',(0.785049202786458,1.,-3.93082655631769));
#53730=CARTESIAN_POINT('Ctrl Pts',(0.781068718228395,-1.,-3.92431956510418));
#53731=CARTESIAN_POINT('Ctrl Pts',(0.781068718228395,1.,-3.92431956510418));
#53732=CARTESIAN_POINT('Ctrl Pts',(0.777129415664915,-1.,-3.91780062334464));
#53733=CARTESIAN_POINT('Ctrl Pts',(0.777129415664915,1.,-3.91780062334464));
#53734=CARTESIAN_POINT('Ctrl Pts',(0.773232154506305,-1.,-3.91127138115238));
#53735=CARTESIAN_POINT('Ctrl Pts',(0.773232154506305,1.,-3.91127138115238));
#53736=CARTESIAN_POINT('Ctrl Pts',(0.769377629847876,-1.,-3.90473237182634));
#53737=CARTESIAN_POINT('Ctrl Pts',(0.769377629847876,1.,-3.90473237182634));
#53738=CARTESIAN_POINT('Ctrl Pts',(0.765566256401306,-1.,-3.89818233104381));
#53739=CARTESIAN_POINT('Ctrl Pts',(0.765566256401306,1.,-3.89818233104381));
#53740=CARTESIAN_POINT('Ctrl Pts',(0.761798028793978,-1.,-3.89161738162245));
#53741=CARTESIAN_POINT('Ctrl Pts',(0.761798028793978,1.,-3.89161738162245));
#53742=CARTESIAN_POINT('Ctrl Pts',(0.758072800564798,-1.,-3.88503262662684));
#53743=CARTESIAN_POINT('Ctrl Pts',(0.758072800564798,1.,-3.88503262662684));
#53744=CARTESIAN_POINT('Ctrl Pts',(0.754390577396846,-1.,-3.87842382520058));
#53745=CARTESIAN_POINT('Ctrl Pts',(0.754390577396846,1.,-3.87842382520058));
#53746=CARTESIAN_POINT('Ctrl Pts',(0.750751822383023,-1.,-3.87178914078372));
#53747=CARTESIAN_POINT('Ctrl Pts',(0.750751822383023,1.,-3.87178914078372));
#53748=CARTESIAN_POINT('Ctrl Pts',(0.747157716488884,-1.,-3.86513062969896));
#53749=CARTESIAN_POINT('Ctrl Pts',(0.747157716488884,1.,-3.86513062969896));
#53750=CARTESIAN_POINT('Ctrl Pts',(0.743610542737041,-1.,-3.85845645217611));
#53751=CARTESIAN_POINT('Ctrl Pts',(0.743610542737041,1.,-3.85845645217611));
#53752=CARTESIAN_POINT('Ctrl Pts',(0.740113146827176,-1.,-3.85177770351237));
#53753=CARTESIAN_POINT('Ctrl Pts',(0.740113146827176,1.,-3.85177770351237));
#53754=CARTESIAN_POINT('Ctrl Pts',(0.736668240497151,-1.,-3.84510432881231));
#53755=CARTESIAN_POINT('Ctrl Pts',(0.736668240497151,1.,-3.84510432881231));
#53756=CARTESIAN_POINT('Ctrl Pts',(0.73327770375609,-1.,-3.83844103658016));
#53757=CARTESIAN_POINT('Ctrl Pts',(0.73327770375609,1.,-3.83844103658016));
#53758=CARTESIAN_POINT('Ctrl Pts',(0.729942010490145,-1.,-3.83178392403371));
#53759=CARTESIAN_POINT('Ctrl Pts',(0.729942010490145,1.,-3.83178392403371));
#53760=CARTESIAN_POINT('Ctrl Pts',(0.726659281876608,-1.,-3.82511495756682));
#53761=CARTESIAN_POINT('Ctrl Pts',(0.726659281876608,1.,-3.82511495756682));
#53762=CARTESIAN_POINT('Ctrl Pts',(0.723426346019349,-1.,-3.81840802610795));
#53763=CARTESIAN_POINT('Ctrl Pts',(0.723426346019349,1.,-3.81840802610795));
#53764=CARTESIAN_POINT('Ctrl Pts',(0.720240466589172,-1.,-3.81163885127309));
#53765=CARTESIAN_POINT('Ctrl Pts',(0.720240466589172,1.,-3.81163885127309));
#53766=CARTESIAN_POINT('Ctrl Pts',(0.717100993669091,-1.,-3.80479445759296));
#53767=CARTESIAN_POINT('Ctrl Pts',(0.717100993669091,1.,-3.80479445759296));
#53768=CARTESIAN_POINT('Ctrl Pts',(0.714010733006677,-1.,-3.79788100314994));
#53769=CARTESIAN_POINT('Ctrl Pts',(0.714010733006677,1.,-3.79788100314994));
#53770=CARTESIAN_POINT('Ctrl Pts',(0.710978231689117,-1.,-3.79093694007146));
#53771=CARTESIAN_POINT('Ctrl Pts',(0.710978231689117,1.,-3.79093694007146));
#53772=CARTESIAN_POINT('Ctrl Pts',(0.7080158793756,-1.,-3.78402183336678));
#53773=CARTESIAN_POINT('Ctrl Pts',(0.7080158793756,1.,-3.78402183336678));
#53774=CARTESIAN_POINT('Ctrl Pts',(0.705135847999949,-1.,-3.77719254217197));
#53775=CARTESIAN_POINT('Ctrl Pts',(0.705135847999949,1.,-3.77719254217197));
#53776=CARTESIAN_POINT('Ctrl Pts',(0.702346356621613,-1.,-3.77048141872904));
#53777=CARTESIAN_POINT('Ctrl Pts',(0.702346356621613,1.,-3.77048141872904));
#53778=CARTESIAN_POINT('Ctrl Pts',(0.699648552230851,-1.,-3.76387780603725));
#53779=CARTESIAN_POINT('Ctrl Pts',(0.699648552230851,1.,-3.76387780603725));
#53780=CARTESIAN_POINT('Ctrl Pts',(0.69703124565953,-1.,-3.75729775766913));
#53781=CARTESIAN_POINT('Ctrl Pts',(0.69703124565953,1.,-3.75729775766913));
#53782=CARTESIAN_POINT('Ctrl Pts',(0.694474562581173,-1.,-3.7506028824329));
#53783=CARTESIAN_POINT('Ctrl Pts',(0.694474562581173,1.,-3.7506028824329));
#53784=CARTESIAN_POINT('Ctrl Pts',(0.691960080400503,-1.,-3.74365508986548));
#53785=CARTESIAN_POINT('Ctrl Pts',(0.691960080400503,1.,-3.74365508986548));
#53786=CARTESIAN_POINT('Ctrl Pts',(0.689479637354651,-1.,-3.73636374474993));
#53787=CARTESIAN_POINT('Ctrl Pts',(0.689479637354651,1.,-3.73636374474993));
#53788=CARTESIAN_POINT('Ctrl Pts',(0.687043475232499,-1.,-3.72872973554125));
#53789=CARTESIAN_POINT('Ctrl Pts',(0.687043475232499,1.,-3.72872973554125));
#53790=CARTESIAN_POINT('Ctrl Pts',(0.684691698168355,-1.,-3.7209063713952));
#53791=CARTESIAN_POINT('Ctrl Pts',(0.684691698168355,1.,-3.7209063713952));
#53792=CARTESIAN_POINT('Ctrl Pts',(0.682492345109689,-1.,-3.71319182790334));
#53793=CARTESIAN_POINT('Ctrl Pts',(0.682492345109689,1.,-3.71319182790334));
#53794=CARTESIAN_POINT('Ctrl Pts',(0.680526909711617,-1.,-3.70595722032165));
#53795=CARTESIAN_POINT('Ctrl Pts',(0.680526909711617,1.,-3.70595722032165));
#53796=CARTESIAN_POINT('Ctrl Pts',(0.678878822226389,-1.,-3.69959004073192));
#53797=CARTESIAN_POINT('Ctrl Pts',(0.678878822226389,1.,-3.69959004073192));
#53798=CARTESIAN_POINT('Ctrl Pts',(0.677621861865196,-1.,-3.69443683573443));
#53799=CARTESIAN_POINT('Ctrl Pts',(0.677621861865196,1.,-3.69443683573443));
#53800=CARTESIAN_POINT('Ctrl Pts',(0.67680581107414,-1.,-3.69073278191505));
#53801=CARTESIAN_POINT('Ctrl Pts',(0.67680581107414,1.,-3.69073278191505));
#53802=CARTESIAN_POINT('Ctrl Pts',(0.676524321060166,-1.,-3.68901718135636));
#53803=CARTESIAN_POINT('Ctrl Pts',(0.676524321060166,1.,-3.68901718135636));
#53804=CARTESIAN_POINT('Ctrl Pts',(0.676525601650139,-1.,-3.68844918120934));
#53805=CARTESIAN_POINT('Ctrl Pts',(0.676525601650139,1.,-3.68844918120934));
#53806=CARTESIAN_POINT('Ctrl Pts',(0.676620796001716,-1.,-3.68838970675356));
#53807=CARTESIAN_POINT('Ctrl Pts',(0.676620796001716,1.,-3.68838970675356));
#53808=CARTESIAN_POINT('Ctrl Pts',(0.676691979611562,-1.,-3.68843977377012));
#53809=CARTESIAN_POINT('Ctrl Pts',(0.676691979611562,1.,-3.68843977377012));
#53810=CARTESIAN_POINT('',(0.906349047628866,1.,-4.10104028313088));
#53811=CARTESIAN_POINT('Ctrl Pts',(0.906349047628866,1.,-4.10104028313088));
#53812=CARTESIAN_POINT('Ctrl Pts',(0.905360112216302,1.,-4.09981755067956));
#53813=CARTESIAN_POINT('Ctrl Pts',(0.903385402444212,1.,-4.09737067247114));
#53814=CARTESIAN_POINT('Ctrl Pts',(0.900432820945975,1.,-4.09369611524319));
#53815=CARTESIAN_POINT('Ctrl Pts',(0.896515019236368,1.,-4.08878822249095));
#53816=CARTESIAN_POINT('Ctrl Pts',(0.891649447920401,1.,-4.08263920306651));
#53817=CARTESIAN_POINT('Ctrl Pts',(0.886815658360739,1.,-4.07647601774639));
#53818=CARTESIAN_POINT('Ctrl Pts',(0.882013797525916,1.,-4.07029866694292));
#53819=CARTESIAN_POINT('Ctrl Pts',(0.877244060484595,1.,-4.06410717232347));
#53820=CARTESIAN_POINT('Ctrl Pts',(0.872506694780563,1.,-4.05790159030495));
#53821=CARTESIAN_POINT('Ctrl Pts',(0.867801988858176,1.,-4.05168199437128));
#53822=CARTESIAN_POINT('Ctrl Pts',(0.863130256642173,1.,-4.04544845048097));
#53823=CARTESIAN_POINT('Ctrl Pts',(0.858491822322571,1.,-4.03920099284658));
#53824=CARTESIAN_POINT('Ctrl Pts',(0.853887006632178,1.,-4.03293960436946));
#53825=CARTESIAN_POINT('Ctrl Pts',(0.849316107475012,1.,-4.02666418343508));
#53826=CARTESIAN_POINT('Ctrl Pts',(0.844779403288517,1.,-4.02037456798787));
#53827=CARTESIAN_POINT('Ctrl Pts',(0.84027717197638,1.,-4.01407059766338));
#53828=CARTESIAN_POINT('Ctrl Pts',(0.835809705809821,1.,-4.00775216907934));
#53829=CARTESIAN_POINT('Ctrl Pts',(0.831377325741487,1.,-4.00141928477447));
#53830=CARTESIAN_POINT('Ctrl Pts',(0.826980400320473,1.,-3.99507212784289));
#53831=CARTESIAN_POINT('Ctrl Pts',(0.822619346021769,1.,-3.98871104646328));
#53832=CARTESIAN_POINT('Ctrl Pts',(0.818294599022033,1.,-3.98233640155287));
#53833=CARTESIAN_POINT('Ctrl Pts',(0.814006592328737,1.,-3.97594844078763));
#53834=CARTESIAN_POINT('Ctrl Pts',(0.809755732818134,1.,-3.96954717513251));
#53835=CARTESIAN_POINT('Ctrl Pts',(0.805542372178495,1.,-3.96313222295874));
#53836=CARTESIAN_POINT('Ctrl Pts',(0.801366797727206,1.,-3.95670276375176));
#53837=CARTESIAN_POINT('Ctrl Pts',(0.797229296085438,1.,-3.95025788827189));
#53838=CARTESIAN_POINT('Ctrl Pts',(0.793130205641017,1.,-3.94379688971307));
#53839=CARTESIAN_POINT('Ctrl Pts',(0.789069971469323,1.,-3.93731956885671));
#53840=CARTESIAN_POINT('Ctrl Pts',(0.785049202786458,1.,-3.93082655631769));
#53841=CARTESIAN_POINT('Ctrl Pts',(0.781068718228395,1.,-3.92431956510418));
#53842=CARTESIAN_POINT('Ctrl Pts',(0.777129415664915,1.,-3.91780062334464));
#53843=CARTESIAN_POINT('Ctrl Pts',(0.773232154506305,1.,-3.91127138115238));
#53844=CARTESIAN_POINT('Ctrl Pts',(0.769377629847876,1.,-3.90473237182634));
#53845=CARTESIAN_POINT('Ctrl Pts',(0.765566256401306,1.,-3.89818233104381));
#53846=CARTESIAN_POINT('Ctrl Pts',(0.761798028793978,1.,-3.89161738162245));
#53847=CARTESIAN_POINT('Ctrl Pts',(0.758072800564798,1.,-3.88503262662684));
#53848=CARTESIAN_POINT('Ctrl Pts',(0.754390577396846,1.,-3.87842382520058));
#53849=CARTESIAN_POINT('Ctrl Pts',(0.750751822383023,1.,-3.87178914078372));
#53850=CARTESIAN_POINT('Ctrl Pts',(0.747157716488884,1.,-3.86513062969896));
#53851=CARTESIAN_POINT('Ctrl Pts',(0.743610542737041,1.,-3.85845645217611));
#53852=CARTESIAN_POINT('Ctrl Pts',(0.740113146827176,1.,-3.85177770351237));
#53853=CARTESIAN_POINT('Ctrl Pts',(0.736668240497151,1.,-3.84510432881231));
#53854=CARTESIAN_POINT('Ctrl Pts',(0.73327770375609,1.,-3.83844103658016));
#53855=CARTESIAN_POINT('Ctrl Pts',(0.729942010490145,1.,-3.83178392403371));
#53856=CARTESIAN_POINT('Ctrl Pts',(0.726659281876608,1.,-3.82511495756682));
#53857=CARTESIAN_POINT('Ctrl Pts',(0.723426346019349,1.,-3.81840802610795));
#53858=CARTESIAN_POINT('Ctrl Pts',(0.720240466589172,1.,-3.81163885127309));
#53859=CARTESIAN_POINT('Ctrl Pts',(0.717100993669091,1.,-3.80479445759296));
#53860=CARTESIAN_POINT('Ctrl Pts',(0.714010733006677,1.,-3.79788100314994));
#53861=CARTESIAN_POINT('Ctrl Pts',(0.710978231689117,1.,-3.79093694007146));
#53862=CARTESIAN_POINT('Ctrl Pts',(0.7080158793756,1.,-3.78402183336678));
#53863=CARTESIAN_POINT('Ctrl Pts',(0.705135847999949,1.,-3.77719254217197));
#53864=CARTESIAN_POINT('Ctrl Pts',(0.702346356621613,1.,-3.77048141872904));
#53865=CARTESIAN_POINT('Ctrl Pts',(0.699648552230851,1.,-3.76387780603725));
#53866=CARTESIAN_POINT('Ctrl Pts',(0.69703124565953,1.,-3.75729775766913));
#53867=CARTESIAN_POINT('Ctrl Pts',(0.694474562581173,1.,-3.7506028824329));
#53868=CARTESIAN_POINT('Ctrl Pts',(0.691960080400503,1.,-3.74365508986548));
#53869=CARTESIAN_POINT('Ctrl Pts',(0.689479637354651,1.,-3.73636374474993));
#53870=CARTESIAN_POINT('Ctrl Pts',(0.687043475232499,1.,-3.72872973554125));
#53871=CARTESIAN_POINT('Ctrl Pts',(0.684691698168355,1.,-3.7209063713952));
#53872=CARTESIAN_POINT('Ctrl Pts',(0.682492345109689,1.,-3.71319182790334));
#53873=CARTESIAN_POINT('Ctrl Pts',(0.680526909711617,1.,-3.70595722032165));
#53874=CARTESIAN_POINT('Ctrl Pts',(0.678878822226389,1.,-3.69959004073192));
#53875=CARTESIAN_POINT('Ctrl Pts',(0.677621861865196,1.,-3.69443683573443));
#53876=CARTESIAN_POINT('Ctrl Pts',(0.676867042599711,1.,-3.6910107117555));
#53877=CARTESIAN_POINT('Ctrl Pts',(0.676580391119535,1.,-3.68934997767391));
#53878=CARTESIAN_POINT('Ctrl Pts',(0.676535079520365,1.,-3.68869596426099));
#53879=CARTESIAN_POINT('Ctrl Pts',(0.67656928609342,1.,-3.68850172300543));
#53880=CARTESIAN_POINT('Ctrl Pts',(0.676591647973661,1.,-3.68845817949618));
#53881=CARTESIAN_POINT('',(0.906349047628866,0.,-4.10104028313088));
#53882=CARTESIAN_POINT('Ctrl Pts',(1.07157964745328,-1.,-3.59363563249864));
#53883=CARTESIAN_POINT('Ctrl Pts',(1.07157964745328,1.,-3.59363563249864));
#53884=CARTESIAN_POINT('Ctrl Pts',(1.07162034256459,-1.,-3.59355870577901));
#53885=CARTESIAN_POINT('Ctrl Pts',(1.07162034256459,1.,-3.59355870577901));
#53886=CARTESIAN_POINT('Ctrl Pts',(1.07173216219145,-1.,-3.59356848057812));
#53887=CARTESIAN_POINT('Ctrl Pts',(1.07173216219145,1.,-3.59356848057812));
#53888=CARTESIAN_POINT('Ctrl Pts',(1.07199116987656,-1.,-3.5940739910409));
#53889=CARTESIAN_POINT('Ctrl Pts',(1.07199116987656,1.,-3.5940739910409));
#53890=CARTESIAN_POINT('Ctrl Pts',(1.07251922679245,-1.,-3.59573039612316));
#53891=CARTESIAN_POINT('Ctrl Pts',(1.07251922679245,1.,-3.59573039612316));
#53892=CARTESIAN_POINT('Ctrl Pts',(1.07347372545714,-1.,-3.59940121154535));
#53893=CARTESIAN_POINT('Ctrl Pts',(1.07347372545714,1.,-3.59940121154535));
#53894=CARTESIAN_POINT('Ctrl Pts',(1.07469327168578,-1.,-3.60456339887778));
#53895=CARTESIAN_POINT('Ctrl Pts',(1.07469327168578,1.,-3.60456339887778));
#53896=CARTESIAN_POINT('Ctrl Pts',(1.07611545402734,-1.,-3.61098481349204));
#53897=CARTESIAN_POINT('Ctrl Pts',(1.07611545402734,1.,-3.61098481349204));
#53898=CARTESIAN_POINT('Ctrl Pts',(1.07764868137619,-1.,-3.61832318504575));
#53899=CARTESIAN_POINT('Ctrl Pts',(1.07764868137619,1.,-3.61832318504575));
#53900=CARTESIAN_POINT('Ctrl Pts',(1.07919137290742,-1.,-3.62619537902361));
#53901=CARTESIAN_POINT('Ctrl Pts',(1.07919137290742,1.,-3.62619537902361));
#53902=CARTESIAN_POINT('Ctrl Pts',(1.08064765719867,-1.,-3.63423373196529));
#53903=CARTESIAN_POINT('Ctrl Pts',(1.08064765719867,1.,-3.63423373196529));
#53904=CARTESIAN_POINT('Ctrl Pts',(1.08194278850996,-1.,-3.64214167843677));
#53905=CARTESIAN_POINT('Ctrl Pts',(1.08194278850996,1.,-3.64214167843677));
#53906=CARTESIAN_POINT('Ctrl Pts',(1.08304289898623,-1.,-3.64976441208358));
#53907=CARTESIAN_POINT('Ctrl Pts',(1.08304289898623,1.,-3.64976441208358));
#53908=CARTESIAN_POINT('Ctrl Pts',(1.08395671077807,-1.,-3.65709649161166));
#53909=CARTESIAN_POINT('Ctrl Pts',(1.08395671077807,1.,-3.65709649161166));
#53910=CARTESIAN_POINT('Ctrl Pts',(1.08471809922901,-1.,-3.66422237895365));
#53911=CARTESIAN_POINT('Ctrl Pts',(1.08471809922901,1.,-3.66422237895365));
#53912=CARTESIAN_POINT('Ctrl Pts',(1.0853733414449,-1.,-3.67127347729666));
#53913=CARTESIAN_POINT('Ctrl Pts',(1.0853733414449,1.,-3.67127347729666));
#53914=CARTESIAN_POINT('Ctrl Pts',(1.0859675575576,-1.,-3.67838211685118));
#53915=CARTESIAN_POINT('Ctrl Pts',(1.0859675575576,1.,-3.67838211685118));
#53916=CARTESIAN_POINT('Ctrl Pts',(1.0865288888259,-1.,-3.68562817420797));
#53917=CARTESIAN_POINT('Ctrl Pts',(1.0865288888259,1.,-3.68562817420797));
#53918=CARTESIAN_POINT('Ctrl Pts',(1.08706319540271,-1.,-3.69302062410157));
#53919=CARTESIAN_POINT('Ctrl Pts',(1.08706319540271,1.,-3.69302062410157));
#53920=CARTESIAN_POINT('Ctrl Pts',(1.08756311291309,-1.,-3.70052690909833));
#53921=CARTESIAN_POINT('Ctrl Pts',(1.08756311291309,1.,-3.70052690909833));
#53922=CARTESIAN_POINT('Ctrl Pts',(1.08801367312185,-1.,-3.70809084139457));
#53923=CARTESIAN_POINT('Ctrl Pts',(1.08801367312185,1.,-3.70809084139457));
#53924=CARTESIAN_POINT('Ctrl Pts',(1.0883988733478,-1.,-3.71565372339075));
#53925=CARTESIAN_POINT('Ctrl Pts',(1.0883988733478,1.,-3.71565372339075));
#53926=CARTESIAN_POINT('Ctrl Pts',(1.08870887220082,-1.,-3.72317741369398));
#53927=CARTESIAN_POINT('Ctrl Pts',(1.08870887220082,1.,-3.72317741369398));
#53928=CARTESIAN_POINT('Ctrl Pts',(1.08894337390937,-1.,-3.73065515162988));
#53929=CARTESIAN_POINT('Ctrl Pts',(1.08894337390937,1.,-3.73065515162988));
#53930=CARTESIAN_POINT('Ctrl Pts',(1.08910769013297,-1.,-3.73809879348239));
#53931=CARTESIAN_POINT('Ctrl Pts',(1.08910769013297,1.,-3.73809879348239));
#53932=CARTESIAN_POINT('Ctrl Pts',(1.08921040494017,-1.,-3.74553121371757));
#53933=CARTESIAN_POINT('Ctrl Pts',(1.08921040494017,1.,-3.74553121371757));
#53934=CARTESIAN_POINT('Ctrl Pts',(1.08926054632925,-1.,-3.75297711748132));
#53935=CARTESIAN_POINT('Ctrl Pts',(1.08926054632925,1.,-3.75297711748132));
#53936=CARTESIAN_POINT('Ctrl Pts',(1.08926462734281,-1.,-3.76045342580208));
#53937=CARTESIAN_POINT('Ctrl Pts',(1.08926462734281,1.,-3.76045342580208));
#53938=CARTESIAN_POINT('Ctrl Pts',(1.08922484204256,-1.,-3.76796340094448));
#53939=CARTESIAN_POINT('Ctrl Pts',(1.08922484204256,1.,-3.76796340094448));
#53940=CARTESIAN_POINT('Ctrl Pts',(1.0891407279127,-1.,-3.77550199409424));
#53941=CARTESIAN_POINT('Ctrl Pts',(1.0891407279127,1.,-3.77550199409424));
#53942=CARTESIAN_POINT('Ctrl Pts',(1.08901018614636,-1.,-3.78305911299504));
#53943=CARTESIAN_POINT('Ctrl Pts',(1.08901018614636,1.,-3.78305911299504));
#53944=CARTESIAN_POINT('Ctrl Pts',(1.08883071512098,-1.,-3.79062357974404));
#53945=CARTESIAN_POINT('Ctrl Pts',(1.08883071512098,1.,-3.79062357974404));
#53946=CARTESIAN_POINT('Ctrl Pts',(1.08860064435778,-1.,-3.79818708705259));
#53947=CARTESIAN_POINT('Ctrl Pts',(1.08860064435778,1.,-3.79818708705259));
#53948=CARTESIAN_POINT('Ctrl Pts',(1.0883200925538,-1.,-3.8057472665766));
#53949=CARTESIAN_POINT('Ctrl Pts',(1.0883200925538,1.,-3.8057472665766));
#53950=CARTESIAN_POINT('Ctrl Pts',(1.08799030610862,-1.,-3.81330554446323));
#53951=CARTESIAN_POINT('Ctrl Pts',(1.08799030610862,1.,-3.81330554446323));
#53952=CARTESIAN_POINT('Ctrl Pts',(1.08761321539442,-1.,-3.82086569676319));
#53953=CARTESIAN_POINT('Ctrl Pts',(1.08761321539442,1.,-3.82086569676319));
#53954=CARTESIAN_POINT('Ctrl Pts',(1.08719091307558,-1.,-3.82843215316984));
#53955=CARTESIAN_POINT('Ctrl Pts',(1.08719091307558,1.,-3.82843215316984));
#53956=CARTESIAN_POINT('Ctrl Pts',(1.08672515456902,-1.,-3.83600837071708));
#53957=CARTESIAN_POINT('Ctrl Pts',(1.08672515456902,1.,-3.83600837071708));
#53958=CARTESIAN_POINT('Ctrl Pts',(1.08621688337604,-1.,-3.8435952876495));
#53959=CARTESIAN_POINT('Ctrl Pts',(1.08621688337604,1.,-3.8435952876495));
#53960=CARTESIAN_POINT('Ctrl Pts',(1.08566647671844,-1.,-3.85119211322755));
#53961=CARTESIAN_POINT('Ctrl Pts',(1.08566647671844,1.,-3.85119211322755));
#53962=CARTESIAN_POINT('Ctrl Pts',(1.08507395120059,-1.,-3.85879698702532));
#53963=CARTESIAN_POINT('Ctrl Pts',(1.08507395120059,1.,-3.85879698702532));
#53964=CARTESIAN_POINT('Ctrl Pts',(1.08443918607927,-1.,-3.86640769434274));
#53965=CARTESIAN_POINT('Ctrl Pts',(1.08443918607927,1.,-3.86640769434274));
#53966=CARTESIAN_POINT('Ctrl Pts',(1.08376213307504,-1.,-3.8740223372254));
#53967=CARTESIAN_POINT('Ctrl Pts',(1.08376213307504,1.,-3.8740223372254));
#53968=CARTESIAN_POINT('Ctrl Pts',(1.08304304871028,-1.,-3.88164007721313));
#53969=CARTESIAN_POINT('Ctrl Pts',(1.08304304871028,1.,-3.88164007721313));
#53970=CARTESIAN_POINT('Ctrl Pts',(1.08228241999346,-1.,-3.88926088975114));
#53971=CARTESIAN_POINT('Ctrl Pts',(1.08228241999346,1.,-3.88926088975114));
#53972=CARTESIAN_POINT('Ctrl Pts',(1.08148086931358,-1.,-3.8968852509835));
#53973=CARTESIAN_POINT('Ctrl Pts',(1.08148086931358,1.,-3.8968852509835));
#53974=CARTESIAN_POINT('Ctrl Pts',(1.08063906483818,-1.,-3.90451384092545));
#53975=CARTESIAN_POINT('Ctrl Pts',(1.08063906483818,1.,-3.90451384092545));
#53976=CARTESIAN_POINT('Ctrl Pts',(1.07975763507473,-1.,-3.91214726022143));
#53977=CARTESIAN_POINT('Ctrl Pts',(1.07975763507473,1.,-3.91214726022143));
#53978=CARTESIAN_POINT('Ctrl Pts',(1.07883706663554,-1.,-3.91978568924178));
#53979=CARTESIAN_POINT('Ctrl Pts',(1.07883706663554,1.,-3.91978568924178));
#53980=CARTESIAN_POINT('Ctrl Pts',(1.07787771707195,-1.,-3.9274289334984));
#53981=CARTESIAN_POINT('Ctrl Pts',(1.07787771707195,1.,-3.9274289334984));
#53982=CARTESIAN_POINT('Ctrl Pts',(1.07687985975384,-1.,-3.93507657572883));
#53983=CARTESIAN_POINT('Ctrl Pts',(1.07687985975384,1.,-3.93507657572883));
#53984=CARTESIAN_POINT('Ctrl Pts',(1.07584371946443,-1.,-3.94272809633331));
#53985=CARTESIAN_POINT('Ctrl Pts',(1.07584371946443,1.,-3.94272809633331));
#53986=CARTESIAN_POINT('Ctrl Pts',(1.07476950921587,-1.,-3.95038299600676));
#53987=CARTESIAN_POINT('Ctrl Pts',(1.07476950921587,1.,-3.95038299600676));
#53988=CARTESIAN_POINT('Ctrl Pts',(1.07365747426491,-1.,-3.95804094429373));
#53989=CARTESIAN_POINT('Ctrl Pts',(1.07365747426491,1.,-3.95804094429373));
#53990=CARTESIAN_POINT('Ctrl Pts',(1.07250789943007,-1.,-3.96570179322338));
#53991=CARTESIAN_POINT('Ctrl Pts',(1.07250789943007,1.,-3.96570179322338));
#53992=CARTESIAN_POINT('Ctrl Pts',(1.07132109206164,-1.,-3.9733655022223));
#53993=CARTESIAN_POINT('Ctrl Pts',(1.07132109206164,1.,-3.9733655022223));
#53994=CARTESIAN_POINT('Ctrl Pts',(1.07009737257767,-1.,-3.98103208801101));
#53995=CARTESIAN_POINT('Ctrl Pts',(1.07009737257767,1.,-3.98103208801101));
#53996=CARTESIAN_POINT('Ctrl Pts',(1.06883706263941,-1.,-3.98870156857412));
#53997=CARTESIAN_POINT('Ctrl Pts',(1.06883706263941,1.,-3.98870156857412));
#53998=CARTESIAN_POINT('Ctrl Pts',(1.06754047381312,-1.,-3.99637389920441));
#53999=CARTESIAN_POINT('Ctrl Pts',(1.06754047381312,1.,-3.99637389920441));
#54000=CARTESIAN_POINT('Ctrl Pts',(1.06620789963606,-1.,-4.00404894952579));
#54001=CARTESIAN_POINT('Ctrl Pts',(1.06620789963606,1.,-4.00404894952579));
#54002=CARTESIAN_POINT('Ctrl Pts',(1.06483961343109,-1.,-4.01172654187398));
#54003=CARTESIAN_POINT('Ctrl Pts',(1.06483961343109,1.,-4.01172654187398));
#54004=CARTESIAN_POINT('Ctrl Pts',(1.06343586496236,-1.,-4.01940647495943));
#54005=CARTESIAN_POINT('Ctrl Pts',(1.06343586496236,1.,-4.01940647495943));
#54006=CARTESIAN_POINT('Ctrl Pts',(1.06199687787462,-1.,-4.02708855235633));
#54007=CARTESIAN_POINT('Ctrl Pts',(1.06199687787462,1.,-4.02708855235633));
#54008=CARTESIAN_POINT('Ctrl Pts',(1.06052284711857,-1.,-4.03477261141553));
#54009=CARTESIAN_POINT('Ctrl Pts',(1.06052284711857,1.,-4.03477261141553));
#54010=CARTESIAN_POINT('Ctrl Pts',(1.05901393666566,-1.,-4.04245854427496));
#54011=CARTESIAN_POINT('Ctrl Pts',(1.05901393666566,1.,-4.04245854427496));
#54012=CARTESIAN_POINT('Ctrl Pts',(1.05747027727959,-1.,-4.05014628384869));
#54013=CARTESIAN_POINT('Ctrl Pts',(1.05747027727959,1.,-4.05014628384869));
#54014=CARTESIAN_POINT('Ctrl Pts',(1.05620762707996,-1.,-4.05629789307025));
#54015=CARTESIAN_POINT('Ctrl Pts',(1.05620762707996,1.,-4.05629789307025));
#54016=CARTESIAN_POINT('Ctrl Pts',(1.05524507177599,-1.,-4.06091239149123));
#54017=CARTESIAN_POINT('Ctrl Pts',(1.05524507177599,1.,-4.06091239149123));
#54018=CARTESIAN_POINT('Ctrl Pts',(1.05459645194823,-1.,-4.06398907542249));
#54019=CARTESIAN_POINT('Ctrl Pts',(1.05459645194823,1.,-4.06398907542249));
#54020=CARTESIAN_POINT('Ctrl Pts',(1.05427041296137,-1.,-4.06552750530042));
#54021=CARTESIAN_POINT('Ctrl Pts',(1.05427041296137,1.,-4.06552750530042));
#54022=CARTESIAN_POINT('',(1.07167739962028,1.,-3.59360648251073));
#54023=CARTESIAN_POINT('Ctrl Pts',(1.07167739962028,-1.,-3.59360648251073));
#54024=CARTESIAN_POINT('Ctrl Pts',(1.07167739962028,-0.666666666666667,
-3.59360648251073));
#54025=CARTESIAN_POINT('Ctrl Pts',(1.07167739962028,-0.333333333333333,
-3.59360648251073));
#54026=CARTESIAN_POINT('Ctrl Pts',(1.07167739962028,0.333333333333333,-3.59360648251073));
#54027=CARTESIAN_POINT('Ctrl Pts',(1.07167739962028,0.666666666666667,-3.59360648251073));
#54028=CARTESIAN_POINT('Ctrl Pts',(1.07167739962028,1.,-3.59360648251073));
#54029=CARTESIAN_POINT('',(1.05427041296137,1.,-4.06552750530042));
#54030=CARTESIAN_POINT('',(1.05427041296137,0.,-4.06552750530042));
#54031=CARTESIAN_POINT('Ctrl Pts',(1.07167739962028,1.,-3.59360648251073));
#54032=CARTESIAN_POINT('Ctrl Pts',(1.07171709254135,1.,-3.5936351279798));
#54033=CARTESIAN_POINT('Ctrl Pts',(1.07183575450617,1.,-3.59379266874567));
#54034=CARTESIAN_POINT('Ctrl Pts',(1.07209229745229,1.,-3.59439596999862));
#54035=CARTESIAN_POINT('Ctrl Pts',(1.07259084660936,1.,-3.59600583194946));
#54036=CARTESIAN_POINT('Ctrl Pts',(1.07347372545714,1.,-3.59940121154535));
#54037=CARTESIAN_POINT('Ctrl Pts',(1.07469327168578,1.,-3.60456339887778));
#54038=CARTESIAN_POINT('Ctrl Pts',(1.07611545402734,1.,-3.61098481349204));
#54039=CARTESIAN_POINT('Ctrl Pts',(1.07764868137619,1.,-3.61832318504575));
#54040=CARTESIAN_POINT('Ctrl Pts',(1.07919137290742,1.,-3.62619537902361));
#54041=CARTESIAN_POINT('Ctrl Pts',(1.08064765719867,1.,-3.63423373196529));
#54042=CARTESIAN_POINT('Ctrl Pts',(1.08194278850996,1.,-3.64214167843677));
#54043=CARTESIAN_POINT('Ctrl Pts',(1.08304289898623,1.,-3.64976441208358));
#54044=CARTESIAN_POINT('Ctrl Pts',(1.08395671077807,1.,-3.65709649161166));
#54045=CARTESIAN_POINT('Ctrl Pts',(1.08471809922901,1.,-3.66422237895365));
#54046=CARTESIAN_POINT('Ctrl Pts',(1.0853733414449,1.,-3.67127347729666));
#54047=CARTESIAN_POINT('Ctrl Pts',(1.0859675575576,1.,-3.67838211685118));
#54048=CARTESIAN_POINT('Ctrl Pts',(1.0865288888259,1.,-3.68562817420797));
#54049=CARTESIAN_POINT('Ctrl Pts',(1.08706319540271,1.,-3.69302062410157));
#54050=CARTESIAN_POINT('Ctrl Pts',(1.08756311291309,1.,-3.70052690909833));
#54051=CARTESIAN_POINT('Ctrl Pts',(1.08801367312185,1.,-3.70809084139457));
#54052=CARTESIAN_POINT('Ctrl Pts',(1.0883988733478,1.,-3.71565372339075));
#54053=CARTESIAN_POINT('Ctrl Pts',(1.08870887220082,1.,-3.72317741369398));
#54054=CARTESIAN_POINT('Ctrl Pts',(1.08894337390937,1.,-3.73065515162988));
#54055=CARTESIAN_POINT('Ctrl Pts',(1.08910769013297,1.,-3.73809879348239));
#54056=CARTESIAN_POINT('Ctrl Pts',(1.08921040494017,1.,-3.74553121371757));
#54057=CARTESIAN_POINT('Ctrl Pts',(1.08926054632925,1.,-3.75297711748132));
#54058=CARTESIAN_POINT('Ctrl Pts',(1.08926462734281,1.,-3.76045342580208));
#54059=CARTESIAN_POINT('Ctrl Pts',(1.08922484204256,1.,-3.76796340094448));
#54060=CARTESIAN_POINT('Ctrl Pts',(1.0891407279127,1.,-3.77550199409424));
#54061=CARTESIAN_POINT('Ctrl Pts',(1.08901018614636,1.,-3.78305911299504));
#54062=CARTESIAN_POINT('Ctrl Pts',(1.08883071512098,1.,-3.79062357974404));
#54063=CARTESIAN_POINT('Ctrl Pts',(1.08860064435778,1.,-3.79818708705259));
#54064=CARTESIAN_POINT('Ctrl Pts',(1.0883200925538,1.,-3.8057472665766));
#54065=CARTESIAN_POINT('Ctrl Pts',(1.08799030610862,1.,-3.81330554446323));
#54066=CARTESIAN_POINT('Ctrl Pts',(1.08761321539442,1.,-3.82086569676319));
#54067=CARTESIAN_POINT('Ctrl Pts',(1.08719091307558,1.,-3.82843215316984));
#54068=CARTESIAN_POINT('Ctrl Pts',(1.08672515456902,1.,-3.83600837071708));
#54069=CARTESIAN_POINT('Ctrl Pts',(1.08621688337604,1.,-3.8435952876495));
#54070=CARTESIAN_POINT('Ctrl Pts',(1.08566647671844,1.,-3.85119211322755));
#54071=CARTESIAN_POINT('Ctrl Pts',(1.08507395120059,1.,-3.85879698702532));
#54072=CARTESIAN_POINT('Ctrl Pts',(1.08443918607927,1.,-3.86640769434274));
#54073=CARTESIAN_POINT('Ctrl Pts',(1.08376213307504,1.,-3.8740223372254));
#54074=CARTESIAN_POINT('Ctrl Pts',(1.08304304871028,1.,-3.88164007721313));
#54075=CARTESIAN_POINT('Ctrl Pts',(1.08228241999346,1.,-3.88926088975114));
#54076=CARTESIAN_POINT('Ctrl Pts',(1.08148086931358,1.,-3.8968852509835));
#54077=CARTESIAN_POINT('Ctrl Pts',(1.08063906483818,1.,-3.90451384092545));
#54078=CARTESIAN_POINT('Ctrl Pts',(1.07975763507473,1.,-3.91214726022143));
#54079=CARTESIAN_POINT('Ctrl Pts',(1.07883706663554,1.,-3.91978568924178));
#54080=CARTESIAN_POINT('Ctrl Pts',(1.07787771707195,1.,-3.9274289334984));
#54081=CARTESIAN_POINT('Ctrl Pts',(1.07687985975384,1.,-3.93507657572883));
#54082=CARTESIAN_POINT('Ctrl Pts',(1.07584371946443,1.,-3.94272809633331));
#54083=CARTESIAN_POINT('Ctrl Pts',(1.07476950921587,1.,-3.95038299600676));
#54084=CARTESIAN_POINT('Ctrl Pts',(1.07365747426491,1.,-3.95804094429373));
#54085=CARTESIAN_POINT('Ctrl Pts',(1.07250789943007,1.,-3.96570179322338));
#54086=CARTESIAN_POINT('Ctrl Pts',(1.07132109206164,1.,-3.9733655022223));
#54087=CARTESIAN_POINT('Ctrl Pts',(1.07009737257767,1.,-3.98103208801101));
#54088=CARTESIAN_POINT('Ctrl Pts',(1.06883706263941,1.,-3.98870156857412));
#54089=CARTESIAN_POINT('Ctrl Pts',(1.06754047381312,1.,-3.99637389920441));
#54090=CARTESIAN_POINT('Ctrl Pts',(1.06620789963606,1.,-4.00404894952579));
#54091=CARTESIAN_POINT('Ctrl Pts',(1.06483961343109,1.,-4.01172654187398));
#54092=CARTESIAN_POINT('Ctrl Pts',(1.06343586496236,1.,-4.01940647495943));
#54093=CARTESIAN_POINT('Ctrl Pts',(1.06199687787462,1.,-4.02708855235633));
#54094=CARTESIAN_POINT('Ctrl Pts',(1.06052284711857,1.,-4.03477261141553));
#54095=CARTESIAN_POINT('Ctrl Pts',(1.05901393666566,1.,-4.04245854427496));
#54096=CARTESIAN_POINT('Ctrl Pts',(1.05747027727959,1.,-4.05014628384869));
#54097=CARTESIAN_POINT('Ctrl Pts',(1.05620762707996,1.,-4.05629789307025));
#54098=CARTESIAN_POINT('Ctrl Pts',(1.05524507177599,1.,-4.06091239149123));
#54099=CARTESIAN_POINT('Ctrl Pts',(1.05459645194823,1.,-4.06398907542249));
#54100=CARTESIAN_POINT('Ctrl Pts',(1.05427041296137,1.,-4.06552750530042));
#54101=CARTESIAN_POINT('Origin',(1.05427041296137,0.,-4.06552750530042));
#54102=CARTESIAN_POINT('',(0.906349047628866,1.,-4.10104028313088));
#54103=CARTESIAN_POINT('Origin',(0.,0.,0.));
#54104=CARTESIAN_POINT('',(1.24526366418038,1.,-3.5372048861597));
#54105=CARTESIAN_POINT('Origin',(0.,1.,0.));
#54106=CARTESIAN_POINT('Ctrl Pts',(1.24526366418038,1.,-3.5372048861597));
#54107=CARTESIAN_POINT('Ctrl Pts',(1.24526366418038,0.666666666666667,-3.5372048861597));
#54108=CARTESIAN_POINT('Ctrl Pts',(1.24526366418038,0.333333333333333,-3.5372048861597));
#54109=CARTESIAN_POINT('Ctrl Pts',(1.24526366418038,-0.333333333333333,
-3.5372048861597));
#54110=CARTESIAN_POINT('Ctrl Pts',(1.24526366418038,-0.666666666666667,
-3.5372048861597));
#54111=CARTESIAN_POINT('Ctrl Pts',(1.24526366418038,-1.,-3.5372048861597));
#54112=CARTESIAN_POINT('Ctrl Pts',(1.53673442965256,-1.,-3.90876544355381));
#54113=CARTESIAN_POINT('Ctrl Pts',(1.53673442965256,1.,-3.90876544355381));
#54114=CARTESIAN_POINT('Ctrl Pts',(1.53556639217905,-1.,-3.90771246855019));
#54115=CARTESIAN_POINT('Ctrl Pts',(1.53556639217905,1.,-3.90771246855019));
#54116=CARTESIAN_POINT('Ctrl Pts',(1.53323321827755,-1.,-3.90560462813969));
#54117=CARTESIAN_POINT('Ctrl Pts',(1.53323321827755,1.,-3.90560462813969));
#54118=CARTESIAN_POINT('Ctrl Pts',(1.52974216056287,-1.,-3.90243719631596));
#54119=CARTESIAN_POINT('Ctrl Pts',(1.52974216056287,1.,-3.90243719631596));
#54120=CARTESIAN_POINT('Ctrl Pts',(1.52510482991635,-1.,-3.89820260708225));
#54121=CARTESIAN_POINT('Ctrl Pts',(1.52510482991635,1.,-3.89820260708225));
#54122=CARTESIAN_POINT('Ctrl Pts',(1.51933724329305,-1.,-3.89289043533657));
#54123=CARTESIAN_POINT('Ctrl Pts',(1.51933724329305,1.,-3.89289043533657));
#54124=CARTESIAN_POINT('Ctrl Pts',(1.51359883110559,-1.,-3.88755930033884));
#54125=CARTESIAN_POINT('Ctrl Pts',(1.51359883110559,1.,-3.88755930033884));
#54126=CARTESIAN_POINT('Ctrl Pts',(1.50788973857757,-1.,-3.88220917950538));
#54127=CARTESIAN_POINT('Ctrl Pts',(1.50788973857757,1.,-3.88220917950538));
#54128=CARTESIAN_POINT('Ctrl Pts',(1.50221016176556,-1.,-3.87684006372134));
#54129=CARTESIAN_POINT('Ctrl Pts',(1.50221016176556,1.,-3.87684006372134));
#54130=CARTESIAN_POINT('Ctrl Pts',(1.49656035399122,-1.,-3.87145196998465));
#54131=CARTESIAN_POINT('Ctrl Pts',(1.49656035399122,1.,-3.87145196998465));
#54132=CARTESIAN_POINT('Ctrl Pts',(1.4909406116431,-1.,-3.86604492575189));
#54133=CARTESIAN_POINT('Ctrl Pts',(1.4909406116431,1.,-3.86604492575189));
#54134=CARTESIAN_POINT('Ctrl Pts',(1.48535125509919,-1.,-3.86061894706087));
#54135=CARTESIAN_POINT('Ctrl Pts',(1.48535125509919,1.,-3.86061894706087));
#54136=CARTESIAN_POINT('Ctrl Pts',(1.4797926099102,-1.,-3.85517401698843));
#54137=CARTESIAN_POINT('Ctrl Pts',(1.4797926099102,1.,-3.85517401698843));
#54138=CARTESIAN_POINT('Ctrl Pts',(1.47426499018538,-1.,-3.84971006847277));
#54139=CARTESIAN_POINT('Ctrl Pts',(1.47426499018538,1.,-3.84971006847277));
#54140=CARTESIAN_POINT('Ctrl Pts',(1.46876867426504,-1.,-3.84422695454796));
#54141=CARTESIAN_POINT('Ctrl Pts',(1.46876867426504,1.,-3.84422695454796));
#54142=CARTESIAN_POINT('Ctrl Pts',(1.46330391180752,-1.,-3.83872447159639));
#54143=CARTESIAN_POINT('Ctrl Pts',(1.46330391180752,1.,-3.83872447159639));
#54144=CARTESIAN_POINT('Ctrl Pts',(1.45787095220852,-1.,-3.83320241775423));
#54145=CARTESIAN_POINT('Ctrl Pts',(1.45787095220852,1.,-3.83320241775423));
#54146=CARTESIAN_POINT('Ctrl Pts',(1.45247006796836,-1.,-3.82766064519075));
#54147=CARTESIAN_POINT('Ctrl Pts',(1.45247006796836,1.,-3.82766064519075));
#54148=CARTESIAN_POINT('Ctrl Pts',(1.44710157648539,-1.,-3.82209910620533));
#54149=CARTESIAN_POINT('Ctrl Pts',(1.44710157648539,1.,-3.82209910620533));
#54150=CARTESIAN_POINT('Ctrl Pts',(1.44176587041347,-1.,-3.81651792398414));
#54151=CARTESIAN_POINT('Ctrl Pts',(1.44176587041347,1.,-3.81651792398414));
#54152=CARTESIAN_POINT('Ctrl Pts',(1.43646341556724,-1.,-3.81091737726815));
#54153=CARTESIAN_POINT('Ctrl Pts',(1.43646341556724,1.,-3.81091737726815));
#54154=CARTESIAN_POINT('Ctrl Pts',(1.4311946992132,-1.,-3.80529775429805));
#54155=CARTESIAN_POINT('Ctrl Pts',(1.4311946992132,1.,-3.80529775429805));
#54156=CARTESIAN_POINT('Ctrl Pts',(1.42596018777283,-1.,-3.7996592319632));
#54157=CARTESIAN_POINT('Ctrl Pts',(1.42596018777283,1.,-3.7996592319632));
#54158=CARTESIAN_POINT('Ctrl Pts',(1.42076028482836,-1.,-3.79400175744408));
#54159=CARTESIAN_POINT('Ctrl Pts',(1.42076028482836,1.,-3.79400175744408));
#54160=CARTESIAN_POINT('Ctrl Pts',(1.4155952780383,-1.,-3.78832489879426));
#54161=CARTESIAN_POINT('Ctrl Pts',(1.4155952780383,1.,-3.78832489879426));
#54162=CARTESIAN_POINT('Ctrl Pts',(1.41046532282593,-1.,-3.78262780065471));
#54163=CARTESIAN_POINT('Ctrl Pts',(1.41046532282593,1.,-3.78262780065471));
#54164=CARTESIAN_POINT('Ctrl Pts',(1.40537056004722,-1.,-3.77690952014259));
#54165=CARTESIAN_POINT('Ctrl Pts',(1.40537056004722,1.,-3.77690952014259));
#54166=CARTESIAN_POINT('Ctrl Pts',(1.40031121335505,-1.,-3.77116930621827));
#54167=CARTESIAN_POINT('Ctrl Pts',(1.40031121335505,1.,-3.77116930621827));
#54168=CARTESIAN_POINT('Ctrl Pts',(1.39528769118052,-1.,-3.76540689249074));
#54169=CARTESIAN_POINT('Ctrl Pts',(1.39528769118052,1.,-3.76540689249074));
#54170=CARTESIAN_POINT('Ctrl Pts',(1.39030069388918,-1.,-3.75962280650855));
#54171=CARTESIAN_POINT('Ctrl Pts',(1.39030069388918,1.,-3.75962280650855));
#54172=CARTESIAN_POINT('Ctrl Pts',(1.38535129801176,-1.,-3.75381861212707));
#54173=CARTESIAN_POINT('Ctrl Pts',(1.38535129801176,1.,-3.75381861212707));
#54174=CARTESIAN_POINT('Ctrl Pts',(1.38044070763295,-1.,-3.74799617204729));
#54175=CARTESIAN_POINT('Ctrl Pts',(1.38044070763295,1.,-3.74799617204729));
#54176=CARTESIAN_POINT('Ctrl Pts',(1.37557002971687,-1.,-3.74215698162555));
#54177=CARTESIAN_POINT('Ctrl Pts',(1.37557002971687,1.,-3.74215698162555));
#54178=CARTESIAN_POINT('Ctrl Pts',(1.37074003422739,-1.,-3.7363014588581));
#54179=CARTESIAN_POINT('Ctrl Pts',(1.37074003422739,1.,-3.7363014588581));
#54180=CARTESIAN_POINT('Ctrl Pts',(1.36595093298676,-1.,-3.73042829011295));
#54181=CARTESIAN_POINT('Ctrl Pts',(1.36595093298676,1.,-3.73042829011295));
#54182=CARTESIAN_POINT('Ctrl Pts',(1.36120211416354,-1.,-3.72453364678279));
#54183=CARTESIAN_POINT('Ctrl Pts',(1.36120211416354,1.,-3.72453364678279));
#54184=CARTESIAN_POINT('Ctrl Pts',(1.35649266705037,-1.,-3.71861271513313));
#54185=CARTESIAN_POINT('Ctrl Pts',(1.35649266705037,1.,-3.71861271513313));
#54186=CARTESIAN_POINT('Ctrl Pts',(1.35182193384424,-1.,-3.71266130563054));
#54187=CARTESIAN_POINT('Ctrl Pts',(1.35182193384424,1.,-3.71266130563054));
#54188=CARTESIAN_POINT('Ctrl Pts',(1.34719008463534,-1.,-3.70667753188248));
#54189=CARTESIAN_POINT('Ctrl Pts',(1.34719008463534,1.,-3.70667753188248));
#54190=CARTESIAN_POINT('Ctrl Pts',(1.34259860752933,-1.,-3.70066324015119));
#54191=CARTESIAN_POINT('Ctrl Pts',(1.34259860752933,1.,-3.70066324015119));
#54192=CARTESIAN_POINT('Ctrl Pts',(1.33805103398219,-1.,-3.69462613305708));
#54193=CARTESIAN_POINT('Ctrl Pts',(1.33805103398219,1.,-3.69462613305708));
#54194=CARTESIAN_POINT('Ctrl Pts',(1.33355191034523,-1.,-3.68857672413033));
#54195=CARTESIAN_POINT('Ctrl Pts',(1.33355191034523,1.,-3.68857672413033));
#54196=CARTESIAN_POINT('Ctrl Pts',(1.3291054707274,-1.,-3.68252441182551));
#54197=CARTESIAN_POINT('Ctrl Pts',(1.3291054707274,1.,-3.68252441182551));
#54198=CARTESIAN_POINT('Ctrl Pts',(1.32471430856415,-1.,-3.67647355257912));
#54199=CARTESIAN_POINT('Ctrl Pts',(1.32471430856415,1.,-3.67647355257912));
#54200=CARTESIAN_POINT('Ctrl Pts',(1.32037828137766,-1.,-3.67042021752656));
#54201=CARTESIAN_POINT('Ctrl Pts',(1.32037828137766,1.,-3.67042021752656));
#54202=CARTESIAN_POINT('Ctrl Pts',(1.31609271239911,-1.,-3.66434688899793));
#54203=CARTESIAN_POINT('Ctrl Pts',(1.31609271239911,1.,-3.66434688899793));
#54204=CARTESIAN_POINT('Ctrl Pts',(1.31185038411218,-1.,-3.65822827358617));
#54205=CARTESIAN_POINT('Ctrl Pts',(1.31185038411218,1.,-3.65822827358617));
#54206=CARTESIAN_POINT('Ctrl Pts',(1.30764479590039,-1.,-3.65204081987068));
#54207=CARTESIAN_POINT('Ctrl Pts',(1.30764479590039,1.,-3.65204081987068));
#54208=CARTESIAN_POINT('Ctrl Pts',(1.30347327603774,-1.,-3.64577181380113));
#54209=CARTESIAN_POINT('Ctrl Pts',(1.30347327603774,1.,-3.64577181380113));
#54210=CARTESIAN_POINT('Ctrl Pts',(1.2993395590647,-1.,-3.63942689872808));
#54211=CARTESIAN_POINT('Ctrl Pts',(1.2993395590647,1.,-3.63942689872808));
#54212=CARTESIAN_POINT('Ctrl Pts',(1.29525810207762,-1.,-3.63304271631046));
#54213=CARTESIAN_POINT('Ctrl Pts',(1.29525810207762,1.,-3.63304271631046));
#54214=CARTESIAN_POINT('Ctrl Pts',(1.29125046021878,-1.,-3.62667616004369));
#54215=CARTESIAN_POINT('Ctrl Pts',(1.29125046021878,1.,-3.62667616004369));
#54216=CARTESIAN_POINT('Ctrl Pts',(1.28733755029384,-1.,-3.6203814849236));
#54217=CARTESIAN_POINT('Ctrl Pts',(1.28733755029384,1.,-3.6203814849236));
#54218=CARTESIAN_POINT('Ctrl Pts',(1.28353255117765,-1.,-3.61418935913823));
#54219=CARTESIAN_POINT('Ctrl Pts',(1.28353255117765,1.,-3.61418935913823));
#54220=CARTESIAN_POINT('Ctrl Pts',(1.27983492861691,-1.,-3.60808907746339));
#54221=CARTESIAN_POINT('Ctrl Pts',(1.27983492861691,1.,-3.60808907746339));
#54222=CARTESIAN_POINT('Ctrl Pts',(1.27622049908625,-1.,-3.60199947736298));
#54223=CARTESIAN_POINT('Ctrl Pts',(1.27622049908625,1.,-3.60199947736298));
#54224=CARTESIAN_POINT('Ctrl Pts',(1.27264798379307,-1.,-3.59578698050006));
#54225=CARTESIAN_POINT('Ctrl Pts',(1.27264798379307,1.,-3.59578698050006));
#54226=CARTESIAN_POINT('Ctrl Pts',(1.26907758484709,-1.,-3.58931807846313));
#54227=CARTESIAN_POINT('Ctrl Pts',(1.26907758484709,1.,-3.58931807846313));
#54228=CARTESIAN_POINT('Ctrl Pts',(1.26548706249862,-1.,-3.58250452868618));
#54229=CARTESIAN_POINT('Ctrl Pts',(1.26548706249862,1.,-3.58250452868618));
#54230=CARTESIAN_POINT('Ctrl Pts',(1.2618866714281,-1.,-3.5753456065171));
#54231=CARTESIAN_POINT('Ctrl Pts',(1.2618866714281,1.,-3.5753456065171));
#54232=CARTESIAN_POINT('Ctrl Pts',(1.25834000485716,-1.,-3.56798645995275));
#54233=CARTESIAN_POINT('Ctrl Pts',(1.25834000485716,1.,-3.56798645995275));
#54234=CARTESIAN_POINT('Ctrl Pts',(1.25496090900009,-1.,-3.56071094991199));
#54235=CARTESIAN_POINT('Ctrl Pts',(1.25496090900009,1.,-3.56071094991199));
#54236=CARTESIAN_POINT('Ctrl Pts',(1.2518879294064,-1.,-3.55387287418985));
#54237=CARTESIAN_POINT('Ctrl Pts',(1.2518879294064,1.,-3.55387287418985));
#54238=CARTESIAN_POINT('Ctrl Pts',(1.24926408628003,-1.,-3.54784190283068));
#54239=CARTESIAN_POINT('Ctrl Pts',(1.24926408628003,1.,-3.54784190283068));
#54240=CARTESIAN_POINT('Ctrl Pts',(1.24721646231966,-1.,-3.54294877425964));
#54241=CARTESIAN_POINT('Ctrl Pts',(1.24721646231966,1.,-3.54294877425964));
#54242=CARTESIAN_POINT('Ctrl Pts',(1.24583101679029,-1.,-3.53941798195825));
#54243=CARTESIAN_POINT('Ctrl Pts',(1.24583101679029,1.,-3.53941798195825));
#54244=CARTESIAN_POINT('Ctrl Pts',(1.24528461332987,-1.,-3.53776753802906));
#54245=CARTESIAN_POINT('Ctrl Pts',(1.24528461332987,1.,-3.53776753802906));
#54246=CARTESIAN_POINT('Ctrl Pts',(1.24519702335451,-1.,-3.53720633057798));
#54247=CARTESIAN_POINT('Ctrl Pts',(1.24519702335451,1.,-3.53720633057798));
#54248=CARTESIAN_POINT('Ctrl Pts',(1.24528174185098,-1.,-3.53713269667399));
#54249=CARTESIAN_POINT('Ctrl Pts',(1.24528174185098,1.,-3.53713269667399));
#54250=CARTESIAN_POINT('Ctrl Pts',(1.24535988127942,-1.,-3.53717101171257));
#54251=CARTESIAN_POINT('Ctrl Pts',(1.24535988127942,1.,-3.53717101171257));
#54252=CARTESIAN_POINT('',(1.53673442965256,1.,-3.90876544355381));
#54253=CARTESIAN_POINT('Ctrl Pts',(1.53673442965256,1.,-3.90876544355381));
#54254=CARTESIAN_POINT('Ctrl Pts',(1.53556639217905,1.,-3.90771246855019));
#54255=CARTESIAN_POINT('Ctrl Pts',(1.53323321827755,1.,-3.90560462813969));
#54256=CARTESIAN_POINT('Ctrl Pts',(1.52974216056287,1.,-3.90243719631596));
#54257=CARTESIAN_POINT('Ctrl Pts',(1.52510482991635,1.,-3.89820260708225));
#54258=CARTESIAN_POINT('Ctrl Pts',(1.51933724329305,1.,-3.89289043533657));
#54259=CARTESIAN_POINT('Ctrl Pts',(1.51359883110559,1.,-3.88755930033884));
#54260=CARTESIAN_POINT('Ctrl Pts',(1.50788973857757,1.,-3.88220917950538));
#54261=CARTESIAN_POINT('Ctrl Pts',(1.50221016176556,1.,-3.87684006372134));
#54262=CARTESIAN_POINT('Ctrl Pts',(1.49656035399122,1.,-3.87145196998465));
#54263=CARTESIAN_POINT('Ctrl Pts',(1.4909406116431,1.,-3.86604492575189));
#54264=CARTESIAN_POINT('Ctrl Pts',(1.48535125509919,1.,-3.86061894706087));
#54265=CARTESIAN_POINT('Ctrl Pts',(1.4797926099102,1.,-3.85517401698843));
#54266=CARTESIAN_POINT('Ctrl Pts',(1.47426499018538,1.,-3.84971006847277));
#54267=CARTESIAN_POINT('Ctrl Pts',(1.46876867426504,1.,-3.84422695454796));
#54268=CARTESIAN_POINT('Ctrl Pts',(1.46330391180752,1.,-3.83872447159639));
#54269=CARTESIAN_POINT('Ctrl Pts',(1.45787095220852,1.,-3.83320241775423));
#54270=CARTESIAN_POINT('Ctrl Pts',(1.45247006796836,1.,-3.82766064519075));
#54271=CARTESIAN_POINT('Ctrl Pts',(1.44710157648539,1.,-3.82209910620533));
#54272=CARTESIAN_POINT('Ctrl Pts',(1.44176587041347,1.,-3.81651792398414));
#54273=CARTESIAN_POINT('Ctrl Pts',(1.43646341556724,1.,-3.81091737726815));
#54274=CARTESIAN_POINT('Ctrl Pts',(1.4311946992132,1.,-3.80529775429805));
#54275=CARTESIAN_POINT('Ctrl Pts',(1.42596018777283,1.,-3.7996592319632));
#54276=CARTESIAN_POINT('Ctrl Pts',(1.42076028482836,1.,-3.79400175744408));
#54277=CARTESIAN_POINT('Ctrl Pts',(1.4155952780383,1.,-3.78832489879426));
#54278=CARTESIAN_POINT('Ctrl Pts',(1.41046532282593,1.,-3.78262780065471));
#54279=CARTESIAN_POINT('Ctrl Pts',(1.40537056004722,1.,-3.77690952014259));
#54280=CARTESIAN_POINT('Ctrl Pts',(1.40031121335505,1.,-3.77116930621827));
#54281=CARTESIAN_POINT('Ctrl Pts',(1.39528769118052,1.,-3.76540689249074));
#54282=CARTESIAN_POINT('Ctrl Pts',(1.39030069388918,1.,-3.75962280650855));
#54283=CARTESIAN_POINT('Ctrl Pts',(1.38535129801176,1.,-3.75381861212707));
#54284=CARTESIAN_POINT('Ctrl Pts',(1.38044070763295,1.,-3.74799617204729));
#54285=CARTESIAN_POINT('Ctrl Pts',(1.37557002971687,1.,-3.74215698162555));
#54286=CARTESIAN_POINT('Ctrl Pts',(1.37074003422739,1.,-3.7363014588581));
#54287=CARTESIAN_POINT('Ctrl Pts',(1.36595093298676,1.,-3.73042829011295));
#54288=CARTESIAN_POINT('Ctrl Pts',(1.36120211416354,1.,-3.72453364678279));
#54289=CARTESIAN_POINT('Ctrl Pts',(1.35649266705037,1.,-3.71861271513313));
#54290=CARTESIAN_POINT('Ctrl Pts',(1.35182193384424,1.,-3.71266130563054));
#54291=CARTESIAN_POINT('Ctrl Pts',(1.34719008463534,1.,-3.70667753188248));
#54292=CARTESIAN_POINT('Ctrl Pts',(1.34259860752933,1.,-3.70066324015119));
#54293=CARTESIAN_POINT('Ctrl Pts',(1.33805103398219,1.,-3.69462613305708));
#54294=CARTESIAN_POINT('Ctrl Pts',(1.33355191034523,1.,-3.68857672413033));
#54295=CARTESIAN_POINT('Ctrl Pts',(1.3291054707274,1.,-3.68252441182551));
#54296=CARTESIAN_POINT('Ctrl Pts',(1.32471430856415,1.,-3.67647355257912));
#54297=CARTESIAN_POINT('Ctrl Pts',(1.32037828137766,1.,-3.67042021752656));
#54298=CARTESIAN_POINT('Ctrl Pts',(1.31609271239911,1.,-3.66434688899793));
#54299=CARTESIAN_POINT('Ctrl Pts',(1.31185038411218,1.,-3.65822827358617));
#54300=CARTESIAN_POINT('Ctrl Pts',(1.30764479590039,1.,-3.65204081987068));
#54301=CARTESIAN_POINT('Ctrl Pts',(1.30347327603774,1.,-3.64577181380113));
#54302=CARTESIAN_POINT('Ctrl Pts',(1.2993395590647,1.,-3.63942689872808));
#54303=CARTESIAN_POINT('Ctrl Pts',(1.29525810207762,1.,-3.63304271631046));
#54304=CARTESIAN_POINT('Ctrl Pts',(1.29125046021878,1.,-3.62667616004369));
#54305=CARTESIAN_POINT('Ctrl Pts',(1.28733755029384,1.,-3.6203814849236));
#54306=CARTESIAN_POINT('Ctrl Pts',(1.28353255117765,1.,-3.61418935913823));
#54307=CARTESIAN_POINT('Ctrl Pts',(1.27983492861691,1.,-3.60808907746339));
#54308=CARTESIAN_POINT('Ctrl Pts',(1.27622049908625,1.,-3.60199947736298));
#54309=CARTESIAN_POINT('Ctrl Pts',(1.27264798379307,1.,-3.59578698050006));
#54310=CARTESIAN_POINT('Ctrl Pts',(1.26907758484709,1.,-3.58931807846313));
#54311=CARTESIAN_POINT('Ctrl Pts',(1.26548706249862,1.,-3.58250452868618));
#54312=CARTESIAN_POINT('Ctrl Pts',(1.2618866714281,1.,-3.5753456065171));
#54313=CARTESIAN_POINT('Ctrl Pts',(1.25834000485716,1.,-3.56798645995275));
#54314=CARTESIAN_POINT('Ctrl Pts',(1.25496090900009,1.,-3.56071094991199));
#54315=CARTESIAN_POINT('Ctrl Pts',(1.2518879294064,1.,-3.55387287418985));
#54316=CARTESIAN_POINT('Ctrl Pts',(1.24926408628003,1.,-3.54784190283068));
#54317=CARTESIAN_POINT('Ctrl Pts',(1.24721646231966,1.,-3.54294877425964));
#54318=CARTESIAN_POINT('Ctrl Pts',(1.24593497226008,1.,-3.53968291130022));
#54319=CARTESIAN_POINT('Ctrl Pts',(1.24539205388767,1.,-3.53808746578196));
#54320=CARTESIAN_POINT('Ctrl Pts',(1.2452449899111,1.,-3.5374485926552));
#54321=CARTESIAN_POINT('Ctrl Pts',(1.24524838931757,1.,-3.53725139174486));
#54322=CARTESIAN_POINT('Ctrl Pts',(1.24526366418038,1.,-3.5372048861597));
#54323=CARTESIAN_POINT('',(1.53673442965256,0.,-3.90876544355381));
#54324=CARTESIAN_POINT('Ctrl Pts',(1.62055519152809,-1.,-3.38176002566879));
#54325=CARTESIAN_POINT('Ctrl Pts',(1.62055519152809,1.,-3.38176002566879));
#54326=CARTESIAN_POINT('Ctrl Pts',(1.62058335162482,-1.,-3.38167767992676));
#54327=CARTESIAN_POINT('Ctrl Pts',(1.62058335162482,1.,-3.38167767992676));
#54328=CARTESIAN_POINT('Ctrl Pts',(1.62069532368199,-1.,-3.38166984193836));
#54329=CARTESIAN_POINT('Ctrl Pts',(1.62069532368199,1.,-3.38166984193836));
#54330=CARTESIAN_POINT('Ctrl Pts',(1.62103022181151,-1.,-3.38212861099984));
#54331=CARTESIAN_POINT('Ctrl Pts',(1.62103022181151,1.,-3.38212861099984));
#54332=CARTESIAN_POINT('Ctrl Pts',(1.62181089631344,-1.,-3.38368201668574));
#54333=CARTESIAN_POINT('Ctrl Pts',(1.62181089631344,1.,-3.38368201668574));
#54334=CARTESIAN_POINT('Ctrl Pts',(1.6233278855625,-1.,-3.38715832179072));
#54335=CARTESIAN_POINT('Ctrl Pts',(1.6233278855625,1.,-3.38715832179072));
#54336=CARTESIAN_POINT('Ctrl Pts',(1.62533996116713,-1.,-3.39206617496906));
#54337=CARTESIAN_POINT('Ctrl Pts',(1.62533996116713,1.,-3.39206617496906));
#54338=CARTESIAN_POINT('Ctrl Pts',(1.62774916464408,-1.,-3.39818605297991));
#54339=CARTESIAN_POINT('Ctrl Pts',(1.62774916464408,1.,-3.39818605297991));
#54340=CARTESIAN_POINT('Ctrl Pts',(1.63041148964828,-1.,-3.40519422740235));
#54341=CARTESIAN_POINT('Ctrl Pts',(1.63041148964828,1.,-3.40519422740235));
#54342=CARTESIAN_POINT('Ctrl Pts',(1.63316667054044,-1.,-3.41272817148478));
#54343=CARTESIAN_POINT('Ctrl Pts',(1.63316667054044,1.,-3.41272817148478));
#54344=CARTESIAN_POINT('Ctrl Pts',(1.63586250099773,-1.,-3.42043974590882));
#54345=CARTESIAN_POINT('Ctrl Pts',(1.63586250099773,1.,-3.42043974590882));
#54346=CARTESIAN_POINT('Ctrl Pts',(1.63837876246926,-1.,-3.42804772926291));
#54347=CARTESIAN_POINT('Ctrl Pts',(1.63837876246926,1.,-3.42804772926291));
#54348=CARTESIAN_POINT('Ctrl Pts',(1.64065778702023,-1.,-3.43540451921548));
#54349=CARTESIAN_POINT('Ctrl Pts',(1.64065778702023,1.,-3.43540451921548));
#54350=CARTESIAN_POINT('Ctrl Pts',(1.64270733821113,-1.,-3.44250337701888));
#54351=CARTESIAN_POINT('Ctrl Pts',(1.64270733821113,1.,-3.44250337701888));
#54352=CARTESIAN_POINT('Ctrl Pts',(1.64457408708107,-1.,-3.44942242546795));
#54353=CARTESIAN_POINT('Ctrl Pts',(1.64457408708107,1.,-3.44942242546795));
#54354=CARTESIAN_POINT('Ctrl Pts',(1.64632429697521,-1.,-3.45628421062422));
#54355=CARTESIAN_POINT('Ctrl Pts',(1.64632429697521,1.,-3.45628421062422));
#54356=CARTESIAN_POINT('Ctrl Pts',(1.64802323352738,-1.,-3.46321237515));
#54357=CARTESIAN_POINT('Ctrl Pts',(1.64802323352738,1.,-3.46321237515));
#54358=CARTESIAN_POINT('Ctrl Pts',(1.64971118698256,-1.,-3.47028140995992));
#54359=CARTESIAN_POINT('Ctrl Pts',(1.64971118698256,1.,-3.47028140995992));
#54360=CARTESIAN_POINT('Ctrl Pts',(1.65139534930322,-1.,-3.47749926256476));
#54361=CARTESIAN_POINT('Ctrl Pts',(1.65139534930322,1.,-3.47749926256476));
#54362=CARTESIAN_POINT('Ctrl Pts',(1.65306335367739,-1.,-3.48483492840894));
#54363=CARTESIAN_POINT('Ctrl Pts',(1.65306335367739,1.,-3.48483492840894));
#54364=CARTESIAN_POINT('Ctrl Pts',(1.65469162644468,-1.,-3.49223525300176));
#54365=CARTESIAN_POINT('Ctrl Pts',(1.65469162644468,1.,-3.49223525300176));
#54366=CARTESIAN_POINT('Ctrl Pts',(1.65625517961588,-1.,-3.4996447647794));
#54367=CARTESIAN_POINT('Ctrl Pts',(1.65625517961588,1.,-3.4996447647794));
#54368=CARTESIAN_POINT('Ctrl Pts',(1.65773832633632,-1.,-3.50702733146542));
#54369=CARTESIAN_POINT('Ctrl Pts',(1.65773832633632,1.,-3.50702733146542));
#54370=CARTESIAN_POINT('Ctrl Pts',(1.65913971687342,-1.,-3.5143763218894));
#54371=CARTESIAN_POINT('Ctrl Pts',(1.65913971687342,1.,-3.5143763218894));
#54372=CARTESIAN_POINT('Ctrl Pts',(1.66046645222279,-1.,-3.52170261543816));
#54373=CARTESIAN_POINT('Ctrl Pts',(1.66046645222279,1.,-3.52170261543816));
#54374=CARTESIAN_POINT('Ctrl Pts',(1.66173058912371,-1.,-3.52902746211093));
#54375=CARTESIAN_POINT('Ctrl Pts',(1.66173058912371,1.,-3.52902746211093));
#54376=CARTESIAN_POINT('Ctrl Pts',(1.66294490916111,-1.,-3.5363738506022));
#54377=CARTESIAN_POINT('Ctrl Pts',(1.66294490916111,1.,-3.5363738506022));
#54378=CARTESIAN_POINT('Ctrl Pts',(1.66411849222326,-1.,-3.54375747475014));
#54379=CARTESIAN_POINT('Ctrl Pts',(1.66411849222326,1.,-3.54375747475014));
#54380=CARTESIAN_POINT('Ctrl Pts',(1.66525401568994,-1.,-3.55118121342861));
#54381=CARTESIAN_POINT('Ctrl Pts',(1.66525401568994,1.,-3.55118121342861));
#54382=CARTESIAN_POINT('Ctrl Pts',(1.66635023293114,-1.,-3.55864015233602));
#54383=CARTESIAN_POINT('Ctrl Pts',(1.66635023293114,1.,-3.55864015233602));
#54384=CARTESIAN_POINT('Ctrl Pts',(1.66740349220305,-1.,-3.56612465179422));
#54385=CARTESIAN_POINT('Ctrl Pts',(1.66740349220305,1.,-3.56612465179422));
#54386=CARTESIAN_POINT('Ctrl Pts',(1.668409574073,-1.,-3.57362406285887));
#54387=CARTESIAN_POINT('Ctrl Pts',(1.668409574073,1.,-3.57362406285887));
#54388=CARTESIAN_POINT('Ctrl Pts',(1.66936552908232,-1.,-3.58113044183829));
#54389=CARTESIAN_POINT('Ctrl Pts',(1.66936552908232,1.,-3.58113044183829));
#54390=CARTESIAN_POINT('Ctrl Pts',(1.67027110397604,-1.,-3.58864143097834));
#54391=CARTESIAN_POINT('Ctrl Pts',(1.67027110397604,1.,-3.58864143097834));
#54392=CARTESIAN_POINT('Ctrl Pts',(1.67112775290707,-1.,-3.59615824388807));
#54393=CARTESIAN_POINT('Ctrl Pts',(1.67112775290707,1.,-3.59615824388807));
#54394=CARTESIAN_POINT('Ctrl Pts',(1.67193797318597,-1.,-3.60368430815201));
#54395=CARTESIAN_POINT('Ctrl Pts',(1.67193797318597,1.,-3.60368430815201));
#54396=CARTESIAN_POINT('Ctrl Pts',(1.67270452466968,-1.,-3.61122367156181));
#54397=CARTESIAN_POINT('Ctrl Pts',(1.67270452466968,1.,-3.61122367156181));
#54398=CARTESIAN_POINT('Ctrl Pts',(1.67342968196224,-1.,-3.61877947398184));
#54399=CARTESIAN_POINT('Ctrl Pts',(1.67342968196224,1.,-3.61877947398184));
#54400=CARTESIAN_POINT('Ctrl Pts',(1.67411452372271,-1.,-3.62635249450923));
#54401=CARTESIAN_POINT('Ctrl Pts',(1.67411452372271,1.,-3.62635249450923));
#54402=CARTESIAN_POINT('Ctrl Pts',(1.67475929882971,-1.,-3.63394189312924));
#54403=CARTESIAN_POINT('Ctrl Pts',(1.67475929882971,1.,-3.63394189312924));
#54404=CARTESIAN_POINT('Ctrl Pts',(1.67536373264848,-1.,-3.6415458297234));
#54405=CARTESIAN_POINT('Ctrl Pts',(1.67536373264848,1.,-3.6415458297234));
#54406=CARTESIAN_POINT('Ctrl Pts',(1.67592735946692,-1.,-3.64916213574667));
#54407=CARTESIAN_POINT('Ctrl Pts',(1.67592735946692,1.,-3.64916213574667));
#54408=CARTESIAN_POINT('Ctrl Pts',(1.67644983469449,-1.,-3.6567889441642));
#54409=CARTESIAN_POINT('Ctrl Pts',(1.67644983469449,1.,-3.6567889441642));
#54410=CARTESIAN_POINT('Ctrl Pts',(1.67693128053132,-1.,-3.66442538670968));
#54411=CARTESIAN_POINT('Ctrl Pts',(1.67693128053132,1.,-3.66442538670968));
#54412=CARTESIAN_POINT('Ctrl Pts',(1.67737217414874,-1.,-3.67207136294575));
#54413=CARTESIAN_POINT('Ctrl Pts',(1.67737217414874,1.,-3.67207136294575));
#54414=CARTESIAN_POINT('Ctrl Pts',(1.67777320475848,-1.,-3.67972724579124));
#54415=CARTESIAN_POINT('Ctrl Pts',(1.67777320475848,1.,-3.67972724579124));
#54416=CARTESIAN_POINT('Ctrl Pts',(1.67813513867965,-1.,-3.68739360236487));
#54417=CARTESIAN_POINT('Ctrl Pts',(1.67813513867965,1.,-3.68739360236487));
#54418=CARTESIAN_POINT('Ctrl Pts',(1.67845869064323,-1.,-3.6950709275959));
#54419=CARTESIAN_POINT('Ctrl Pts',(1.67845869064323,1.,-3.6950709275959));
#54420=CARTESIAN_POINT('Ctrl Pts',(1.67874436948667,-1.,-3.70275932351108));
#54421=CARTESIAN_POINT('Ctrl Pts',(1.67874436948667,1.,-3.70275932351108));
#54422=CARTESIAN_POINT('Ctrl Pts',(1.67899249793462,-1.,-3.71045854208343));
#54423=CARTESIAN_POINT('Ctrl Pts',(1.67899249793462,1.,-3.71045854208343));
#54424=CARTESIAN_POINT('Ctrl Pts',(1.67920328071708,-1.,-3.71816812842322));
#54425=CARTESIAN_POINT('Ctrl Pts',(1.67920328071708,1.,-3.71816812842322));
#54426=CARTESIAN_POINT('Ctrl Pts',(1.67937685856652,-1.,-3.72588753416396));
#54427=CARTESIAN_POINT('Ctrl Pts',(1.67937685856652,1.,-3.72588753416396));
#54428=CARTESIAN_POINT('Ctrl Pts',(1.67951336376402,-1.,-3.73361623282543));
#54429=CARTESIAN_POINT('Ctrl Pts',(1.67951336376402,1.,-3.73361623282543));
#54430=CARTESIAN_POINT('Ctrl Pts',(1.6796129868522,-1.,-3.74135385965401));
#54431=CARTESIAN_POINT('Ctrl Pts',(1.6796129868522,1.,-3.74135385965401));
#54432=CARTESIAN_POINT('Ctrl Pts',(1.67967598599525,-1.,-3.7491002239452));
#54433=CARTESIAN_POINT('Ctrl Pts',(1.67967598599525,1.,-3.7491002239452));
#54434=CARTESIAN_POINT('Ctrl Pts',(1.67970265841239,-1.,-3.75685523754493));
#54435=CARTESIAN_POINT('Ctrl Pts',(1.67970265841239,1.,-3.75685523754493));
#54436=CARTESIAN_POINT('Ctrl Pts',(1.67969332319245,-1.,-3.76461886684344));
#54437=CARTESIAN_POINT('Ctrl Pts',(1.67969332319245,1.,-3.76461886684344));
#54438=CARTESIAN_POINT('Ctrl Pts',(1.67964830084993,-1.,-3.77239107928502));
#54439=CARTESIAN_POINT('Ctrl Pts',(1.67964830084993,1.,-3.77239107928502));
#54440=CARTESIAN_POINT('Ctrl Pts',(1.67956789212141,-1.,-3.78017178197317));
#54441=CARTESIAN_POINT('Ctrl Pts',(1.67956789212141,1.,-3.78017178197317));
#54442=CARTESIAN_POINT('Ctrl Pts',(1.67945236653493,-1.,-3.7879608002176));
#54443=CARTESIAN_POINT('Ctrl Pts',(1.67945236653493,1.,-3.7879608002176));
#54444=CARTESIAN_POINT('Ctrl Pts',(1.67930196625548,-1.,-3.79575791578424));
#54445=CARTESIAN_POINT('Ctrl Pts',(1.67930196625548,1.,-3.79575791578424));
#54446=CARTESIAN_POINT('Ctrl Pts',(1.67911690648355,-1.,-3.80356289079005));
#54447=CARTESIAN_POINT('Ctrl Pts',(1.67911690648355,1.,-3.80356289079005));
#54448=CARTESIAN_POINT('Ctrl Pts',(1.6788973773827,-1.,-3.81137549624179));
#54449=CARTESIAN_POINT('Ctrl Pts',(1.6788973773827,1.,-3.81137549624179));
#54450=CARTESIAN_POINT('Ctrl Pts',(1.67864354605954,-1.,-3.81919554099578));
#54451=CARTESIAN_POINT('Ctrl Pts',(1.67864354605954,1.,-3.81919554099578));
#54452=CARTESIAN_POINT('Ctrl Pts',(1.6783555575934,-1.,-3.82702289286713));
#54453=CARTESIAN_POINT('Ctrl Pts',(1.6783555575934,1.,-3.82702289286713));
#54454=CARTESIAN_POINT('Ctrl Pts',(1.67803353064351,-1.,-3.8348574651399));
#54455=CARTESIAN_POINT('Ctrl Pts',(1.67803353064351,1.,-3.8348574651399));
#54456=CARTESIAN_POINT('Ctrl Pts',(1.67774874946079,-1.,-3.84113085985244));
#54457=CARTESIAN_POINT('Ctrl Pts',(1.67774874946079,1.,-3.84113085985244));
#54458=CARTESIAN_POINT('Ctrl Pts',(1.6775199114018,-1.,-3.84583912296459));
#54459=CARTESIAN_POINT('Ctrl Pts',(1.6775199114018,1.,-3.84583912296459));
#54460=CARTESIAN_POINT('Ctrl Pts',(1.67736057656533,-1.,-3.84897939430696));
#54461=CARTESIAN_POINT('Ctrl Pts',(1.67736057656533,1.,-3.84897939430696));
#54462=CARTESIAN_POINT('Ctrl Pts',(1.67727921511438,-1.,-3.85054988729471));
#54463=CARTESIAN_POINT('Ctrl Pts',(1.67727921511438,1.,-3.85054988729471));
#54464=CARTESIAN_POINT('',(1.62064718014094,1.,-3.38171594275765));
#54465=CARTESIAN_POINT('Ctrl Pts',(1.62064718014093,-1.,-3.38171594275765));
#54466=CARTESIAN_POINT('Ctrl Pts',(1.62064718014093,-0.666666666666667,
-3.38171594275765));
#54467=CARTESIAN_POINT('Ctrl Pts',(1.62064718014093,-0.333333333333333,
-3.38171594275765));
#54468=CARTESIAN_POINT('Ctrl Pts',(1.62064718014093,0.333333333333333,-3.38171594275765));
#54469=CARTESIAN_POINT('Ctrl Pts',(1.62064718014093,0.666666666666667,-3.38171594275765));
#54470=CARTESIAN_POINT('Ctrl Pts',(1.62064718014093,1.,-3.38171594275765));
#54471=CARTESIAN_POINT('',(1.67727921511438,1.,-3.85054988729471));
#54472=CARTESIAN_POINT('',(1.67727921511438,0.,-3.85054988729471));
#54473=CARTESIAN_POINT('Ctrl Pts',(1.62064718014094,1.,-3.38171594275765));
#54474=CARTESIAN_POINT('Ctrl Pts',(1.62069086551492,1.,-3.38173802621259));
#54475=CARTESIAN_POINT('Ctrl Pts',(1.62083271135947,1.,-3.38187506456922));
#54476=CARTESIAN_POINT('Ctrl Pts',(1.62118047294498,1.,-3.38243080602409));
#54477=CARTESIAN_POINT('Ctrl Pts',(1.62192472202769,1.,-3.38394285763222));
#54478=CARTESIAN_POINT('Ctrl Pts',(1.6233278855625,1.,-3.38715832179072));
#54479=CARTESIAN_POINT('Ctrl Pts',(1.62533996116713,1.,-3.39206617496906));
#54480=CARTESIAN_POINT('Ctrl Pts',(1.62774916464408,1.,-3.39818605297991));
#54481=CARTESIAN_POINT('Ctrl Pts',(1.63041148964828,1.,-3.40519422740235));
#54482=CARTESIAN_POINT('Ctrl Pts',(1.63316667054044,1.,-3.41272817148478));
#54483=CARTESIAN_POINT('Ctrl Pts',(1.63586250099773,1.,-3.42043974590882));
#54484=CARTESIAN_POINT('Ctrl Pts',(1.63837876246926,1.,-3.42804772926291));
#54485=CARTESIAN_POINT('Ctrl Pts',(1.64065778702023,1.,-3.43540451921548));
#54486=CARTESIAN_POINT('Ctrl Pts',(1.64270733821113,1.,-3.44250337701888));
#54487=CARTESIAN_POINT('Ctrl Pts',(1.64457408708107,1.,-3.44942242546795));
#54488=CARTESIAN_POINT('Ctrl Pts',(1.64632429697521,1.,-3.45628421062422));
#54489=CARTESIAN_POINT('Ctrl Pts',(1.64802323352738,1.,-3.46321237515));
#54490=CARTESIAN_POINT('Ctrl Pts',(1.64971118698256,1.,-3.47028140995992));
#54491=CARTESIAN_POINT('Ctrl Pts',(1.65139534930322,1.,-3.47749926256476));
#54492=CARTESIAN_POINT('Ctrl Pts',(1.65306335367739,1.,-3.48483492840894));
#54493=CARTESIAN_POINT('Ctrl Pts',(1.65469162644468,1.,-3.49223525300176));
#54494=CARTESIAN_POINT('Ctrl Pts',(1.65625517961588,1.,-3.4996447647794));
#54495=CARTESIAN_POINT('Ctrl Pts',(1.65773832633632,1.,-3.50702733146542));
#54496=CARTESIAN_POINT('Ctrl Pts',(1.65913971687342,1.,-3.5143763218894));
#54497=CARTESIAN_POINT('Ctrl Pts',(1.66046645222279,1.,-3.52170261543816));
#54498=CARTESIAN_POINT('Ctrl Pts',(1.66173058912371,1.,-3.52902746211093));
#54499=CARTESIAN_POINT('Ctrl Pts',(1.66294490916111,1.,-3.5363738506022));
#54500=CARTESIAN_POINT('Ctrl Pts',(1.66411849222326,1.,-3.54375747475014));
#54501=CARTESIAN_POINT('Ctrl Pts',(1.66525401568994,1.,-3.55118121342861));
#54502=CARTESIAN_POINT('Ctrl Pts',(1.66635023293114,1.,-3.55864015233602));
#54503=CARTESIAN_POINT('Ctrl Pts',(1.66740349220305,1.,-3.56612465179422));
#54504=CARTESIAN_POINT('Ctrl Pts',(1.668409574073,1.,-3.57362406285887));
#54505=CARTESIAN_POINT('Ctrl Pts',(1.66936552908232,1.,-3.58113044183829));
#54506=CARTESIAN_POINT('Ctrl Pts',(1.67027110397604,1.,-3.58864143097834));
#54507=CARTESIAN_POINT('Ctrl Pts',(1.67112775290707,1.,-3.59615824388807));
#54508=CARTESIAN_POINT('Ctrl Pts',(1.67193797318597,1.,-3.60368430815201));
#54509=CARTESIAN_POINT('Ctrl Pts',(1.67270452466968,1.,-3.61122367156181));
#54510=CARTESIAN_POINT('Ctrl Pts',(1.67342968196224,1.,-3.61877947398184));
#54511=CARTESIAN_POINT('Ctrl Pts',(1.67411452372271,1.,-3.62635249450923));
#54512=CARTESIAN_POINT('Ctrl Pts',(1.67475929882971,1.,-3.63394189312924));
#54513=CARTESIAN_POINT('Ctrl Pts',(1.67536373264848,1.,-3.6415458297234));
#54514=CARTESIAN_POINT('Ctrl Pts',(1.67592735946692,1.,-3.64916213574667));
#54515=CARTESIAN_POINT('Ctrl Pts',(1.67644983469449,1.,-3.6567889441642));
#54516=CARTESIAN_POINT('Ctrl Pts',(1.67693128053132,1.,-3.66442538670968));
#54517=CARTESIAN_POINT('Ctrl Pts',(1.67737217414874,1.,-3.67207136294575));
#54518=CARTESIAN_POINT('Ctrl Pts',(1.67777320475848,1.,-3.67972724579124));
#54519=CARTESIAN_POINT('Ctrl Pts',(1.67813513867965,1.,-3.68739360236487));
#54520=CARTESIAN_POINT('Ctrl Pts',(1.67845869064323,1.,-3.6950709275959));
#54521=CARTESIAN_POINT('Ctrl Pts',(1.67874436948667,1.,-3.70275932351108));
#54522=CARTESIAN_POINT('Ctrl Pts',(1.67899249793462,1.,-3.71045854208343));
#54523=CARTESIAN_POINT('Ctrl Pts',(1.67920328071708,1.,-3.71816812842322));
#54524=CARTESIAN_POINT('Ctrl Pts',(1.67937685856652,1.,-3.72588753416396));
#54525=CARTESIAN_POINT('Ctrl Pts',(1.67951336376402,1.,-3.73361623282543));
#54526=CARTESIAN_POINT('Ctrl Pts',(1.6796129868522,1.,-3.74135385965401));
#54527=CARTESIAN_POINT('Ctrl Pts',(1.67967598599525,1.,-3.7491002239452));
#54528=CARTESIAN_POINT('Ctrl Pts',(1.67970265841239,1.,-3.75685523754493));
#54529=CARTESIAN_POINT('Ctrl Pts',(1.67969332319245,1.,-3.76461886684344));
#54530=CARTESIAN_POINT('Ctrl Pts',(1.67964830084993,1.,-3.77239107928502));
#54531=CARTESIAN_POINT('Ctrl Pts',(1.67956789212141,1.,-3.78017178197317));
#54532=CARTESIAN_POINT('Ctrl Pts',(1.67945236653493,1.,-3.7879608002176));
#54533=CARTESIAN_POINT('Ctrl Pts',(1.67930196625548,1.,-3.79575791578424));
#54534=CARTESIAN_POINT('Ctrl Pts',(1.67911690648355,1.,-3.80356289079005));
#54535=CARTESIAN_POINT('Ctrl Pts',(1.6788973773827,1.,-3.81137549624179));
#54536=CARTESIAN_POINT('Ctrl Pts',(1.67864354605954,1.,-3.81919554099578));
#54537=CARTESIAN_POINT('Ctrl Pts',(1.6783555575934,1.,-3.82702289286713));
#54538=CARTESIAN_POINT('Ctrl Pts',(1.67803353064351,1.,-3.8348574651399));
#54539=CARTESIAN_POINT('Ctrl Pts',(1.67774874946079,1.,-3.84113085985244));
#54540=CARTESIAN_POINT('Ctrl Pts',(1.6775199114018,1.,-3.84583912296459));
#54541=CARTESIAN_POINT('Ctrl Pts',(1.67736057656533,1.,-3.84897939430696));
#54542=CARTESIAN_POINT('Ctrl Pts',(1.67727921511438,1.,-3.85054988729471));
#54543=CARTESIAN_POINT('Origin',(1.67727921511438,0.,-3.85054988729471));
#54544=CARTESIAN_POINT('',(1.53673442965256,1.,-3.90876544355381));
#54545=CARTESIAN_POINT('Origin',(0.,0.,0.));
#54546=CARTESIAN_POINT('',(1.78327315618183,1.,-3.29885386921599));
#54547=CARTESIAN_POINT('Origin',(0.,1.,0.));
#54548=CARTESIAN_POINT('Ctrl Pts',(1.78327315618183,1.,-3.29885386921599));
#54549=CARTESIAN_POINT('Ctrl Pts',(1.78327315618183,0.666666666666667,-3.29885386921599));
#54550=CARTESIAN_POINT('Ctrl Pts',(1.78327315618183,0.333333333333333,-3.29885386921599));
#54551=CARTESIAN_POINT('Ctrl Pts',(1.78327315618183,-0.333333333333333,
-3.29885386921599));
#54552=CARTESIAN_POINT('Ctrl Pts',(1.78327315618183,-0.666666666666667,
-3.29885386921599));
#54553=CARTESIAN_POINT('Ctrl Pts',(1.78327315618183,-1.,-3.29885386921599));
#54554=CARTESIAN_POINT('Ctrl Pts',(2.12928030988903,-1.,-3.62024382630768));
#54555=CARTESIAN_POINT('Ctrl Pts',(2.12928030988903,1.,-3.62024382630768));
#54556=CARTESIAN_POINT('Ctrl Pts',(2.12796193131368,-1.,-3.61938653649098));
#54557=CARTESIAN_POINT('Ctrl Pts',(2.12796193131368,1.,-3.61938653649098));
#54558=CARTESIAN_POINT('Ctrl Pts',(2.12532774376758,-1.,-3.61766963590482));
#54559=CARTESIAN_POINT('Ctrl Pts',(2.12532774376758,1.,-3.61766963590482));
#54560=CARTESIAN_POINT('Ctrl Pts',(2.12138417126355,-1.,-3.61508732216891));
#54561=CARTESIAN_POINT('Ctrl Pts',(2.12138417126355,1.,-3.61508732216891));
#54562=CARTESIAN_POINT('Ctrl Pts',(2.11614149815106,-1.,-3.61163030609447));
#54563=CARTESIAN_POINT('Ctrl Pts',(2.11614149815106,1.,-3.61163030609447));
#54564=CARTESIAN_POINT('Ctrl Pts',(2.10961391334462,-1.,-3.60728578532601));
#54565=CARTESIAN_POINT('Ctrl Pts',(2.10961391334462,1.,-3.60728578532601));
#54566=CARTESIAN_POINT('Ctrl Pts',(2.1031121772821,-1.,-3.60291797088734));
#54567=CARTESIAN_POINT('Ctrl Pts',(2.1031121772821,1.,-3.60291797088734));
#54568=CARTESIAN_POINT('Ctrl Pts',(2.09663642986631,-1.,-3.59852681775485));
#54569=CARTESIAN_POINT('Ctrl Pts',(2.09663642986631,1.,-3.59852681775485));
#54570=CARTESIAN_POINT('Ctrl Pts',(2.09018686331416,-1.,-3.59411228625588));
#54571=CARTESIAN_POINT('Ctrl Pts',(2.09018686331416,1.,-3.59411228625588));
#54572=CARTESIAN_POINT('Ctrl Pts',(2.08376373048756,-1.,-3.58967435355088));
#54573=CARTESIAN_POINT('Ctrl Pts',(2.08376373048756,1.,-3.58967435355088));
#54574=CARTESIAN_POINT('Ctrl Pts',(2.07736732842117,-1.,-3.58521300039299));
#54575=CARTESIAN_POINT('Ctrl Pts',(2.07736732842117,1.,-3.58521300039299));
#54576=CARTESIAN_POINT('Ctrl Pts',(2.07099797605747,-1.,-3.58072819250442));
#54577=CARTESIAN_POINT('Ctrl Pts',(2.07099797605747,1.,-3.58072819250442));
#54578=CARTESIAN_POINT('Ctrl Pts',(2.06465599229174,-1.,-3.576219862243));
#54579=CARTESIAN_POINT('Ctrl Pts',(2.06465599229174,1.,-3.576219862243));
#54580=CARTESIAN_POINT('Ctrl Pts',(2.05834167687523,-1.,-3.57168789423507));
#54581=CARTESIAN_POINT('Ctrl Pts',(2.05834167687523,1.,-3.57168789423507));
#54582=CARTESIAN_POINT('Ctrl Pts',(2.0520552817309,-1.,-3.56713209978208));
#54583=CARTESIAN_POINT('Ctrl Pts',(2.0520552817309,1.,-3.56713209978208));
#54584=CARTESIAN_POINT('Ctrl Pts',(2.04579702159056,-1.,-3.5625522387181));
#54585=CARTESIAN_POINT('Ctrl Pts',(2.04579702159056,1.,-3.5625522387181));
#54586=CARTESIAN_POINT('Ctrl Pts',(2.03956711120099,-1.,-3.55794807265052));
#54587=CARTESIAN_POINT('Ctrl Pts',(2.03956711120099,1.,-3.55794807265052));
#54588=CARTESIAN_POINT('Ctrl Pts',(2.03336579658174,-1.,-3.55331941294018));
#54589=CARTESIAN_POINT('Ctrl Pts',(2.03336579658174,1.,-3.55331941294018));
#54590=CARTESIAN_POINT('Ctrl Pts',(2.02719338376144,-1.,-3.54866616282173));
#54591=CARTESIAN_POINT('Ctrl Pts',(2.02719338376144,1.,-3.54866616282173));
#54592=CARTESIAN_POINT('Ctrl Pts',(2.0210502798303,-1.,-3.54398838254011));
#54593=CARTESIAN_POINT('Ctrl Pts',(2.0210502798303,1.,-3.54398838254011));
#54594=CARTESIAN_POINT('Ctrl Pts',(2.0149369884727,-1.,-3.53928627453503));
#54595=CARTESIAN_POINT('Ctrl Pts',(2.0149369884727,1.,-3.53928627453503));
#54596=CARTESIAN_POINT('Ctrl Pts',(2.00885403604685,-1.,-3.53456004727321));
#54597=CARTESIAN_POINT('Ctrl Pts',(2.00885403604685,1.,-3.53456004727321));
#54598=CARTESIAN_POINT('Ctrl Pts',(2.00280191090341,-1.,-3.52980980250181));
#54599=CARTESIAN_POINT('Ctrl Pts',(2.00280191090341,1.,-3.52980980250181));
#54600=CARTESIAN_POINT('Ctrl Pts',(1.99678100339305,-1.,-3.52503542491745));
#54601=CARTESIAN_POINT('Ctrl Pts',(1.99678100339305,1.,-3.52503542491745));
#54602=CARTESIAN_POINT('Ctrl Pts',(1.99079153006143,-1.,-3.52023644289195));
#54603=CARTESIAN_POINT('Ctrl Pts',(1.99079153006143,1.,-3.52023644289195));
#54604=CARTESIAN_POINT('Ctrl Pts',(1.98483351061066,-1.,-3.51541198728362));
#54605=CARTESIAN_POINT('Ctrl Pts',(1.98483351061066,1.,-3.51541198728362));
#54606=CARTESIAN_POINT('Ctrl Pts',(1.97890693666316,-1.,-3.51056110478334));
#54607=CARTESIAN_POINT('Ctrl Pts',(1.97890693666316,1.,-3.51056110478334));
#54608=CARTESIAN_POINT('Ctrl Pts',(1.9730119116298,-1.,-3.505683018611));
#54609=CARTESIAN_POINT('Ctrl Pts',(1.9730119116298,1.,-3.505683018611));
#54610=CARTESIAN_POINT('Ctrl Pts',(1.9671487972405,-1.,-3.50077740176262));
#54611=CARTESIAN_POINT('Ctrl Pts',(1.9671487972405,1.,-3.50077740176262));
#54612=CARTESIAN_POINT('Ctrl Pts',(1.96131836776489,-1.,-3.49584466573045));
#54613=CARTESIAN_POINT('Ctrl Pts',(1.96131836776489,1.,-3.49584466573045));
#54614=CARTESIAN_POINT('Ctrl Pts',(1.95552193112071,-1.,-3.49088618670967));
#54615=CARTESIAN_POINT('Ctrl Pts',(1.95552193112071,1.,-3.49088618670967));
#54616=CARTESIAN_POINT('Ctrl Pts',(1.94976096795902,-1.,-3.485903616108));
#54617=CARTESIAN_POINT('Ctrl Pts',(1.94976096795902,1.,-3.485903616108));
#54618=CARTESIAN_POINT('Ctrl Pts',(1.94403680554062,-1.,-3.48089825770412));
#54619=CARTESIAN_POINT('Ctrl Pts',(1.94403680554062,1.,-3.48089825770412));
#54620=CARTESIAN_POINT('Ctrl Pts',(1.93835026973888,-1.,-3.47587040389916));
#54621=CARTESIAN_POINT('Ctrl Pts',(1.93835026973888,1.,-3.47587040389916));
#54622=CARTESIAN_POINT('Ctrl Pts',(1.93270136427083,-1.,-3.47081872409783));
#54623=CARTESIAN_POINT('Ctrl Pts',(1.93270136427083,1.,-3.47081872409783));
#54624=CARTESIAN_POINT('Ctrl Pts',(1.92708888591159,-1.,-3.46573953254084));
#54625=CARTESIAN_POINT('Ctrl Pts',(1.92708888591159,1.,-3.46573953254084));
#54626=CARTESIAN_POINT('Ctrl Pts',(1.9215111821321,-1.,-3.4606282172248));
#54627=CARTESIAN_POINT('Ctrl Pts',(1.9215111821321,1.,-3.4606282172248));
#54628=CARTESIAN_POINT('Ctrl Pts',(1.9159669478406,-1.,-3.45548074309943));
#54629=CARTESIAN_POINT('Ctrl Pts',(1.9159669478406,1.,-3.45548074309943));
#54630=CARTESIAN_POINT('Ctrl Pts',(1.91045605593638,-1.,-3.45029522038885));
#54631=CARTESIAN_POINT('Ctrl Pts',(1.91045605593638,1.,-3.45029522038885));
#54632=CARTESIAN_POINT('Ctrl Pts',(1.90498026502308,-1.,-3.44507323983374));
#54633=CARTESIAN_POINT('Ctrl Pts',(1.90498026502308,1.,-3.44507323983374));
#54634=CARTESIAN_POINT('Ctrl Pts',(1.89954426803392,-1.,-3.43982185678105));
#54635=CARTESIAN_POINT('Ctrl Pts',(1.89954426803392,1.,-3.43982185678105));
#54636=CARTESIAN_POINT('Ctrl Pts',(1.89415420002553,-1.,-3.43455074411591));
#54637=CARTESIAN_POINT('Ctrl Pts',(1.89415420002553,1.,-3.43455074411591));
#54638=CARTESIAN_POINT('Ctrl Pts',(1.88881571322018,-1.,-3.42926852222174));
#54639=CARTESIAN_POINT('Ctrl Pts',(1.88881571322018,1.,-3.42926852222174));
#54640=CARTESIAN_POINT('Ctrl Pts',(1.88353205062063,-1.,-3.42397908819741));
#54641=CARTESIAN_POINT('Ctrl Pts',(1.88353205062063,1.,-3.42397908819741));
#54642=CARTESIAN_POINT('Ctrl Pts',(1.87830245689338,-1.,-3.4186785838376));
#54643=CARTESIAN_POINT('Ctrl Pts',(1.87830245689338,1.,-3.4186785838376));
#54644=CARTESIAN_POINT('Ctrl Pts',(1.87311957248106,-1.,-3.41335043875182));
#54645=CARTESIAN_POINT('Ctrl Pts',(1.87311957248106,1.,-3.41335043875182));
#54646=CARTESIAN_POINT('Ctrl Pts',(1.86797231196635,-1.,-3.40797080000513));
#54647=CARTESIAN_POINT('Ctrl Pts',(1.86797231196635,1.,-3.40797080000513));
#54648=CARTESIAN_POINT('Ctrl Pts',(1.86285057051228,-1.,-3.40251742305445));
#54649=CARTESIAN_POINT('Ctrl Pts',(1.86285057051228,1.,-3.40251742305445));
#54650=CARTESIAN_POINT('Ctrl Pts',(1.85774972037055,-1.,-3.39697816833056));
#54651=CARTESIAN_POINT('Ctrl Pts',(1.85774972037055,1.,-3.39697816833056));
#54652=CARTESIAN_POINT('Ctrl Pts',(1.85267433291778,-1.,-3.39135802549415));
#54653=CARTESIAN_POINT('Ctrl Pts',(1.85267433291778,1.,-3.39135802549415));
#54654=CARTESIAN_POINT('Ctrl Pts',(1.84764441927778,-1.,-3.38569092349639));
#54655=CARTESIAN_POINT('Ctrl Pts',(1.84764441927778,1.,-3.38569092349639));
#54656=CARTESIAN_POINT('Ctrl Pts',(1.84269016931679,-1.,-3.38002968341222));
#54657=CARTESIAN_POINT('Ctrl Pts',(1.84269016931679,1.,-3.38002968341222));
#54658=CARTESIAN_POINT('Ctrl Pts',(1.83784072967111,-1.,-3.37442462015914));
#54659=CARTESIAN_POINT('Ctrl Pts',(1.83784072967111,1.,-3.37442462015914));
#54660=CARTESIAN_POINT('Ctrl Pts',(1.83311391452338,-1.,-3.36890396271864));
#54661=CARTESIAN_POINT('Ctrl Pts',(1.83311391452338,1.,-3.36890396271864));
#54662=CARTESIAN_POINT('Ctrl Pts',(1.82850752153182,-1.,-3.36345722124127));
#54663=CARTESIAN_POINT('Ctrl Pts',(1.82850752153182,1.,-3.36345722124127));
#54664=CARTESIAN_POINT('Ctrl Pts',(1.82398496829247,-1.,-3.35800801557326));
#54665=CARTESIAN_POINT('Ctrl Pts',(1.82398496829247,1.,-3.35800801557326));
#54666=CARTESIAN_POINT('Ctrl Pts',(1.81948458796748,-1.,-3.35243086937451));
#54667=CARTESIAN_POINT('Ctrl Pts',(1.81948458796748,1.,-3.35243086937451));
#54668=CARTESIAN_POINT('Ctrl Pts',(1.81494618732772,-1.,-3.34660014370527));
#54669=CARTESIAN_POINT('Ctrl Pts',(1.81494618732772,1.,-3.34660014370527));
#54670=CARTESIAN_POINT('Ctrl Pts',(1.81033399625311,-1.,-3.34043216147532));
#54671=CARTESIAN_POINT('Ctrl Pts',(1.81033399625311,1.,-3.34043216147532));
#54672=CARTESIAN_POINT('Ctrl Pts',(1.80565802981138,-1.,-3.33392460276874));
#54673=CARTESIAN_POINT('Ctrl Pts',(1.80565802981138,1.,-3.33392460276874));
#54674=CARTESIAN_POINT('Ctrl Pts',(1.80100380443535,-1.,-3.3272108803981));
#54675=CARTESIAN_POINT('Ctrl Pts',(1.80100380443535,1.,-3.3272108803981));
#54676=CARTESIAN_POINT('Ctrl Pts',(1.79652817033444,-1.,-3.32055355101168));
#54677=CARTESIAN_POINT('Ctrl Pts',(1.79652817033444,1.,-3.32055355101168));
#54678=CARTESIAN_POINT('Ctrl Pts',(1.79242331350137,-1.,-3.31428038326763));
#54679=CARTESIAN_POINT('Ctrl Pts',(1.79242331350137,1.,-3.31428038326763));
#54680=CARTESIAN_POINT('Ctrl Pts',(1.78888832245965,-1.,-3.30873412266954));
#54681=CARTESIAN_POINT('Ctrl Pts',(1.78888832245965,1.,-3.30873412266954));
#54682=CARTESIAN_POINT('Ctrl Pts',(1.78610045419769,-1.,-3.30422155558973));
#54683=CARTESIAN_POINT('Ctrl Pts',(1.78610045419769,1.,-3.30422155558973));
#54684=CARTESIAN_POINT('Ctrl Pts',(1.78417972819696,-1.,-3.30095096463082));
#54685=CARTESIAN_POINT('Ctrl Pts',(1.78417972819696,1.,-3.30095096463082));
#54686=CARTESIAN_POINT('Ctrl Pts',(1.78338186555671,-1.,-3.29940631673818));
#54687=CARTESIAN_POINT('Ctrl Pts',(1.78338186555671,1.,-3.29940631673818));
#54688=CARTESIAN_POINT('Ctrl Pts',(1.78320756177191,-1.,-3.29886572077303));
#54689=CARTESIAN_POINT('Ctrl Pts',(1.78320756177191,1.,-3.29886572077303));
#54690=CARTESIAN_POINT('Ctrl Pts',(1.78327971836272,-1.,-3.29877974053191));
#54691=CARTESIAN_POINT('Ctrl Pts',(1.78327971836272,1.,-3.29877974053191));
#54692=CARTESIAN_POINT('Ctrl Pts',(1.7833628895577,-1.,-3.2988053601491));
#54693=CARTESIAN_POINT('Ctrl Pts',(1.7833628895577,1.,-3.2988053601491));
#54694=CARTESIAN_POINT('',(2.12928030988903,1.,-3.62024382630768));
#54695=CARTESIAN_POINT('Ctrl Pts',(2.12928030988903,1.,-3.62024382630768));
#54696=CARTESIAN_POINT('Ctrl Pts',(2.12796193131368,1.,-3.61938653649098));
#54697=CARTESIAN_POINT('Ctrl Pts',(2.12532774376758,1.,-3.61766963590482));
#54698=CARTESIAN_POINT('Ctrl Pts',(2.12138417126355,1.,-3.61508732216891));
#54699=CARTESIAN_POINT('Ctrl Pts',(2.11614149815106,1.,-3.61163030609447));
#54700=CARTESIAN_POINT('Ctrl Pts',(2.10961391334462,1.,-3.60728578532601));
#54701=CARTESIAN_POINT('Ctrl Pts',(2.1031121772821,1.,-3.60291797088734));
#54702=CARTESIAN_POINT('Ctrl Pts',(2.09663642986631,1.,-3.59852681775485));
#54703=CARTESIAN_POINT('Ctrl Pts',(2.09018686331416,1.,-3.59411228625588));
#54704=CARTESIAN_POINT('Ctrl Pts',(2.08376373048756,1.,-3.58967435355088));
#54705=CARTESIAN_POINT('Ctrl Pts',(2.07736732842117,1.,-3.58521300039299));
#54706=CARTESIAN_POINT('Ctrl Pts',(2.07099797605747,1.,-3.58072819250442));
#54707=CARTESIAN_POINT('Ctrl Pts',(2.06465599229174,1.,-3.576219862243));
#54708=CARTESIAN_POINT('Ctrl Pts',(2.05834167687523,1.,-3.57168789423507));
#54709=CARTESIAN_POINT('Ctrl Pts',(2.0520552817309,1.,-3.56713209978208));
#54710=CARTESIAN_POINT('Ctrl Pts',(2.04579702159056,1.,-3.5625522387181));
#54711=CARTESIAN_POINT('Ctrl Pts',(2.03956711120099,1.,-3.55794807265052));
#54712=CARTESIAN_POINT('Ctrl Pts',(2.03336579658174,1.,-3.55331941294018));
#54713=CARTESIAN_POINT('Ctrl Pts',(2.02719338376144,1.,-3.54866616282173));
#54714=CARTESIAN_POINT('Ctrl Pts',(2.0210502798303,1.,-3.54398838254011));
#54715=CARTESIAN_POINT('Ctrl Pts',(2.0149369884727,1.,-3.53928627453503));
#54716=CARTESIAN_POINT('Ctrl Pts',(2.00885403604685,1.,-3.53456004727321));
#54717=CARTESIAN_POINT('Ctrl Pts',(2.00280191090341,1.,-3.52980980250181));
#54718=CARTESIAN_POINT('Ctrl Pts',(1.99678100339305,1.,-3.52503542491745));
#54719=CARTESIAN_POINT('Ctrl Pts',(1.99079153006143,1.,-3.52023644289195));
#54720=CARTESIAN_POINT('Ctrl Pts',(1.98483351061066,1.,-3.51541198728362));
#54721=CARTESIAN_POINT('Ctrl Pts',(1.97890693666316,1.,-3.51056110478334));
#54722=CARTESIAN_POINT('Ctrl Pts',(1.9730119116298,1.,-3.505683018611));
#54723=CARTESIAN_POINT('Ctrl Pts',(1.9671487972405,1.,-3.50077740176262));
#54724=CARTESIAN_POINT('Ctrl Pts',(1.96131836776489,1.,-3.49584466573045));
#54725=CARTESIAN_POINT('Ctrl Pts',(1.95552193112071,1.,-3.49088618670967));
#54726=CARTESIAN_POINT('Ctrl Pts',(1.94976096795902,1.,-3.485903616108));
#54727=CARTESIAN_POINT('Ctrl Pts',(1.94403680554062,1.,-3.48089825770412));
#54728=CARTESIAN_POINT('Ctrl Pts',(1.93835026973888,1.,-3.47587040389916));
#54729=CARTESIAN_POINT('Ctrl Pts',(1.93270136427083,1.,-3.47081872409783));
#54730=CARTESIAN_POINT('Ctrl Pts',(1.92708888591159,1.,-3.46573953254084));
#54731=CARTESIAN_POINT('Ctrl Pts',(1.9215111821321,1.,-3.4606282172248));
#54732=CARTESIAN_POINT('Ctrl Pts',(1.9159669478406,1.,-3.45548074309943));
#54733=CARTESIAN_POINT('Ctrl Pts',(1.91045605593638,1.,-3.45029522038885));
#54734=CARTESIAN_POINT('Ctrl Pts',(1.90498026502308,1.,-3.44507323983374));
#54735=CARTESIAN_POINT('Ctrl Pts',(1.89954426803392,1.,-3.43982185678105));
#54736=CARTESIAN_POINT('Ctrl Pts',(1.89415420002553,1.,-3.43455074411591));
#54737=CARTESIAN_POINT('Ctrl Pts',(1.88881571322018,1.,-3.42926852222174));
#54738=CARTESIAN_POINT('Ctrl Pts',(1.88353205062063,1.,-3.42397908819741));
#54739=CARTESIAN_POINT('Ctrl Pts',(1.87830245689338,1.,-3.4186785838376));
#54740=CARTESIAN_POINT('Ctrl Pts',(1.87311957248106,1.,-3.41335043875182));
#54741=CARTESIAN_POINT('Ctrl Pts',(1.86797231196635,1.,-3.40797080000513));
#54742=CARTESIAN_POINT('Ctrl Pts',(1.86285057051228,1.,-3.40251742305445));
#54743=CARTESIAN_POINT('Ctrl Pts',(1.85774972037055,1.,-3.39697816833056));
#54744=CARTESIAN_POINT('Ctrl Pts',(1.85267433291778,1.,-3.39135802549415));
#54745=CARTESIAN_POINT('Ctrl Pts',(1.84764441927778,1.,-3.38569092349639));
#54746=CARTESIAN_POINT('Ctrl Pts',(1.84269016931679,1.,-3.38002968341222));
#54747=CARTESIAN_POINT('Ctrl Pts',(1.83784072967111,1.,-3.37442462015914));
#54748=CARTESIAN_POINT('Ctrl Pts',(1.83311391452338,1.,-3.36890396271864));
#54749=CARTESIAN_POINT('Ctrl Pts',(1.82850752153182,1.,-3.36345722124127));
#54750=CARTESIAN_POINT('Ctrl Pts',(1.82398496829247,1.,-3.35800801557326));
#54751=CARTESIAN_POINT('Ctrl Pts',(1.81948458796748,1.,-3.35243086937451));
#54752=CARTESIAN_POINT('Ctrl Pts',(1.81494618732772,1.,-3.34660014370527));
#54753=CARTESIAN_POINT('Ctrl Pts',(1.81033399625311,1.,-3.34043216147532));
#54754=CARTESIAN_POINT('Ctrl Pts',(1.80565802981138,1.,-3.33392460276874));
#54755=CARTESIAN_POINT('Ctrl Pts',(1.80100380443535,1.,-3.3272108803981));
#54756=CARTESIAN_POINT('Ctrl Pts',(1.79652817033444,1.,-3.32055355101168));
#54757=CARTESIAN_POINT('Ctrl Pts',(1.79242331350137,1.,-3.31428038326763));
#54758=CARTESIAN_POINT('Ctrl Pts',(1.78888832245965,1.,-3.30873412266954));
#54759=CARTESIAN_POINT('Ctrl Pts',(1.78610045419769,1.,-3.30422155558973));
#54760=CARTESIAN_POINT('Ctrl Pts',(1.7843238478823,1.,-3.30119637003466));
#54761=CARTESIAN_POINT('Ctrl Pts',(1.78353803106983,1.,-3.29970549824336));
#54762=CARTESIAN_POINT('Ctrl Pts',(1.78329283591903,1.,-3.29909749657945));
#54763=CARTESIAN_POINT('Ctrl Pts',(1.78326534445426,1.,-3.29890219175522));
#54764=CARTESIAN_POINT('Ctrl Pts',(1.78327315618183,1.,-3.29885386921599));
#54765=CARTESIAN_POINT('',(2.12928030988903,0.,-3.62024382630768));
#54766=CARTESIAN_POINT('Ctrl Pts',(2.12962728847314,-1.,-3.08661426358891));
#54767=CARTESIAN_POINT('Ctrl Pts',(2.12962728847314,1.,-3.08661426358891));
#54768=CARTESIAN_POINT('Ctrl Pts',(2.12964222016025,-1.,-3.08652852644995));
#54769=CARTESIAN_POINT('Ctrl Pts',(2.12964222016025,1.,-3.08652852644995));
#54770=CARTESIAN_POINT('Ctrl Pts',(2.12975158752407,-1.,-3.08650326867133));
#54771=CARTESIAN_POINT('Ctrl Pts',(2.12975158752407,1.,-3.08650326867133));
#54772=CARTESIAN_POINT('Ctrl Pts',(2.1301541297946,-1.,-3.08690399991464));
#54773=CARTESIAN_POINT('Ctrl Pts',(2.1301541297946,1.,-3.08690399991464));
#54774=CARTESIAN_POINT('Ctrl Pts',(2.13116819908542,-1.,-3.08831615620074));
#54775=CARTESIAN_POINT('Ctrl Pts',(2.13116819908542,1.,-3.08831615620074));
#54776=CARTESIAN_POINT('Ctrl Pts',(2.13321032560893,-1.,-3.09151235281963));
#54777=CARTESIAN_POINT('Ctrl Pts',(2.13321032560893,1.,-3.09151235281963));
#54778=CARTESIAN_POINT('Ctrl Pts',(2.13596538661048,-1.,-3.0960450242104));
#54779=CARTESIAN_POINT('Ctrl Pts',(2.13596538661048,1.,-3.0960450242104));
#54780=CARTESIAN_POINT('Ctrl Pts',(2.13930228863751,-1.,-3.10171267391049));
#54781=CARTESIAN_POINT('Ctrl Pts',(2.13930228863751,1.,-3.10171267391049));
#54782=CARTESIAN_POINT('Ctrl Pts',(2.14302815601973,-1.,-3.1082180866886));
#54783=CARTESIAN_POINT('Ctrl Pts',(2.14302815601973,1.,-3.1082180866886));
#54784=CARTESIAN_POINT('Ctrl Pts',(2.14692798457532,-1.,-3.11522827016855));
#54785=CARTESIAN_POINT('Ctrl Pts',(2.14692798457532,1.,-3.11522827016855));
#54786=CARTESIAN_POINT('Ctrl Pts',(2.15079698090584,-1.,-3.12242318151938));
#54787=CARTESIAN_POINT('Ctrl Pts',(2.15079698090584,1.,-3.12242318151938));
#54788=CARTESIAN_POINT('Ctrl Pts',(2.1544724138292,-1.,-3.12954386795646));
#54789=CARTESIAN_POINT('Ctrl Pts',(2.1544724138292,1.,-3.12954386795646));
#54790=CARTESIAN_POINT('Ctrl Pts',(2.15787423530676,-1.,-3.13645356563038));
#54791=CARTESIAN_POINT('Ctrl Pts',(2.15787423530676,1.,-3.13645356563038));
#54792=CARTESIAN_POINT('Ctrl Pts',(2.16100905914435,-1.,-3.14314440427022));
#54793=CARTESIAN_POINT('Ctrl Pts',(2.16100905914435,1.,-3.14314440427022));
#54794=CARTESIAN_POINT('Ctrl Pts',(2.16393520288072,-1.,-3.14968624389054));
#54795=CARTESIAN_POINT('Ctrl Pts',(2.16393520288072,1.,-3.14968624389054));
#54796=CARTESIAN_POINT('Ctrl Pts',(2.16673728447689,-1.,-3.15618975593656));
#54797=CARTESIAN_POINT('Ctrl Pts',(2.16673728447689,1.,-3.15618975593656));
#54798=CARTESIAN_POINT('Ctrl Pts',(2.16949910801219,-1.,-3.16276685102972));
#54799=CARTESIAN_POINT('Ctrl Pts',(2.16949910801219,1.,-3.16276685102972));
#54800=CARTESIAN_POINT('Ctrl Pts',(2.17227212063817,-1.,-3.16948480019497));
#54801=CARTESIAN_POINT('Ctrl Pts',(2.17227212063817,1.,-3.16948480019497));
#54802=CARTESIAN_POINT('Ctrl Pts',(2.17506466903694,-1.,-3.17635032802523));
#54803=CARTESIAN_POINT('Ctrl Pts',(2.17506466903694,1.,-3.17635032802523));
#54804=CARTESIAN_POINT('Ctrl Pts',(2.17785968847142,-1.,-3.18333474627807));
#54805=CARTESIAN_POINT('Ctrl Pts',(2.17785968847142,1.,-3.18333474627807));
#54806=CARTESIAN_POINT('Ctrl Pts',(2.18062558031778,-1.,-3.19038924261573));
#54807=CARTESIAN_POINT('Ctrl Pts',(2.18062558031778,1.,-3.19038924261573));
#54808=CARTESIAN_POINT('Ctrl Pts',(2.18332898656602,-1.,-3.19746293740411));
#54809=CARTESIAN_POINT('Ctrl Pts',(2.18332898656602,1.,-3.19746293740411));
#54810=CARTESIAN_POINT('Ctrl Pts',(2.18594876115934,-1.,-3.20452259717976));
#54811=CARTESIAN_POINT('Ctrl Pts',(2.18594876115934,1.,-3.20452259717976));
#54812=CARTESIAN_POINT('Ctrl Pts',(2.18848253363901,-1.,-3.21156188355769));
#54813=CARTESIAN_POINT('Ctrl Pts',(2.18848253363901,1.,-3.21156188355769));
#54814=CARTESIAN_POINT('Ctrl Pts',(2.19093901948667,-1.,-3.21859043114095));
#54815=CARTESIAN_POINT('Ctrl Pts',(2.19093901948667,1.,-3.21859043114095));
#54816=CARTESIAN_POINT('Ctrl Pts',(2.19333345123538,-1.,-3.22562734221646));
#54817=CARTESIAN_POINT('Ctrl Pts',(2.19333345123538,1.,-3.22562734221646));
#54818=CARTESIAN_POINT('Ctrl Pts',(2.19568204933168,-1.,-3.23269332296933));
#54819=CARTESIAN_POINT('Ctrl Pts',(2.19568204933168,1.,-3.23269332296933));
#54820=CARTESIAN_POINT('Ctrl Pts',(2.19799623693253,-1.,-3.23980245361308));
#54821=CARTESIAN_POINT('Ctrl Pts',(2.19799623693253,1.,-3.23980245361308));
#54822=CARTESIAN_POINT('Ctrl Pts',(2.20027910880981,-1.,-3.24695715874338));
#54823=CARTESIAN_POINT('Ctrl Pts',(2.20027910880981,1.,-3.24695715874338));
#54824=CARTESIAN_POINT('Ctrl Pts',(2.20252866491545,-1.,-3.25415277957775));
#54825=CARTESIAN_POINT('Ctrl Pts',(2.20252866491545,1.,-3.25415277957775));
#54826=CARTESIAN_POINT('Ctrl Pts',(2.20473979048678,-1.,-3.26138036637705));
#54827=CARTESIAN_POINT('Ctrl Pts',(2.20473979048678,1.,-3.26138036637705));
#54828=CARTESIAN_POINT('Ctrl Pts',(2.20690665217742,-1.,-3.26863006136782));
#54829=CARTESIAN_POINT('Ctrl Pts',(2.20690665217742,1.,-3.26863006136782));
#54830=CARTESIAN_POINT('Ctrl Pts',(2.2090250941743,-1.,-3.2758944800554));
#54831=CARTESIAN_POINT('Ctrl Pts',(2.2090250941743,1.,-3.2758944800554));
#54832=CARTESIAN_POINT('Ctrl Pts',(2.21109449750641,-1.,-3.28317133333131));
#54833=CARTESIAN_POINT('Ctrl Pts',(2.21109449750641,1.,-3.28317133333131));
#54834=CARTESIAN_POINT('Ctrl Pts',(2.21311648827391,-1.,-3.29046159238343));
#54835=CARTESIAN_POINT('Ctrl Pts',(2.21311648827391,1.,-3.29046159238343));
#54836=CARTESIAN_POINT('Ctrl Pts',(2.21509406923368,-1.,-3.29776825193159));
#54837=CARTESIAN_POINT('Ctrl Pts',(2.21509406923368,1.,-3.29776825193159));
#54838=CARTESIAN_POINT('Ctrl Pts',(2.21703059947836,-1.,-3.30509487819569));
#54839=CARTESIAN_POINT('Ctrl Pts',(2.21703059947836,1.,-3.30509487819569));
#54840=CARTESIAN_POINT('Ctrl Pts',(2.21892881679086,-1.,-3.31244421655666));
#54841=CARTESIAN_POINT('Ctrl Pts',(2.21892881679086,1.,-3.31244421655666));
#54842=CARTESIAN_POINT('Ctrl Pts',(2.22078990842776,-1.,-3.31981686778022));
#54843=CARTESIAN_POINT('Ctrl Pts',(2.22078990842776,1.,-3.31981686778022));
#54844=CARTESIAN_POINT('Ctrl Pts',(2.22261398879635,-1.,-3.3272119632604));
#54845=CARTESIAN_POINT('Ctrl Pts',(2.22261398879635,1.,-3.3272119632604));
#54846=CARTESIAN_POINT('Ctrl Pts',(2.22440049878511,-1.,-3.33462772849598));
#54847=CARTESIAN_POINT('Ctrl Pts',(2.22440049878511,1.,-3.33462772849598));
#54848=CARTESIAN_POINT('Ctrl Pts',(2.22614863918047,-1.,-3.34206209449375));
#54849=CARTESIAN_POINT('Ctrl Pts',(2.22614863918047,1.,-3.34206209449375));
#54850=CARTESIAN_POINT('Ctrl Pts',(2.22785777756576,-1.,-3.34951327111096));
#54851=CARTESIAN_POINT('Ctrl Pts',(2.22785777756576,1.,-3.34951327111096));
#54852=CARTESIAN_POINT('Ctrl Pts',(2.22952789880982,-1.,-3.35698038165483));
#54853=CARTESIAN_POINT('Ctrl Pts',(2.22952789880982,1.,-3.35698038165483));
#54854=CARTESIAN_POINT('Ctrl Pts',(2.23115945849739,-1.,-3.36446325227848));
#54855=CARTESIAN_POINT('Ctrl Pts',(2.23115945849739,1.,-3.36446325227848));
#54856=CARTESIAN_POINT('Ctrl Pts',(2.23275319569221,-1.,-3.37196214349304));
#54857=CARTESIAN_POINT('Ctrl Pts',(2.23275319569221,1.,-3.37196214349304));
#54858=CARTESIAN_POINT('Ctrl Pts',(2.23430995599561,-1.,-3.37947749555632));
#54859=CARTESIAN_POINT('Ctrl Pts',(2.23430995599561,1.,-3.37947749555632));
#54860=CARTESIAN_POINT('Ctrl Pts',(2.23583052276308,-1.,-3.38700968549563));
#54861=CARTESIAN_POINT('Ctrl Pts',(2.23583052276308,1.,-3.38700968549563));
#54862=CARTESIAN_POINT('Ctrl Pts',(2.23731541452791,-1.,-3.39455873448189));
#54863=CARTESIAN_POINT('Ctrl Pts',(2.23731541452791,1.,-3.39455873448189));
#54864=CARTESIAN_POINT('Ctrl Pts',(2.2387649112415,-1.,-3.40212434705647));
#54865=CARTESIAN_POINT('Ctrl Pts',(2.2387649112415,1.,-3.40212434705647));
#54866=CARTESIAN_POINT('Ctrl Pts',(2.24017914395289,-1.,-3.40970604190328));
#54867=CARTESIAN_POINT('Ctrl Pts',(2.24017914395289,1.,-3.40970604190328));
#54868=CARTESIAN_POINT('Ctrl Pts',(2.24155816587844,-1.,-3.41730325539172));
#54869=CARTESIAN_POINT('Ctrl Pts',(2.24155816587844,1.,-3.41730325539172));
#54870=CARTESIAN_POINT('Ctrl Pts',(2.24290202531101,-1.,-3.42491544683008));
#54871=CARTESIAN_POINT('Ctrl Pts',(2.24290202531101,1.,-3.42491544683008));
#54872=CARTESIAN_POINT('Ctrl Pts',(2.24421085338727,-1.,-3.43254222614803));
#54873=CARTESIAN_POINT('Ctrl Pts',(2.24421085338727,1.,-3.43254222614803));
#54874=CARTESIAN_POINT('Ctrl Pts',(2.24548487526022,-1.,-3.4401833646032));
#54875=CARTESIAN_POINT('Ctrl Pts',(2.24548487526022,1.,-3.4401833646032));
#54876=CARTESIAN_POINT('Ctrl Pts',(2.2467243706995,-1.,-3.44783872863151));
#54877=CARTESIAN_POINT('Ctrl Pts',(2.2467243706995,1.,-3.44783872863151));
#54878=CARTESIAN_POINT('Ctrl Pts',(2.2479296496077,-1.,-3.45550823512049));
#54879=CARTESIAN_POINT('Ctrl Pts',(2.2479296496077,1.,-3.45550823512049));
#54880=CARTESIAN_POINT('Ctrl Pts',(2.2491010234604,-1.,-3.46319180177573));
#54881=CARTESIAN_POINT('Ctrl Pts',(2.2491010234604,1.,-3.46319180177573));
#54882=CARTESIAN_POINT('Ctrl Pts',(2.25023877475942,-1.,-3.47088928979889));
#54883=CARTESIAN_POINT('Ctrl Pts',(2.25023877475942,1.,-3.47088928979889));
#54884=CARTESIAN_POINT('Ctrl Pts',(2.25134314238687,-1.,-3.47860048448691));
#54885=CARTESIAN_POINT('Ctrl Pts',(2.25134314238687,1.,-3.47860048448691));
#54886=CARTESIAN_POINT('Ctrl Pts',(2.25241433138695,-1.,-3.48632513240961));
#54887=CARTESIAN_POINT('Ctrl Pts',(2.25241433138695,1.,-3.48632513240961));
#54888=CARTESIAN_POINT('Ctrl Pts',(2.25345251709759,-1.,-3.49406296494791));
#54889=CARTESIAN_POINT('Ctrl Pts',(2.25345251709759,1.,-3.49406296494791));
#54890=CARTESIAN_POINT('Ctrl Pts',(2.25445785151868,-1.,-3.50181372617971));
#54891=CARTESIAN_POINT('Ctrl Pts',(2.25445785151868,1.,-3.50181372617971));
#54892=CARTESIAN_POINT('Ctrl Pts',(2.25543046979799,-1.,-3.50957720117341));
#54893=CARTESIAN_POINT('Ctrl Pts',(2.25543046979799,1.,-3.50957720117341));
#54894=CARTESIAN_POINT('Ctrl Pts',(2.25637049455044,-1.,-3.51735323667612));
#54895=CARTESIAN_POINT('Ctrl Pts',(2.25637049455044,1.,-3.51735323667612));
#54896=CARTESIAN_POINT('Ctrl Pts',(2.25727802940898,-1.,-3.52514172847711));
#54897=CARTESIAN_POINT('Ctrl Pts',(2.25727802940898,1.,-3.52514172847711));
#54898=CARTESIAN_POINT('Ctrl Pts',(2.25797812950104,-1.,-3.53138243688262));
#54899=CARTESIAN_POINT('Ctrl Pts',(2.25797812950104,1.,-3.53138243688262));
#54900=CARTESIAN_POINT('Ctrl Pts',(2.25848864343951,-1.,-3.53606853162228));
#54901=CARTESIAN_POINT('Ctrl Pts',(2.25848864343951,1.,-3.53606853162228));
#54902=CARTESIAN_POINT('Ctrl Pts',(2.2588225169468,-1.,-3.53919506647335));
#54903=CARTESIAN_POINT('Ctrl Pts',(2.2588225169468,1.,-3.53919506647335));
#54904=CARTESIAN_POINT('Ctrl Pts',(2.25898783642071,-1.,-3.54075895182139));
#54905=CARTESIAN_POINT('Ctrl Pts',(2.25898783642071,1.,-3.54075895182139));
#54906=CARTESIAN_POINT('',(2.1297112484669,1.,-3.08655633322212));
#54907=CARTESIAN_POINT('Ctrl Pts',(2.1297112484669,-1.,-3.08655633322212));
#54908=CARTESIAN_POINT('Ctrl Pts',(2.1297112484669,-0.666666666666667,-3.08655633322212));
#54909=CARTESIAN_POINT('Ctrl Pts',(2.1297112484669,-0.333333333333333,-3.08655633322212));
#54910=CARTESIAN_POINT('Ctrl Pts',(2.1297112484669,0.333333333333333,-3.08655633322212));
#54911=CARTESIAN_POINT('Ctrl Pts',(2.1297112484669,0.666666666666667,-3.08655633322212));
#54912=CARTESIAN_POINT('Ctrl Pts',(2.1297112484669,1.,-3.08655633322212));
#54913=CARTESIAN_POINT('',(2.25898783642071,1.,-3.54075895182139));
#54914=CARTESIAN_POINT('',(2.25898783642071,0.,-3.54075895182139));
#54915=CARTESIAN_POINT('Ctrl Pts',(2.1297112484669,1.,-3.08655633322212));
#54916=CARTESIAN_POINT('Ctrl Pts',(2.1297578506149,1.,-3.08657131089497));
#54917=CARTESIAN_POINT('Ctrl Pts',(2.12991938762373,1.,-3.08668447250322));
#54918=CARTESIAN_POINT('Ctrl Pts',(2.13034980480424,1.,-3.08717896996098));
#54919=CARTESIAN_POINT('Ctrl Pts',(2.13132142793017,1.,-3.08855597949761));
#54920=CARTESIAN_POINT('Ctrl Pts',(2.13321032560893,1.,-3.09151235281963));
#54921=CARTESIAN_POINT('Ctrl Pts',(2.13596538661048,1.,-3.0960450242104));
#54922=CARTESIAN_POINT('Ctrl Pts',(2.13930228863751,1.,-3.10171267391049));
#54923=CARTESIAN_POINT('Ctrl Pts',(2.14302815601973,1.,-3.1082180866886));
#54924=CARTESIAN_POINT('Ctrl Pts',(2.14692798457532,1.,-3.11522827016855));
#54925=CARTESIAN_POINT('Ctrl Pts',(2.15079698090584,1.,-3.12242318151938));
#54926=CARTESIAN_POINT('Ctrl Pts',(2.1544724138292,1.,-3.12954386795646));
#54927=CARTESIAN_POINT('Ctrl Pts',(2.15787423530676,1.,-3.13645356563038));
#54928=CARTESIAN_POINT('Ctrl Pts',(2.16100905914435,1.,-3.14314440427022));
#54929=CARTESIAN_POINT('Ctrl Pts',(2.16393520288072,1.,-3.14968624389054));
#54930=CARTESIAN_POINT('Ctrl Pts',(2.16673728447689,1.,-3.15618975593656));
#54931=CARTESIAN_POINT('Ctrl Pts',(2.16949910801219,1.,-3.16276685102972));
#54932=CARTESIAN_POINT('Ctrl Pts',(2.17227212063817,1.,-3.16948480019497));
#54933=CARTESIAN_POINT('Ctrl Pts',(2.17506466903694,1.,-3.17635032802523));
#54934=CARTESIAN_POINT('Ctrl Pts',(2.17785968847142,1.,-3.18333474627807));
#54935=CARTESIAN_POINT('Ctrl Pts',(2.18062558031778,1.,-3.19038924261573));
#54936=CARTESIAN_POINT('Ctrl Pts',(2.18332898656602,1.,-3.19746293740411));
#54937=CARTESIAN_POINT('Ctrl Pts',(2.18594876115934,1.,-3.20452259717976));
#54938=CARTESIAN_POINT('Ctrl Pts',(2.18848253363901,1.,-3.21156188355769));
#54939=CARTESIAN_POINT('Ctrl Pts',(2.19093901948667,1.,-3.21859043114095));
#54940=CARTESIAN_POINT('Ctrl Pts',(2.19333345123538,1.,-3.22562734221646));
#54941=CARTESIAN_POINT('Ctrl Pts',(2.19568204933168,1.,-3.23269332296933));
#54942=CARTESIAN_POINT('Ctrl Pts',(2.19799623693253,1.,-3.23980245361308));
#54943=CARTESIAN_POINT('Ctrl Pts',(2.20027910880981,1.,-3.24695715874338));
#54944=CARTESIAN_POINT('Ctrl Pts',(2.20252866491545,1.,-3.25415277957775));
#54945=CARTESIAN_POINT('Ctrl Pts',(2.20473979048678,1.,-3.26138036637705));
#54946=CARTESIAN_POINT('Ctrl Pts',(2.20690665217742,1.,-3.26863006136782));
#54947=CARTESIAN_POINT('Ctrl Pts',(2.2090250941743,1.,-3.2758944800554));
#54948=CARTESIAN_POINT('Ctrl Pts',(2.21109449750641,1.,-3.28317133333131));
#54949=CARTESIAN_POINT('Ctrl Pts',(2.21311648827391,1.,-3.29046159238343));
#54950=CARTESIAN_POINT('Ctrl Pts',(2.21509406923368,1.,-3.29776825193159));
#54951=CARTESIAN_POINT('Ctrl Pts',(2.21703059947836,1.,-3.30509487819569));
#54952=CARTESIAN_POINT('Ctrl Pts',(2.21892881679086,1.,-3.31244421655666));
#54953=CARTESIAN_POINT('Ctrl Pts',(2.22078990842776,1.,-3.31981686778022));
#54954=CARTESIAN_POINT('Ctrl Pts',(2.22261398879635,1.,-3.3272119632604));
#54955=CARTESIAN_POINT('Ctrl Pts',(2.22440049878511,1.,-3.33462772849598));
#54956=CARTESIAN_POINT('Ctrl Pts',(2.22614863918047,1.,-3.34206209449375));
#54957=CARTESIAN_POINT('Ctrl Pts',(2.22785777756576,1.,-3.34951327111096));
#54958=CARTESIAN_POINT('Ctrl Pts',(2.22952789880982,1.,-3.35698038165483));
#54959=CARTESIAN_POINT('Ctrl Pts',(2.23115945849739,1.,-3.36446325227848));
#54960=CARTESIAN_POINT('Ctrl Pts',(2.23275319569221,1.,-3.37196214349304));
#54961=CARTESIAN_POINT('Ctrl Pts',(2.23430995599561,1.,-3.37947749555632));
#54962=CARTESIAN_POINT('Ctrl Pts',(2.23583052276308,1.,-3.38700968549563));
#54963=CARTESIAN_POINT('Ctrl Pts',(2.23731541452791,1.,-3.39455873448189));
#54964=CARTESIAN_POINT('Ctrl Pts',(2.2387649112415,1.,-3.40212434705647));
#54965=CARTESIAN_POINT('Ctrl Pts',(2.24017914395289,1.,-3.40970604190328));
#54966=CARTESIAN_POINT('Ctrl Pts',(2.24155816587844,1.,-3.41730325539172));
#54967=CARTESIAN_POINT('Ctrl Pts',(2.24290202531101,1.,-3.42491544683008));
#54968=CARTESIAN_POINT('Ctrl Pts',(2.24421085338727,1.,-3.43254222614803));
#54969=CARTESIAN_POINT('Ctrl Pts',(2.24548487526022,1.,-3.4401833646032));
#54970=CARTESIAN_POINT('Ctrl Pts',(2.2467243706995,1.,-3.44783872863151));
#54971=CARTESIAN_POINT('Ctrl Pts',(2.2479296496077,1.,-3.45550823512049));
#54972=CARTESIAN_POINT('Ctrl Pts',(2.2491010234604,1.,-3.46319180177573));
#54973=CARTESIAN_POINT('Ctrl Pts',(2.25023877475942,1.,-3.47088928979889));
#54974=CARTESIAN_POINT('Ctrl Pts',(2.25134314238687,1.,-3.47860048448691));
#54975=CARTESIAN_POINT('Ctrl Pts',(2.25241433138695,1.,-3.48632513240961));
#54976=CARTESIAN_POINT('Ctrl Pts',(2.25345251709759,1.,-3.49406296494791));
#54977=CARTESIAN_POINT('Ctrl Pts',(2.25445785151868,1.,-3.50181372617971));
#54978=CARTESIAN_POINT('Ctrl Pts',(2.25543046979799,1.,-3.50957720117341));
#54979=CARTESIAN_POINT('Ctrl Pts',(2.25637049455044,1.,-3.51735323667612));
#54980=CARTESIAN_POINT('Ctrl Pts',(2.25727802940898,1.,-3.52514172847711));
#54981=CARTESIAN_POINT('Ctrl Pts',(2.25797812950104,1.,-3.53138243688262));
#54982=CARTESIAN_POINT('Ctrl Pts',(2.25848864343951,1.,-3.53606853162228));
#54983=CARTESIAN_POINT('Ctrl Pts',(2.2588225169468,1.,-3.53919506647335));
#54984=CARTESIAN_POINT('Ctrl Pts',(2.25898783642071,1.,-3.54075895182139));
#54985=CARTESIAN_POINT('Origin',(2.25898783642071,0.,-3.54075895182139));
#54986=CARTESIAN_POINT('',(2.12928030988903,1.,-3.62024382630768));
#54987=CARTESIAN_POINT('Origin',(0.,0.,0.));
#54988=CARTESIAN_POINT('',(2.27737254473378,1.,-2.97927412174388));
#54989=CARTESIAN_POINT('Origin',(0.,1.,0.));
#54990=CARTESIAN_POINT('Ctrl Pts',(2.27737254473378,1.,-2.97927412174388));
#54991=CARTESIAN_POINT('Ctrl Pts',(2.27737254473378,0.666666666666667,-2.97927412174388));
#54992=CARTESIAN_POINT('Ctrl Pts',(2.27737254473378,0.333333333333333,-2.97927412174388));
#54993=CARTESIAN_POINT('Ctrl Pts',(2.27737254473378,-0.333333333333333,
-2.97927412174388));
#54994=CARTESIAN_POINT('Ctrl Pts',(2.27737254473378,-0.666666666666667,
-2.97927412174388));
#54995=CARTESIAN_POINT('Ctrl Pts',(2.27737254473378,-1.,-2.97927412174388));
#54996=CARTESIAN_POINT('Ctrl Pts',(2.66939624221984,-1.,-3.24257979115744));
#54997=CARTESIAN_POINT('Ctrl Pts',(2.66939624221984,1.,-3.24257979115744));
#54998=CARTESIAN_POINT('Ctrl Pts',(2.66795998539861,-1.,-3.24193929584813));
#54999=CARTESIAN_POINT('Ctrl Pts',(2.66795998539861,1.,-3.24193929584813));
#55000=CARTESIAN_POINT('Ctrl Pts',(2.66508964664767,-1.,-3.24065561087681));
#55001=CARTESIAN_POINT('Ctrl Pts',(2.66508964664767,1.,-3.24065561087681));
#55002=CARTESIAN_POINT('Ctrl Pts',(2.6607906631973,-1.,-3.23872200036311));
#55003=CARTESIAN_POINT('Ctrl Pts',(2.6607906631973,1.,-3.23872200036311));
#55004=CARTESIAN_POINT('Ctrl Pts',(2.6550717396303,-1.,-3.23612768065687));
#55005=CARTESIAN_POINT('Ctrl Pts',(2.6550717396303,1.,-3.23612768065687));
#55006=CARTESIAN_POINT('Ctrl Pts',(2.64794488744246,-1.,-3.23285778738558));
#55007=CARTESIAN_POINT('Ctrl Pts',(2.64794488744246,1.,-3.23285778738558));
#55008=CARTESIAN_POINT('Ctrl Pts',(2.64083992182478,-1.,-3.2295608435934));
#55009=CARTESIAN_POINT('Ctrl Pts',(2.64083992182478,1.,-3.2295608435934));
#55010=CARTESIAN_POINT('Ctrl Pts',(2.63375697391438,-1.,-3.22623678292539));
#55011=CARTESIAN_POINT('Ctrl Pts',(2.63375697391438,1.,-3.22623678292539));
#55012=CARTESIAN_POINT('Ctrl Pts',(2.62669622735548,-1.,-3.222885536128));
#55013=CARTESIAN_POINT('Ctrl Pts',(2.62669622735548,1.,-3.222885536128));
#55014=CARTESIAN_POINT('Ctrl Pts',(2.61965792832396,-1.,-3.21950704108654));
#55015=CARTESIAN_POINT('Ctrl Pts',(2.61965792832396,1.,-3.21950704108654));
#55016=CARTESIAN_POINT('Ctrl Pts',(2.61264236718662,-1.,-3.21610123232465));
#55017=CARTESIAN_POINT('Ctrl Pts',(2.61264236718662,1.,-3.21610123232465));
#55018=CARTESIAN_POINT('Ctrl Pts',(2.60564985359699,-1.,-3.21266802609297));
#55019=CARTESIAN_POINT('Ctrl Pts',(2.60564985359699,1.,-3.21266802609297));
#55020=CARTESIAN_POINT('Ctrl Pts',(2.59868069194267,-1.,-3.2092073056959));
#55021=CARTESIAN_POINT('Ctrl Pts',(2.59868069194267,1.,-3.2092073056959));
#55022=CARTESIAN_POINT('Ctrl Pts',(2.59173516023605,-1.,-3.20571891028879));
#55023=CARTESIAN_POINT('Ctrl Pts',(2.59173516023605,1.,-3.20571891028879));
#55024=CARTESIAN_POINT('Ctrl Pts',(2.58481347777953,-1.,-3.20220261408685));
#55025=CARTESIAN_POINT('Ctrl Pts',(2.58481347777953,1.,-3.20220261408685));
#55026=CARTESIAN_POINT('Ctrl Pts',(2.577915819091,-1.,-3.19865814628955));
#55027=CARTESIAN_POINT('Ctrl Pts',(2.577915819091,1.,-3.19865814628955));
#55028=CARTESIAN_POINT('Ctrl Pts',(2.57104235898053,-1.,-3.19508523784548));
#55029=CARTESIAN_POINT('Ctrl Pts',(2.57104235898053,1.,-3.19508523784548));
#55030=CARTESIAN_POINT('Ctrl Pts',(2.56419331092909,-1.,-3.19148366395201));
#55031=CARTESIAN_POINT('Ctrl Pts',(2.56419331092909,1.,-3.19148366395201));
#55032=CARTESIAN_POINT('Ctrl Pts',(2.55736896206016,-1.,-3.1878532811617));
#55033=CARTESIAN_POINT('Ctrl Pts',(2.55736896206016,1.,-3.1878532811617));
#55034=CARTESIAN_POINT('Ctrl Pts',(2.55056972387638,-1.,-3.18419408529482));
#55035=CARTESIAN_POINT('Ctrl Pts',(2.55056972387638,1.,-3.18419408529482));
#55036=CARTESIAN_POINT('Ctrl Pts',(2.54379612552948,-1.,-3.18050619750515));
#55037=CARTESIAN_POINT('Ctrl Pts',(2.54379612552948,1.,-3.18050619750515));
#55038=CARTESIAN_POINT('Ctrl Pts',(2.53704871950871,-1.,-3.17678974135225));
#55039=CARTESIAN_POINT('Ctrl Pts',(2.53704871950871,1.,-3.17678974135225));
#55040=CARTESIAN_POINT('Ctrl Pts',(2.5303280040691,-1.,-3.17304474093574));
#55041=CARTESIAN_POINT('Ctrl Pts',(2.5303280040691,1.,-3.17304474093574));
#55042=CARTESIAN_POINT('Ctrl Pts',(2.523634346718,-1.,-3.16927102130751));
#55043=CARTESIAN_POINT('Ctrl Pts',(2.523634346718,1.,-3.16927102130751));
#55044=CARTESIAN_POINT('Ctrl Pts',(2.51696788755615,-1.,-3.16546808277069));
#55045=CARTESIAN_POINT('Ctrl Pts',(2.51696788755615,1.,-3.16546808277069));
#55046=CARTESIAN_POINT('Ctrl Pts',(2.51032851007939,-1.,-3.16163506380211));
#55047=CARTESIAN_POINT('Ctrl Pts',(2.51032851007939,1.,-3.16163506380211));
#55048=CARTESIAN_POINT('Ctrl Pts',(2.50371605688287,-1.,-3.15777102413998));
#55049=CARTESIAN_POINT('Ctrl Pts',(2.50371605688287,1.,-3.15777102413998));
#55050=CARTESIAN_POINT('Ctrl Pts',(2.49713050858911,-1.,-3.15387518039064));
#55051=CARTESIAN_POINT('Ctrl Pts',(2.49713050858911,1.,-3.15387518039064));
#55052=CARTESIAN_POINT('Ctrl Pts',(2.49057217131985,-1.,-3.14994715298903));
#55053=CARTESIAN_POINT('Ctrl Pts',(2.49057217131985,1.,-3.14994715298903));
#55054=CARTESIAN_POINT('Ctrl Pts',(2.48404187418376,-1.,-3.1459872272388));
#55055=CARTESIAN_POINT('Ctrl Pts',(2.48404187418376,1.,-3.1459872272388));
#55056=CARTESIAN_POINT('Ctrl Pts',(2.47754112428027,-1.,-3.14199655778845));
#55057=CARTESIAN_POINT('Ctrl Pts',(2.47754112428027,1.,-3.14199655778845));
#55058=CARTESIAN_POINT('Ctrl Pts',(2.47107164236827,-1.,-3.13797654408931));
#55059=CARTESIAN_POINT('Ctrl Pts',(2.47107164236827,1.,-3.13797654408931));
#55060=CARTESIAN_POINT('Ctrl Pts',(2.4646349433237,-1.,-3.13392826623902));
#55061=CARTESIAN_POINT('Ctrl Pts',(2.4646349433237,1.,-3.13392826623902));
#55062=CARTESIAN_POINT('Ctrl Pts',(2.45823188859366,-1.,-3.12985188384372));
#55063=CARTESIAN_POINT('Ctrl Pts',(2.45823188859366,1.,-3.12985188384372));
#55064=CARTESIAN_POINT('Ctrl Pts',(2.45186227369848,-1.,-3.12574608210849));
#55065=CARTESIAN_POINT('Ctrl Pts',(2.45186227369848,1.,-3.12574608210849));
#55066=CARTESIAN_POINT('Ctrl Pts',(2.44552433364716,-1.,-3.12160740887768));
#55067=CARTESIAN_POINT('Ctrl Pts',(2.44552433364716,1.,-3.12160740887768));
#55068=CARTESIAN_POINT('Ctrl Pts',(2.43921571477975,-1.,-3.11743156744182));
#55069=CARTESIAN_POINT('Ctrl Pts',(2.43921571477975,1.,-3.11743156744182));
#55070=CARTESIAN_POINT('Ctrl Pts',(2.4329344968514,-1.,-3.11321477659012));
#55071=CARTESIAN_POINT('Ctrl Pts',(2.4329344968514,1.,-3.11321477659012));
#55072=CARTESIAN_POINT('Ctrl Pts',(2.42668025870013,-1.,-3.10895518969592));
#55073=CARTESIAN_POINT('Ctrl Pts',(2.42668025870013,1.,-3.10895518969592));
#55074=CARTESIAN_POINT('Ctrl Pts',(2.42045498612494,-1.,-3.10465410280902));
#55075=CARTESIAN_POINT('Ctrl Pts',(2.42045498612494,1.,-3.10465410280902));
#55076=CARTESIAN_POINT('Ctrl Pts',(2.41426441798067,-1.,-3.10031775027683));
#55077=CARTESIAN_POINT('Ctrl Pts',(2.41426441798067,1.,-3.10031775027683));
#55078=CARTESIAN_POINT('Ctrl Pts',(2.40811612696382,-1.,-3.09595472616093));
#55079=CARTESIAN_POINT('Ctrl Pts',(2.40811612696382,1.,-3.09595472616093));
#55080=CARTESIAN_POINT('Ctrl Pts',(2.40201704423352,-1.,-3.09157266051115));
#55081=CARTESIAN_POINT('Ctrl Pts',(2.40201704423352,1.,-3.09157266051115));
#55082=CARTESIAN_POINT('Ctrl Pts',(2.39597098250635,-1.,-3.08717489512919));
#55083=CARTESIAN_POINT('Ctrl Pts',(2.39597098250635,1.,-3.08717489512919));
#55084=CARTESIAN_POINT('Ctrl Pts',(2.38997659219192,-1.,-3.08275773747083));
#55085=CARTESIAN_POINT('Ctrl Pts',(2.38997659219192,1.,-3.08275773747083));
#55086=CARTESIAN_POINT('Ctrl Pts',(2.38402401216107,-1.,-3.07830597244301));
#55087=CARTESIAN_POINT('Ctrl Pts',(2.38402401216107,1.,-3.07830597244301));
#55088=CARTESIAN_POINT('Ctrl Pts',(2.37809856205524,-1.,-3.07379777492133));
#55089=CARTESIAN_POINT('Ctrl Pts',(2.37809856205524,1.,-3.07379777492133));
#55090=CARTESIAN_POINT('Ctrl Pts',(2.37218678163157,-1.,-3.06921275497472));
#55091=CARTESIAN_POINT('Ctrl Pts',(2.37218678163157,1.,-3.06921275497472));
#55092=CARTESIAN_POINT('Ctrl Pts',(2.36628220107001,-1.,-3.06453964643152));
#55093=CARTESIAN_POINT('Ctrl Pts',(2.36628220107001,1.,-3.06453964643152));
#55094=CARTESIAN_POINT('Ctrl Pts',(2.36039011602084,-1.,-3.05978266240056));
#55095=CARTESIAN_POINT('Ctrl Pts',(2.36039011602084,1.,-3.05978266240056));
#55096=CARTESIAN_POINT('Ctrl Pts',(2.35453559889506,-1.,-3.05497218368188));
#55097=CARTESIAN_POINT('Ctrl Pts',(2.35453559889506,1.,-3.05497218368188));
#55098=CARTESIAN_POINT('Ctrl Pts',(2.34875673090816,-1.,-3.05015565829976));
#55099=CARTESIAN_POINT('Ctrl Pts',(2.34875673090816,1.,-3.05015565829976));
#55100=CARTESIAN_POINT('Ctrl Pts',(2.3430901708402,-1.,-3.04537822217311));
#55101=CARTESIAN_POINT('Ctrl Pts',(2.3430901708402,1.,-3.04537822217311));
#55102=CARTESIAN_POINT('Ctrl Pts',(2.33755792953726,-1.,-3.04066496998569));
#55103=CARTESIAN_POINT('Ctrl Pts',(2.33755792953726,1.,-3.04066496998569));
#55104=CARTESIAN_POINT('Ctrl Pts',(2.33215619079807,-1.,-3.03600588555765));
#55105=CARTESIAN_POINT('Ctrl Pts',(2.33215619079807,1.,-3.03600588555765));
#55106=CARTESIAN_POINT('Ctrl Pts',(2.32683687412027,-1.,-3.03133125185047));
#55107=CARTESIAN_POINT('Ctrl Pts',(2.32683687412027,1.,-3.03133125185047));
#55108=CARTESIAN_POINT('Ctrl Pts',(2.32151944306299,-1.,-3.02652678416478));
#55109=CARTESIAN_POINT('Ctrl Pts',(2.32151944306299,1.,-3.02652678416478));
#55110=CARTESIAN_POINT('Ctrl Pts',(2.31612479121528,-1.,-3.02147780668029));
#55111=CARTESIAN_POINT('Ctrl Pts',(2.31612479121528,1.,-3.02147780668029));
#55112=CARTESIAN_POINT('Ctrl Pts',(2.31060449886577,-1.,-3.01610726819019));
#55113=CARTESIAN_POINT('Ctrl Pts',(2.31060449886577,1.,-3.01610726819019));
#55114=CARTESIAN_POINT('Ctrl Pts',(2.30496809486528,-1.,-3.01041131063882));
#55115=CARTESIAN_POINT('Ctrl Pts',(2.30496809486528,1.,-3.01041131063882));
#55116=CARTESIAN_POINT('Ctrl Pts',(2.29932091315939,-1.,-3.00450832658822));
#55117=CARTESIAN_POINT('Ctrl Pts',(2.29932091315939,1.,-3.00450832658822));
#55118=CARTESIAN_POINT('Ctrl Pts',(2.29385894577999,-1.,-2.99863310340004));
#55119=CARTESIAN_POINT('Ctrl Pts',(2.29385894577999,1.,-2.99863310340004));
#55120=CARTESIAN_POINT('Ctrl Pts',(2.28882328690601,-1.,-2.9930793098434));
#55121=CARTESIAN_POINT('Ctrl Pts',(2.28882328690601,1.,-2.9930793098434));
#55122=CARTESIAN_POINT('Ctrl Pts',(2.28446419116036,-1.,-2.98815432734929));
#55123=CARTESIAN_POINT('Ctrl Pts',(2.28446419116036,1.,-2.98815432734929));
#55124=CARTESIAN_POINT('Ctrl Pts',(2.28100472516582,-1.,-2.98413343613858));
#55125=CARTESIAN_POINT('Ctrl Pts',(2.28100472516582,1.,-2.98413343613858));
#55126=CARTESIAN_POINT('Ctrl Pts',(2.2785960133424,-1.,-2.98120357932601));
#55127=CARTESIAN_POINT('Ctrl Pts',(2.2785960133424,1.,-2.98120357932601));
#55128=CARTESIAN_POINT('Ctrl Pts',(2.27756633754846,-1.,-2.97980276182744));
#55129=CARTESIAN_POINT('Ctrl Pts',(2.27756633754846,1.,-2.97980276182744));
#55130=CARTESIAN_POINT('Ctrl Pts',(2.27730961189188,-1.,-2.97929608861502));
#55131=CARTESIAN_POINT('Ctrl Pts',(2.27730961189188,1.,-2.97929608861502));
#55132=CARTESIAN_POINT('Ctrl Pts',(2.2773674298423,-1.,-2.97919987915565));
#55133=CARTESIAN_POINT('Ctrl Pts',(2.2773674298423,1.,-2.97919987915565));
#55134=CARTESIAN_POINT('Ctrl Pts',(2.27745358485296,-1.,-2.97921217251145));
#55135=CARTESIAN_POINT('Ctrl Pts',(2.27745358485296,1.,-2.97921217251145));
#55136=CARTESIAN_POINT('',(2.66939624221984,1.,-3.24257979115744));
#55137=CARTESIAN_POINT('Ctrl Pts',(2.66939624221984,1.,-3.24257979115744));
#55138=CARTESIAN_POINT('Ctrl Pts',(2.66795998539861,1.,-3.24193929584813));
#55139=CARTESIAN_POINT('Ctrl Pts',(2.66508964664767,1.,-3.24065561087681));
#55140=CARTESIAN_POINT('Ctrl Pts',(2.6607906631973,1.,-3.23872200036311));
#55141=CARTESIAN_POINT('Ctrl Pts',(2.6550717396303,1.,-3.23612768065687));
#55142=CARTESIAN_POINT('Ctrl Pts',(2.64794488744246,1.,-3.23285778738558));
#55143=CARTESIAN_POINT('Ctrl Pts',(2.64083992182478,1.,-3.2295608435934));
#55144=CARTESIAN_POINT('Ctrl Pts',(2.63375697391438,1.,-3.22623678292539));
#55145=CARTESIAN_POINT('Ctrl Pts',(2.62669622735548,1.,-3.222885536128));
#55146=CARTESIAN_POINT('Ctrl Pts',(2.61965792832396,1.,-3.21950704108654));
#55147=CARTESIAN_POINT('Ctrl Pts',(2.61264236718662,1.,-3.21610123232465));
#55148=CARTESIAN_POINT('Ctrl Pts',(2.60564985359699,1.,-3.21266802609297));
#55149=CARTESIAN_POINT('Ctrl Pts',(2.59868069194267,1.,-3.2092073056959));
#55150=CARTESIAN_POINT('Ctrl Pts',(2.59173516023605,1.,-3.20571891028879));
#55151=CARTESIAN_POINT('Ctrl Pts',(2.58481347777953,1.,-3.20220261408685));
#55152=CARTESIAN_POINT('Ctrl Pts',(2.577915819091,1.,-3.19865814628955));
#55153=CARTESIAN_POINT('Ctrl Pts',(2.57104235898053,1.,-3.19508523784548));
#55154=CARTESIAN_POINT('Ctrl Pts',(2.56419331092909,1.,-3.19148366395201));
#55155=CARTESIAN_POINT('Ctrl Pts',(2.55736896206016,1.,-3.1878532811617));
#55156=CARTESIAN_POINT('Ctrl Pts',(2.55056972387638,1.,-3.18419408529482));
#55157=CARTESIAN_POINT('Ctrl Pts',(2.54379612552948,1.,-3.18050619750515));
#55158=CARTESIAN_POINT('Ctrl Pts',(2.53704871950871,1.,-3.17678974135225));
#55159=CARTESIAN_POINT('Ctrl Pts',(2.5303280040691,1.,-3.17304474093574));
#55160=CARTESIAN_POINT('Ctrl Pts',(2.523634346718,1.,-3.16927102130751));
#55161=CARTESIAN_POINT('Ctrl Pts',(2.51696788755615,1.,-3.16546808277069));
#55162=CARTESIAN_POINT('Ctrl Pts',(2.51032851007939,1.,-3.16163506380211));
#55163=CARTESIAN_POINT('Ctrl Pts',(2.50371605688287,1.,-3.15777102413998));
#55164=CARTESIAN_POINT('Ctrl Pts',(2.49713050858911,1.,-3.15387518039064));
#55165=CARTESIAN_POINT('Ctrl Pts',(2.49057217131985,1.,-3.14994715298903));
#55166=CARTESIAN_POINT('Ctrl Pts',(2.48404187418376,1.,-3.1459872272388));
#55167=CARTESIAN_POINT('Ctrl Pts',(2.47754112428027,1.,-3.14199655778845));
#55168=CARTESIAN_POINT('Ctrl Pts',(2.47107164236827,1.,-3.13797654408931));
#55169=CARTESIAN_POINT('Ctrl Pts',(2.4646349433237,1.,-3.13392826623902));
#55170=CARTESIAN_POINT('Ctrl Pts',(2.45823188859366,1.,-3.12985188384372));
#55171=CARTESIAN_POINT('Ctrl Pts',(2.45186227369848,1.,-3.12574608210849));
#55172=CARTESIAN_POINT('Ctrl Pts',(2.44552433364716,1.,-3.12160740887768));
#55173=CARTESIAN_POINT('Ctrl Pts',(2.43921571477975,1.,-3.11743156744182));
#55174=CARTESIAN_POINT('Ctrl Pts',(2.4329344968514,1.,-3.11321477659012));
#55175=CARTESIAN_POINT('Ctrl Pts',(2.42668025870013,1.,-3.10895518969592));
#55176=CARTESIAN_POINT('Ctrl Pts',(2.42045498612494,1.,-3.10465410280902));
#55177=CARTESIAN_POINT('Ctrl Pts',(2.41426441798067,1.,-3.10031775027683));
#55178=CARTESIAN_POINT('Ctrl Pts',(2.40811612696382,1.,-3.09595472616093));
#55179=CARTESIAN_POINT('Ctrl Pts',(2.40201704423352,1.,-3.09157266051115));
#55180=CARTESIAN_POINT('Ctrl Pts',(2.39597098250635,1.,-3.08717489512919));
#55181=CARTESIAN_POINT('Ctrl Pts',(2.38997659219192,1.,-3.08275773747083));
#55182=CARTESIAN_POINT('Ctrl Pts',(2.38402401216107,1.,-3.07830597244301));
#55183=CARTESIAN_POINT('Ctrl Pts',(2.37809856205524,1.,-3.07379777492133));
#55184=CARTESIAN_POINT('Ctrl Pts',(2.37218678163157,1.,-3.06921275497472));
#55185=CARTESIAN_POINT('Ctrl Pts',(2.36628220107001,1.,-3.06453964643152));
#55186=CARTESIAN_POINT('Ctrl Pts',(2.36039011602084,1.,-3.05978266240056));
#55187=CARTESIAN_POINT('Ctrl Pts',(2.35453559889506,1.,-3.05497218368188));
#55188=CARTESIAN_POINT('Ctrl Pts',(2.34875673090816,1.,-3.05015565829976));
#55189=CARTESIAN_POINT('Ctrl Pts',(2.3430901708402,1.,-3.04537822217311));
#55190=CARTESIAN_POINT('Ctrl Pts',(2.33755792953726,1.,-3.04066496998569));
#55191=CARTESIAN_POINT('Ctrl Pts',(2.33215619079807,1.,-3.03600588555765));
#55192=CARTESIAN_POINT('Ctrl Pts',(2.32683687412027,1.,-3.03133125185047));
#55193=CARTESIAN_POINT('Ctrl Pts',(2.32151944306299,1.,-3.02652678416478));
#55194=CARTESIAN_POINT('Ctrl Pts',(2.31612479121528,1.,-3.02147780668029));
#55195=CARTESIAN_POINT('Ctrl Pts',(2.31060449886577,1.,-3.01610726819019));
#55196=CARTESIAN_POINT('Ctrl Pts',(2.30496809486528,1.,-3.01041131063882));
#55197=CARTESIAN_POINT('Ctrl Pts',(2.29932091315939,1.,-3.00450832658822));
#55198=CARTESIAN_POINT('Ctrl Pts',(2.29385894577999,1.,-2.99863310340004));
#55199=CARTESIAN_POINT('Ctrl Pts',(2.28882328690601,1.,-2.9930793098434));
#55200=CARTESIAN_POINT('Ctrl Pts',(2.28446419116036,1.,-2.98815432734929));
#55201=CARTESIAN_POINT('Ctrl Pts',(2.28100472516582,1.,-2.98413343613858));
#55202=CARTESIAN_POINT('Ctrl Pts',(2.27877674853833,1.,-2.98142341809623));
#55203=CARTESIAN_POINT('Ctrl Pts',(2.27776738270369,1.,-2.98007383024333));
#55204=CARTESIAN_POINT('Ctrl Pts',(2.27743009389704,1.,-2.97951167106106));
#55205=CARTESIAN_POINT('Ctrl Pts',(2.27737238849212,1.,-2.97932307137589));
#55206=CARTESIAN_POINT('Ctrl Pts',(2.27737254473378,1.,-2.97927412174388));
#55207=CARTESIAN_POINT('',(2.66939624221984,0.,-3.24257979115744));
#55208=CARTESIAN_POINT('Ctrl Pts',(2.58626089374824,-1.,-2.71546581445404));
#55209=CARTESIAN_POINT('Ctrl Pts',(2.58626089374824,1.,-2.71546581445404));
#55210=CARTESIAN_POINT('Ctrl Pts',(2.58626222935803,-1.,-2.71537879705104));
#55211=CARTESIAN_POINT('Ctrl Pts',(2.58626222935803,1.,-2.71537879705104));
#55212=CARTESIAN_POINT('Ctrl Pts',(2.58636629904103,-1.,-2.71533674141254));
#55213=CARTESIAN_POINT('Ctrl Pts',(2.58636629904103,1.,-2.71533674141254));
#55214=CARTESIAN_POINT('Ctrl Pts',(2.5868265735259,-1.,-2.71566956750452));
#55215=CARTESIAN_POINT('Ctrl Pts',(2.5868265735259,1.,-2.71566956750452));
#55216=CARTESIAN_POINT('Ctrl Pts',(2.58804906785417,-1.,-2.71690570241638));
#55217=CARTESIAN_POINT('Ctrl Pts',(2.58804906785417,1.,-2.71690570241638));
#55218=CARTESIAN_POINT('Ctrl Pts',(2.59056604771971,-1.,-2.71974308958086));
#55219=CARTESIAN_POINT('Ctrl Pts',(2.59056604771971,1.,-2.71974308958086));
#55220=CARTESIAN_POINT('Ctrl Pts',(2.59399625537278,-1.,-2.72378896977134));
#55221=CARTESIAN_POINT('Ctrl Pts',(2.59399625537278,1.,-2.72378896977134));
#55222=CARTESIAN_POINT('Ctrl Pts',(2.59817869034746,-1.,-2.7288648348152));
#55223=CARTESIAN_POINT('Ctrl Pts',(2.59817869034746,1.,-2.7288648348152));
#55224=CARTESIAN_POINT('Ctrl Pts',(2.60287635688728,-1.,-2.73470730109615));
#55225=CARTESIAN_POINT('Ctrl Pts',(2.60287635688728,1.,-2.73470730109615));
#55226=CARTESIAN_POINT('Ctrl Pts',(2.60782480638448,-1.,-2.7410211099909));
#55227=CARTESIAN_POINT('Ctrl Pts',(2.60782480638448,1.,-2.7410211099909));
#55228=CARTESIAN_POINT('Ctrl Pts',(2.61277170105813,-1.,-2.74752219567252));
#55229=CARTESIAN_POINT('Ctrl Pts',(2.61277170105813,1.,-2.74752219567252));
#55230=CARTESIAN_POINT('Ctrl Pts',(2.61751580407667,-1.,-2.7539802502603));
#55231=CARTESIAN_POINT('Ctrl Pts',(2.61751580407667,1.,-2.7539802502603));
#55232=CARTESIAN_POINT('Ctrl Pts',(2.62195665834605,-1.,-2.76027271596686));
#55233=CARTESIAN_POINT('Ctrl Pts',(2.62195665834605,1.,-2.76027271596686));
#55234=CARTESIAN_POINT('Ctrl Pts',(2.62609956506355,-1.,-2.76639078479021));
#55235=CARTESIAN_POINT('Ctrl Pts',(2.62609956506355,1.,-2.76639078479021));
#55236=CARTESIAN_POINT('Ctrl Pts',(2.63001305229625,-1.,-2.77239433377921));
#55237=CARTESIAN_POINT('Ctrl Pts',(2.63001305229625,1.,-2.77239433377921));
#55238=CARTESIAN_POINT('Ctrl Pts',(2.63379800904599,-1.,-2.77837943466449));
#55239=CARTESIAN_POINT('Ctrl Pts',(2.63379800904599,1.,-2.77837943466449));
#55240=CARTESIAN_POINT('Ctrl Pts',(2.637554714303,-1.,-2.78444351041571));
#55241=CARTESIAN_POINT('Ctrl Pts',(2.637554714303,1.,-2.78444351041571));
#55242=CARTESIAN_POINT('Ctrl Pts',(2.64134450532584,-1.,-2.79064495573224));
#55243=CARTESIAN_POINT('Ctrl Pts',(2.64134450532584,1.,-2.79064495573224));
#55244=CARTESIAN_POINT('Ctrl Pts',(2.64517667799319,-1.,-2.79698910670736));
#55245=CARTESIAN_POINT('Ctrl Pts',(2.64517667799319,1.,-2.79698910670736));
#55246=CARTESIAN_POINT('Ctrl Pts',(2.64902988983337,-1.,-2.80345029781152));
#55247=CARTESIAN_POINT('Ctrl Pts',(2.64902988983337,1.,-2.80345029781152));
#55248=CARTESIAN_POINT('Ctrl Pts',(2.65286529532208,-1.,-2.80998526078165));
#55249=CARTESIAN_POINT('Ctrl Pts',(2.65286529532208,1.,-2.80998526078165));
#55250=CARTESIAN_POINT('Ctrl Pts',(2.65664198781344,-1.,-2.81654896073883));
#55251=CARTESIAN_POINT('Ctrl Pts',(2.65664198781344,1.,-2.81654896073883));
#55252=CARTESIAN_POINT('Ctrl Pts',(2.66033388273461,-1.,-2.82311188135078));
#55253=CARTESIAN_POINT('Ctrl Pts',(2.66033388273461,1.,-2.82311188135078));
#55254=CARTESIAN_POINT('Ctrl Pts',(2.6639376472693,-1.,-2.82966813308998));
#55255=CARTESIAN_POINT('Ctrl Pts',(2.6639376472693,1.,-2.82966813308998));
#55256=CARTESIAN_POINT('Ctrl Pts',(2.66746339678107,-1.,-2.83622586853982));
#55257=CARTESIAN_POINT('Ctrl Pts',(2.66746339678107,1.,-2.83622586853982));
#55258=CARTESIAN_POINT('Ctrl Pts',(2.67092916452125,-1.,-2.84280157191323));
#55259=CARTESIAN_POINT('Ctrl Pts',(2.67092916452125,1.,-2.84280157191323));
#55260=CARTESIAN_POINT('Ctrl Pts',(2.67435421039677,-1.,-2.84941315703092));
#55261=CARTESIAN_POINT('Ctrl Pts',(2.67435421039677,1.,-2.84941315703092));
#55262=CARTESIAN_POINT('Ctrl Pts',(2.67775201955724,-1.,-2.85607274378018));
#55263=CARTESIAN_POINT('Ctrl Pts',(2.67775201955724,1.,-2.85607274378018));
#55264=CARTESIAN_POINT('Ctrl Pts',(2.68112602796308,-1.,-2.86278224277689));
#55265=CARTESIAN_POINT('Ctrl Pts',(2.68112602796308,1.,-2.86278224277689));
#55266=CARTESIAN_POINT('Ctrl Pts',(2.68447353139599,-1.,-2.86953736547238));
#55267=CARTESIAN_POINT('Ctrl Pts',(2.68447353139599,1.,-2.86953736547238));
#55268=CARTESIAN_POINT('Ctrl Pts',(2.68778807801686,-1.,-2.8763300724388));
#55269=CARTESIAN_POINT('Ctrl Pts',(2.68778807801686,1.,-2.8763300724388));
#55270=CARTESIAN_POINT('Ctrl Pts',(2.69106236420198,-1.,-2.88315153980466));
#55271=CARTESIAN_POINT('Ctrl Pts',(2.69106236420198,1.,-2.88315153980466));
#55272=CARTESIAN_POINT('Ctrl Pts',(2.69429113011374,-1.,-2.88999512410309));
#55273=CARTESIAN_POINT('Ctrl Pts',(2.69429113011374,1.,-2.88999512410309));
#55274=CARTESIAN_POINT('Ctrl Pts',(2.69747340630625,-1.,-2.89685866123671));
#55275=CARTESIAN_POINT('Ctrl Pts',(2.69747340630625,1.,-2.89685866123671));
#55276=CARTESIAN_POINT('Ctrl Pts',(2.70061095078692,-1.,-2.90374285605838));
#55277=CARTESIAN_POINT('Ctrl Pts',(2.70061095078692,1.,-2.90374285605838));
#55278=CARTESIAN_POINT('Ctrl Pts',(2.70370719782113,-1.,-2.91065019668329));
#55279=CARTESIAN_POINT('Ctrl Pts',(2.70370719782113,1.,-2.91065019668329));
#55280=CARTESIAN_POINT('Ctrl Pts',(2.70676602302518,-1.,-2.91758367994737));
#55281=CARTESIAN_POINT('Ctrl Pts',(2.70676602302518,1.,-2.91758367994737));
#55282=CARTESIAN_POINT('Ctrl Pts',(2.70979055994754,-1.,-2.92454558914778));
#55283=CARTESIAN_POINT('Ctrl Pts',(2.70979055994754,1.,-2.92454558914778));
#55284=CARTESIAN_POINT('Ctrl Pts',(2.71278207520817,-1.,-2.93153633192595));
#55285=CARTESIAN_POINT('Ctrl Pts',(2.71278207520817,1.,-2.93153633192595));
#55286=CARTESIAN_POINT('Ctrl Pts',(2.7157405459259,-1.,-2.93855503247266));
#55287=CARTESIAN_POINT('Ctrl Pts',(2.7157405459259,1.,-2.93855503247266));
#55288=CARTESIAN_POINT('Ctrl Pts',(2.71866514227965,-1.,-2.94560002559806));
#55289=CARTESIAN_POINT('Ctrl Pts',(2.71866514227965,1.,-2.94560002559806));
#55290=CARTESIAN_POINT('Ctrl Pts',(2.72155475123364,-1.,-2.95266939280621));
#55291=CARTESIAN_POINT('Ctrl Pts',(2.72155475123364,1.,-2.95266939280621));
#55292=CARTESIAN_POINT('Ctrl Pts',(2.72440846811729,-1.,-2.95976146492576));
#55293=CARTESIAN_POINT('Ctrl Pts',(2.72440846811729,1.,-2.95976146492576));
#55294=CARTESIAN_POINT('Ctrl Pts',(2.72722614084076,-1.,-2.96687537842451));
#55295=CARTESIAN_POINT('Ctrl Pts',(2.72722614084076,1.,-2.96687537842451));
#55296=CARTESIAN_POINT('Ctrl Pts',(2.73000819218414,-1.,-2.97401089032677));
#55297=CARTESIAN_POINT('Ctrl Pts',(2.73000819218414,1.,-2.97401089032677));
#55298=CARTESIAN_POINT('Ctrl Pts',(2.73275539286497,-1.,-2.98116814232129));
#55299=CARTESIAN_POINT('Ctrl Pts',(2.73275539286497,1.,-2.98116814232129));
#55300=CARTESIAN_POINT('Ctrl Pts',(2.73546864694536,-1.,-2.9883474369644));
#55301=CARTESIAN_POINT('Ctrl Pts',(2.73546864694536,1.,-2.9883474369644));
#55302=CARTESIAN_POINT('Ctrl Pts',(2.73814878711641,-1.,-2.99554902409778));
#55303=CARTESIAN_POINT('Ctrl Pts',(2.73814878711641,1.,-2.99554902409778));
#55304=CARTESIAN_POINT('Ctrl Pts',(2.74079632883931,-1.,-3.00277284351521));
#55305=CARTESIAN_POINT('Ctrl Pts',(2.74079632883931,1.,-3.00277284351521));
#55306=CARTESIAN_POINT('Ctrl Pts',(2.74341150239887,-1.,-3.01001855960162));
#55307=CARTESIAN_POINT('Ctrl Pts',(2.74341150239887,1.,-3.01001855960162));
#55308=CARTESIAN_POINT('Ctrl Pts',(2.74599436193625,-1.,-3.01728567646611));
#55309=CARTESIAN_POINT('Ctrl Pts',(2.74599436193625,1.,-3.01728567646611));
#55310=CARTESIAN_POINT('Ctrl Pts',(2.7485448718414,-1.,-3.02457362909245));
#55311=CARTESIAN_POINT('Ctrl Pts',(2.7485448718414,1.,-3.02457362909245));
#55312=CARTESIAN_POINT('Ctrl Pts',(2.75106299522979,-1.,-3.03188187589107));
#55313=CARTESIAN_POINT('Ctrl Pts',(2.75106299522979,1.,-3.03188187589107));
#55314=CARTESIAN_POINT('Ctrl Pts',(2.75354880060314,-1.,-3.03921001107977));
#55315=CARTESIAN_POINT('Ctrl Pts',(2.75354880060314,1.,-3.03921001107977));
#55316=CARTESIAN_POINT('Ctrl Pts',(2.75600247455925,-1.,-3.04655777351067));
#55317=CARTESIAN_POINT('Ctrl Pts',(2.75600247455925,1.,-3.04655777351067));
#55318=CARTESIAN_POINT('Ctrl Pts',(2.75842427252931,-1.,-3.05392498749847));
#55319=CARTESIAN_POINT('Ctrl Pts',(2.75842427252931,1.,-3.05392498749847));
#55320=CARTESIAN_POINT('Ctrl Pts',(2.76081448759882,-1.,-3.06131152247454));
#55321=CARTESIAN_POINT('Ctrl Pts',(2.76081448759882,1.,-3.06131152247454));
#55322=CARTESIAN_POINT('Ctrl Pts',(2.76317341453493,-1.,-3.0687172484321));
#55323=CARTESIAN_POINT('Ctrl Pts',(2.76317341453493,1.,-3.0687172484321));
#55324=CARTESIAN_POINT('Ctrl Pts',(2.76550131064852,-1.,-3.07614198408862));
#55325=CARTESIAN_POINT('Ctrl Pts',(2.76550131064852,1.,-3.07614198408862));
#55326=CARTESIAN_POINT('Ctrl Pts',(2.76779837829373,-1.,-3.08358548001504));
#55327=CARTESIAN_POINT('Ctrl Pts',(2.76779837829373,1.,-3.08358548001504));
#55328=CARTESIAN_POINT('Ctrl Pts',(2.7700647803451,-1.,-3.09104745382531));
#55329=CARTESIAN_POINT('Ctrl Pts',(2.7700647803451,1.,-3.09104745382531));
#55330=CARTESIAN_POINT('Ctrl Pts',(2.77230064796057,-1.,-3.0985276127786));
#55331=CARTESIAN_POINT('Ctrl Pts',(2.77230064796057,1.,-3.0985276127786));
#55332=CARTESIAN_POINT('Ctrl Pts',(2.77450609123362,-1.,-3.10602568032564));
#55333=CARTESIAN_POINT('Ctrl Pts',(2.77450609123362,1.,-3.10602568032564));
#55334=CARTESIAN_POINT('Ctrl Pts',(2.77668121002545,-1.,-3.11354142303921));
#55335=CARTESIAN_POINT('Ctrl Pts',(2.77668121002545,1.,-3.11354142303921));
#55336=CARTESIAN_POINT('Ctrl Pts',(2.77882610146731,-1.,-3.12107467037201));
#55337=CARTESIAN_POINT('Ctrl Pts',(2.77882610146731,1.,-3.12107467037201));
#55338=CARTESIAN_POINT('Ctrl Pts',(2.78094085161413,-1.,-3.12862530318457));
#55339=CARTESIAN_POINT('Ctrl Pts',(2.78094085161413,1.,-3.12862530318457));
#55340=CARTESIAN_POINT('Ctrl Pts',(2.78260859419319,-1.,-3.13467965833037));
#55341=CARTESIAN_POINT('Ctrl Pts',(2.78260859419319,1.,-3.13467965833037));
#55342=CARTESIAN_POINT('Ctrl Pts',(2.78384588958165,-1.,-3.13922819749279));
#55343=CARTESIAN_POINT('Ctrl Pts',(2.78384588958165,1.,-3.13922819749279));
#55344=CARTESIAN_POINT('Ctrl Pts',(2.7846647503589,-1.,-3.14226401018816));
#55345=CARTESIAN_POINT('Ctrl Pts',(2.7846647503589,1.,-3.14226401018816));
#55346=CARTESIAN_POINT('Ctrl Pts',(2.78507268004356,-1.,-3.14378277984898));
#55347=CARTESIAN_POINT('Ctrl Pts',(2.78507268004356,1.,-3.14378277984898));
#55348=CARTESIAN_POINT('',(2.58633475774921,1.,-2.71539546306948));
#55349=CARTESIAN_POINT('Ctrl Pts',(2.58633475774921,-1.,-2.71539546306948));
#55350=CARTESIAN_POINT('Ctrl Pts',(2.58633475774921,-0.666666666666667,
-2.71539546306948));
#55351=CARTESIAN_POINT('Ctrl Pts',(2.58633475774921,-0.333333333333333,
-2.71539546306948));
#55352=CARTESIAN_POINT('Ctrl Pts',(2.58633475774921,0.333333333333333,-2.71539546306948));
#55353=CARTESIAN_POINT('Ctrl Pts',(2.58633475774921,0.666666666666667,-2.71539546306948));
#55354=CARTESIAN_POINT('Ctrl Pts',(2.58633475774921,1.,-2.71539546306948));
#55355=CARTESIAN_POINT('',(2.78507268004356,1.,-3.14378277984898));
#55356=CARTESIAN_POINT('',(2.78507268004356,0.,-3.14378277984898));
#55357=CARTESIAN_POINT('Ctrl Pts',(2.58633475774921,1.,-2.71539546306948));
#55358=CARTESIAN_POINT('Ctrl Pts',(2.58638312917168,1.,-2.71540296616024));
#55359=CARTESIAN_POINT('Ctrl Pts',(2.58656037976753,1.,-2.71548946460575));
#55360=CARTESIAN_POINT('Ctrl Pts',(2.58706285424358,1.,-2.71591054189786));
#55361=CARTESIAN_POINT('Ctrl Pts',(2.58823792682672,1.,-2.71711860281815));
#55362=CARTESIAN_POINT('Ctrl Pts',(2.59056604771971,1.,-2.71974308958086));
#55363=CARTESIAN_POINT('Ctrl Pts',(2.59399625537278,1.,-2.72378896977134));
#55364=CARTESIAN_POINT('Ctrl Pts',(2.59817869034746,1.,-2.7288648348152));
#55365=CARTESIAN_POINT('Ctrl Pts',(2.60287635688728,1.,-2.73470730109615));
#55366=CARTESIAN_POINT('Ctrl Pts',(2.60782480638448,1.,-2.7410211099909));
#55367=CARTESIAN_POINT('Ctrl Pts',(2.61277170105813,1.,-2.74752219567252));
#55368=CARTESIAN_POINT('Ctrl Pts',(2.61751580407667,1.,-2.7539802502603));
#55369=CARTESIAN_POINT('Ctrl Pts',(2.62195665834605,1.,-2.76027271596686));
#55370=CARTESIAN_POINT('Ctrl Pts',(2.62609956506355,1.,-2.76639078479021));
#55371=CARTESIAN_POINT('Ctrl Pts',(2.63001305229625,1.,-2.77239433377921));
#55372=CARTESIAN_POINT('Ctrl Pts',(2.63379800904599,1.,-2.77837943466449));
#55373=CARTESIAN_POINT('Ctrl Pts',(2.637554714303,1.,-2.78444351041571));
#55374=CARTESIAN_POINT('Ctrl Pts',(2.64134450532584,1.,-2.79064495573224));
#55375=CARTESIAN_POINT('Ctrl Pts',(2.64517667799319,1.,-2.79698910670736));
#55376=CARTESIAN_POINT('Ctrl Pts',(2.64902988983337,1.,-2.80345029781152));
#55377=CARTESIAN_POINT('Ctrl Pts',(2.65286529532208,1.,-2.80998526078165));
#55378=CARTESIAN_POINT('Ctrl Pts',(2.65664198781344,1.,-2.81654896073883));
#55379=CARTESIAN_POINT('Ctrl Pts',(2.66033388273461,1.,-2.82311188135078));
#55380=CARTESIAN_POINT('Ctrl Pts',(2.6639376472693,1.,-2.82966813308998));
#55381=CARTESIAN_POINT('Ctrl Pts',(2.66746339678107,1.,-2.83622586853982));
#55382=CARTESIAN_POINT('Ctrl Pts',(2.67092916452125,1.,-2.84280157191323));
#55383=CARTESIAN_POINT('Ctrl Pts',(2.67435421039677,1.,-2.84941315703092));
#55384=CARTESIAN_POINT('Ctrl Pts',(2.67775201955724,1.,-2.85607274378018));
#55385=CARTESIAN_POINT('Ctrl Pts',(2.68112602796308,1.,-2.86278224277689));
#55386=CARTESIAN_POINT('Ctrl Pts',(2.68447353139599,1.,-2.86953736547238));
#55387=CARTESIAN_POINT('Ctrl Pts',(2.68778807801686,1.,-2.8763300724388));
#55388=CARTESIAN_POINT('Ctrl Pts',(2.69106236420198,1.,-2.88315153980466));
#55389=CARTESIAN_POINT('Ctrl Pts',(2.69429113011374,1.,-2.88999512410309));
#55390=CARTESIAN_POINT('Ctrl Pts',(2.69747340630625,1.,-2.89685866123671));
#55391=CARTESIAN_POINT('Ctrl Pts',(2.70061095078692,1.,-2.90374285605838));
#55392=CARTESIAN_POINT('Ctrl Pts',(2.70370719782113,1.,-2.91065019668329));
#55393=CARTESIAN_POINT('Ctrl Pts',(2.70676602302518,1.,-2.91758367994737));
#55394=CARTESIAN_POINT('Ctrl Pts',(2.70979055994754,1.,-2.92454558914778));
#55395=CARTESIAN_POINT('Ctrl Pts',(2.71278207520817,1.,-2.93153633192595));
#55396=CARTESIAN_POINT('Ctrl Pts',(2.7157405459259,1.,-2.93855503247266));
#55397=CARTESIAN_POINT('Ctrl Pts',(2.71866514227965,1.,-2.94560002559806));
#55398=CARTESIAN_POINT('Ctrl Pts',(2.72155475123364,1.,-2.95266939280621));
#55399=CARTESIAN_POINT('Ctrl Pts',(2.72440846811729,1.,-2.95976146492576));
#55400=CARTESIAN_POINT('Ctrl Pts',(2.72722614084076,1.,-2.96687537842451));
#55401=CARTESIAN_POINT('Ctrl Pts',(2.73000819218414,1.,-2.97401089032677));
#55402=CARTESIAN_POINT('Ctrl Pts',(2.73275539286497,1.,-2.98116814232129));
#55403=CARTESIAN_POINT('Ctrl Pts',(2.73546864694536,1.,-2.9883474369644));
#55404=CARTESIAN_POINT('Ctrl Pts',(2.73814878711641,1.,-2.99554902409778));
#55405=CARTESIAN_POINT('Ctrl Pts',(2.74079632883931,1.,-3.00277284351521));
#55406=CARTESIAN_POINT('Ctrl Pts',(2.74341150239887,1.,-3.01001855960162));
#55407=CARTESIAN_POINT('Ctrl Pts',(2.74599436193625,1.,-3.01728567646611));
#55408=CARTESIAN_POINT('Ctrl Pts',(2.7485448718414,1.,-3.02457362909245));
#55409=CARTESIAN_POINT('Ctrl Pts',(2.75106299522979,1.,-3.03188187589107));
#55410=CARTESIAN_POINT('Ctrl Pts',(2.75354880060314,1.,-3.03921001107977));
#55411=CARTESIAN_POINT('Ctrl Pts',(2.75600247455925,1.,-3.04655777351067));
#55412=CARTESIAN_POINT('Ctrl Pts',(2.75842427252931,1.,-3.05392498749847));
#55413=CARTESIAN_POINT('Ctrl Pts',(2.76081448759882,1.,-3.06131152247454));
#55414=CARTESIAN_POINT('Ctrl Pts',(2.76317341453493,1.,-3.0687172484321));
#55415=CARTESIAN_POINT('Ctrl Pts',(2.76550131064852,1.,-3.07614198408862));
#55416=CARTESIAN_POINT('Ctrl Pts',(2.76779837829373,1.,-3.08358548001504));
#55417=CARTESIAN_POINT('Ctrl Pts',(2.7700647803451,1.,-3.09104745382531));
#55418=CARTESIAN_POINT('Ctrl Pts',(2.77230064796057,1.,-3.0985276127786));
#55419=CARTESIAN_POINT('Ctrl Pts',(2.77450609123362,1.,-3.10602568032564));
#55420=CARTESIAN_POINT('Ctrl Pts',(2.77668121002545,1.,-3.11354142303921));
#55421=CARTESIAN_POINT('Ctrl Pts',(2.77882610146731,1.,-3.12107467037201));
#55422=CARTESIAN_POINT('Ctrl Pts',(2.78094085161413,1.,-3.12862530318457));
#55423=CARTESIAN_POINT('Ctrl Pts',(2.78260859419319,1.,-3.13467965833037));
#55424=CARTESIAN_POINT('Ctrl Pts',(2.78384588958165,1.,-3.13922819749279));
#55425=CARTESIAN_POINT('Ctrl Pts',(2.7846647503589,1.,-3.14226401018816));
#55426=CARTESIAN_POINT('Ctrl Pts',(2.78507268004356,1.,-3.14378277984898));
#55427=CARTESIAN_POINT('Origin',(2.78507268004356,0.,-3.14378277984898));
#55428=CARTESIAN_POINT('',(2.66939624221984,1.,-3.24257979115744));
#55429=CARTESIAN_POINT('Origin',(0.,0.,0.));
#55430=CARTESIAN_POINT('',(2.71539546306824,1.,-2.58633475775051));
#55431=CARTESIAN_POINT('Origin',(0.,1.,0.));
#55432=CARTESIAN_POINT('Ctrl Pts',(2.71539546306824,1.,-2.58633475775051));
#55433=CARTESIAN_POINT('Ctrl Pts',(2.71539546306824,0.666666666666667,-2.58633475775051));
#55434=CARTESIAN_POINT('Ctrl Pts',(2.71539546306824,0.333333333333333,-2.58633475775051));
#55435=CARTESIAN_POINT('Ctrl Pts',(2.71539546306824,-0.333333333333333,
-2.58633475775051));
#55436=CARTESIAN_POINT('Ctrl Pts',(2.71539546306824,-0.666666666666667,
-2.58633475775051));
#55437=CARTESIAN_POINT('Ctrl Pts',(2.71539546306824,-1.,-2.58633475775051));
#55438=CARTESIAN_POINT('Ctrl Pts',(3.14378277984898,-1.,-2.78507268004356));
#55439=CARTESIAN_POINT('Ctrl Pts',(3.14378277984898,1.,-2.78507268004356));
#55440=CARTESIAN_POINT('Ctrl Pts',(3.14226401019149,-1.,-2.78466475036183));
#55441=CARTESIAN_POINT('Ctrl Pts',(3.14226401019149,1.,-2.78466475036183));
#55442=CARTESIAN_POINT('Ctrl Pts',(3.13922819750185,-1.,-2.78384588958965));
#55443=CARTESIAN_POINT('Ctrl Pts',(3.13922819750185,1.,-2.78384588958965));
#55444=CARTESIAN_POINT('Ctrl Pts',(3.1346796583452,-1.,-2.78260859420629));
#55445=CARTESIAN_POINT('Ctrl Pts',(3.1346796583452,1.,-2.78260859420629));
#55446=CARTESIAN_POINT('Ctrl Pts',(3.12862530320194,-1.,-2.78094085162947));
#55447=CARTESIAN_POINT('Ctrl Pts',(3.12862530320194,1.,-2.78094085162947));
#55448=CARTESIAN_POINT('Ctrl Pts',(3.12107467038623,-1.,-2.77882610147986));
#55449=CARTESIAN_POINT('Ctrl Pts',(3.12107467038623,1.,-2.77882610147986));
#55450=CARTESIAN_POINT('Ctrl Pts',(3.11354142304692,-1.,-2.77668121003225));
#55451=CARTESIAN_POINT('Ctrl Pts',(3.11354142304692,1.,-2.77668121003225));
#55452=CARTESIAN_POINT('Ctrl Pts',(3.10602568032641,-1.,-2.7745060912343));
#55453=CARTESIAN_POINT('Ctrl Pts',(3.10602568032641,1.,-2.7745060912343));
#55454=CARTESIAN_POINT('Ctrl Pts',(3.09852761277432,-1.,-2.77230064795679));
#55455=CARTESIAN_POINT('Ctrl Pts',(3.09852761277432,1.,-2.77230064795679));
#55456=CARTESIAN_POINT('Ctrl Pts',(3.09104745381882,-1.,-2.77006478033937));
#55457=CARTESIAN_POINT('Ctrl Pts',(3.09104745381882,1.,-2.77006478033937));
#55458=CARTESIAN_POINT('Ctrl Pts',(3.08358548000904,-1.,-2.76779837828843));
#55459=CARTESIAN_POINT('Ctrl Pts',(3.08358548000904,1.,-2.76779837828843));
#55460=CARTESIAN_POINT('Ctrl Pts',(3.07614198408488,-1.,-2.76550131064522));
#55461=CARTESIAN_POINT('Ctrl Pts',(3.07614198408488,1.,-2.76550131064522));
#55462=CARTESIAN_POINT('Ctrl Pts',(3.06871724843121,-1.,-2.76317341453415));
#55463=CARTESIAN_POINT('Ctrl Pts',(3.06871724843121,1.,-2.76317341453415));
#55464=CARTESIAN_POINT('Ctrl Pts',(3.06131152247599,-1.,-2.76081448760011));
#55465=CARTESIAN_POINT('Ctrl Pts',(3.06131152247599,1.,-2.76081448760011));
#55466=CARTESIAN_POINT('Ctrl Pts',(3.05392498750112,-1.,-2.75842427253164));
#55467=CARTESIAN_POINT('Ctrl Pts',(3.05392498750112,1.,-2.75842427253164));
#55468=CARTESIAN_POINT('Ctrl Pts',(3.04655777351333,-1.,-2.7560024745616));
#55469=CARTESIAN_POINT('Ctrl Pts',(3.04655777351333,1.,-2.7560024745616));
#55470=CARTESIAN_POINT('Ctrl Pts',(3.03921001108158,-1.,-2.75354880060473));
#55471=CARTESIAN_POINT('Ctrl Pts',(3.03921001108158,1.,-2.75354880060473));
#55472=CARTESIAN_POINT('Ctrl Pts',(3.03188187589168,-1.,-2.75106299523032));
#55473=CARTESIAN_POINT('Ctrl Pts',(3.03188187589168,1.,-2.75106299523032));
#55474=CARTESIAN_POINT('Ctrl Pts',(3.02457362909199,-1.,-2.74854487184099));
#55475=CARTESIAN_POINT('Ctrl Pts',(3.02457362909199,1.,-2.74854487184099));
#55476=CARTESIAN_POINT('Ctrl Pts',(3.01728567646502,-1.,-2.74599436193528));
#55477=CARTESIAN_POINT('Ctrl Pts',(3.01728567646502,1.,-2.74599436193528));
#55478=CARTESIAN_POINT('Ctrl Pts',(3.01001855960041,-1.,-2.7434115023978));
#55479=CARTESIAN_POINT('Ctrl Pts',(3.01001855960041,1.,-2.7434115023978));
#55480=CARTESIAN_POINT('Ctrl Pts',(3.00277284351431,-1.,-2.74079632883852));
#55481=CARTESIAN_POINT('Ctrl Pts',(3.00277284351431,1.,-2.74079632883852));
#55482=CARTESIAN_POINT('Ctrl Pts',(2.99554902409741,-1.,-2.73814878711609));
#55483=CARTESIAN_POINT('Ctrl Pts',(2.99554902409741,1.,-2.73814878711609));
#55484=CARTESIAN_POINT('Ctrl Pts',(2.98834743696455,-1.,-2.73546864694548));
#55485=CARTESIAN_POINT('Ctrl Pts',(2.98834743696455,1.,-2.73546864694548));
#55486=CARTESIAN_POINT('Ctrl Pts',(2.98116814232175,-1.,-2.73275539286537));
#55487=CARTESIAN_POINT('Ctrl Pts',(2.98116814232175,1.,-2.73275539286537));
#55488=CARTESIAN_POINT('Ctrl Pts',(2.97401089032729,-1.,-2.7300081921846));
#55489=CARTESIAN_POINT('Ctrl Pts',(2.97401089032729,1.,-2.7300081921846));
#55490=CARTESIAN_POINT('Ctrl Pts',(2.96687537842492,-1.,-2.72722614084112));
#55491=CARTESIAN_POINT('Ctrl Pts',(2.96687537842492,1.,-2.72722614084112));
#55492=CARTESIAN_POINT('Ctrl Pts',(2.95976146492595,-1.,-2.72440846811745));
#55493=CARTESIAN_POINT('Ctrl Pts',(2.95976146492595,1.,-2.72440846811745));
#55494=CARTESIAN_POINT('Ctrl Pts',(2.95266939280617,-1.,-2.72155475123361));
#55495=CARTESIAN_POINT('Ctrl Pts',(2.95266939280617,1.,-2.72155475123361));
#55496=CARTESIAN_POINT('Ctrl Pts',(2.94560002559789,-1.,-2.71866514227951));
#55497=CARTESIAN_POINT('Ctrl Pts',(2.94560002559789,1.,-2.71866514227951));
#55498=CARTESIAN_POINT('Ctrl Pts',(2.93855503247248,-1.,-2.71574054592575));
#55499=CARTESIAN_POINT('Ctrl Pts',(2.93855503247248,1.,-2.71574054592575));
#55500=CARTESIAN_POINT('Ctrl Pts',(2.93153633192583,-1.,-2.71278207520807));
#55501=CARTESIAN_POINT('Ctrl Pts',(2.93153633192583,1.,-2.71278207520807));
#55502=CARTESIAN_POINT('Ctrl Pts',(2.92454558914774,-1.,-2.70979055994751));
#55503=CARTESIAN_POINT('Ctrl Pts',(2.92454558914774,1.,-2.70979055994751));
#55504=CARTESIAN_POINT('Ctrl Pts',(2.91758367994738,-1.,-2.70676602302518));
#55505=CARTESIAN_POINT('Ctrl Pts',(2.91758367994738,1.,-2.70676602302518));
#55506=CARTESIAN_POINT('Ctrl Pts',(2.91065019668331,-1.,-2.70370719782114));
#55507=CARTESIAN_POINT('Ctrl Pts',(2.91065019668331,1.,-2.70370719782114));
#55508=CARTESIAN_POINT('Ctrl Pts',(2.90374285605839,-1.,-2.70061095078692));
#55509=CARTESIAN_POINT('Ctrl Pts',(2.90374285605839,1.,-2.70061095078692));
#55510=CARTESIAN_POINT('Ctrl Pts',(2.89685866123668,-1.,-2.69747340630621));
#55511=CARTESIAN_POINT('Ctrl Pts',(2.89685866123668,1.,-2.69747340630621));
#55512=CARTESIAN_POINT('Ctrl Pts',(2.88999512410304,-1.,-2.69429113011369));
#55513=CARTESIAN_POINT('Ctrl Pts',(2.88999512410304,1.,-2.69429113011369));
#55514=CARTESIAN_POINT('Ctrl Pts',(2.88315153980464,-1.,-2.69106236420197));
#55515=CARTESIAN_POINT('Ctrl Pts',(2.88315153980464,1.,-2.69106236420197));
#55516=CARTESIAN_POINT('Ctrl Pts',(2.87633007243885,-1.,-2.68778807801691));
#55517=CARTESIAN_POINT('Ctrl Pts',(2.87633007243885,1.,-2.68778807801691));
#55518=CARTESIAN_POINT('Ctrl Pts',(2.8695373654725,-1.,-2.68447353139611));
#55519=CARTESIAN_POINT('Ctrl Pts',(2.8695373654725,1.,-2.68447353139611));
#55520=CARTESIAN_POINT('Ctrl Pts',(2.86278224277705,-1.,-2.68112602796323));
#55521=CARTESIAN_POINT('Ctrl Pts',(2.86278224277705,1.,-2.68112602796323));
#55522=CARTESIAN_POINT('Ctrl Pts',(2.85607274378031,-1.,-2.67775201955736));
#55523=CARTESIAN_POINT('Ctrl Pts',(2.85607274378031,1.,-2.67775201955736));
#55524=CARTESIAN_POINT('Ctrl Pts',(2.84941315703096,-1.,-2.67435421039682));
#55525=CARTESIAN_POINT('Ctrl Pts',(2.84941315703096,1.,-2.67435421039682));
#55526=CARTESIAN_POINT('Ctrl Pts',(2.84280157191314,-1.,-2.67092916452117));
#55527=CARTESIAN_POINT('Ctrl Pts',(2.84280157191314,1.,-2.67092916452117));
#55528=CARTESIAN_POINT('Ctrl Pts',(2.8362258685396,-1.,-2.66746339678085));
#55529=CARTESIAN_POINT('Ctrl Pts',(2.8362258685396,1.,-2.66746339678085));
#55530=CARTESIAN_POINT('Ctrl Pts',(2.82966813308969,-1.,-2.66393764726902));
#55531=CARTESIAN_POINT('Ctrl Pts',(2.82966813308969,1.,-2.66393764726902));
#55532=CARTESIAN_POINT('Ctrl Pts',(2.82311188135053,-1.,-2.66033388273437));
#55533=CARTESIAN_POINT('Ctrl Pts',(2.82311188135053,1.,-2.66033388273437));
#55534=CARTESIAN_POINT('Ctrl Pts',(2.81654896073874,-1.,-2.65664198781335));
#55535=CARTESIAN_POINT('Ctrl Pts',(2.81654896073874,1.,-2.65664198781335));
#55536=CARTESIAN_POINT('Ctrl Pts',(2.80998526078179,-1.,-2.65286529532221));
#55537=CARTESIAN_POINT('Ctrl Pts',(2.80998526078179,1.,-2.65286529532221));
#55538=CARTESIAN_POINT('Ctrl Pts',(2.80345029781191,-1.,-2.64902988983373));
#55539=CARTESIAN_POINT('Ctrl Pts',(2.80345029781191,1.,-2.64902988983373));
#55540=CARTESIAN_POINT('Ctrl Pts',(2.7969891067079,-1.,-2.6451766779937));
#55541=CARTESIAN_POINT('Ctrl Pts',(2.7969891067079,1.,-2.6451766779937));
#55542=CARTESIAN_POINT('Ctrl Pts',(2.79064495573275,-1.,-2.64134450532632));
#55543=CARTESIAN_POINT('Ctrl Pts',(2.79064495573275,1.,-2.64134450532632));
#55544=CARTESIAN_POINT('Ctrl Pts',(2.78444351041594,-1.,-2.63755471430322));
#55545=CARTESIAN_POINT('Ctrl Pts',(2.78444351041594,1.,-2.63755471430322));
#55546=CARTESIAN_POINT('Ctrl Pts',(2.77837943466423,-1.,-2.63379800904575));
#55547=CARTESIAN_POINT('Ctrl Pts',(2.77837943466423,1.,-2.63379800904575));
#55548=CARTESIAN_POINT('Ctrl Pts',(2.77239433377839,-1.,-2.63001305229548));
#55549=CARTESIAN_POINT('Ctrl Pts',(2.77239433377839,1.,-2.63001305229548));
#55550=CARTESIAN_POINT('Ctrl Pts',(2.76639078478898,-1.,-2.6260995650624));
#55551=CARTESIAN_POINT('Ctrl Pts',(2.76639078478898,1.,-2.6260995650624));
#55552=CARTESIAN_POINT('Ctrl Pts',(2.76027271596564,-1.,-2.62195665834491));
#55553=CARTESIAN_POINT('Ctrl Pts',(2.76027271596564,1.,-2.62195665834491));
#55554=CARTESIAN_POINT('Ctrl Pts',(2.75398025025967,-1.,-2.61751580407608));
#55555=CARTESIAN_POINT('Ctrl Pts',(2.75398025025967,1.,-2.61751580407608));
#55556=CARTESIAN_POINT('Ctrl Pts',(2.74752219567307,-1.,-2.61277170105864));
#55557=CARTESIAN_POINT('Ctrl Pts',(2.74752219567307,1.,-2.61277170105864));
#55558=CARTESIAN_POINT('Ctrl Pts',(2.74102110999284,-1.,-2.60782480638629));
#55559=CARTESIAN_POINT('Ctrl Pts',(2.74102110999284,1.,-2.60782480638629));
#55560=CARTESIAN_POINT('Ctrl Pts',(2.73470730109906,-1.,-2.60287635689));
#55561=CARTESIAN_POINT('Ctrl Pts',(2.73470730109906,1.,-2.60287635689));
#55562=CARTESIAN_POINT('Ctrl Pts',(2.72886483481804,-1.,-2.5981786903501));
#55563=CARTESIAN_POINT('Ctrl Pts',(2.72886483481804,1.,-2.5981786903501));
#55564=CARTESIAN_POINT('Ctrl Pts',(2.72378896977273,-1.,-2.59399625537407));
#55565=CARTESIAN_POINT('Ctrl Pts',(2.72378896977273,1.,-2.59399625537407));
#55566=CARTESIAN_POINT('Ctrl Pts',(2.7197430895797,-1.,-2.59056604771863));
#55567=CARTESIAN_POINT('Ctrl Pts',(2.7197430895797,1.,-2.59056604771863));
#55568=CARTESIAN_POINT('Ctrl Pts',(2.71690570241274,-1.,-2.58804906785077));
#55569=CARTESIAN_POINT('Ctrl Pts',(2.71690570241274,1.,-2.58804906785077));
#55570=CARTESIAN_POINT('Ctrl Pts',(2.71566956750046,-1.,-2.58682657352212));
#55571=CARTESIAN_POINT('Ctrl Pts',(2.71566956750046,1.,-2.58682657352212));
#55572=CARTESIAN_POINT('Ctrl Pts',(2.71533674140979,-1.,-2.58636629903847));
#55573=CARTESIAN_POINT('Ctrl Pts',(2.71533674140979,1.,-2.58636629903847));
#55574=CARTESIAN_POINT('Ctrl Pts',(2.71537879704999,-1.,-2.58626222935706));
#55575=CARTESIAN_POINT('Ctrl Pts',(2.71537879704999,1.,-2.58626222935706));
#55576=CARTESIAN_POINT('Ctrl Pts',(2.71546581445404,-1.,-2.58626089374824));
#55577=CARTESIAN_POINT('Ctrl Pts',(2.71546581445404,1.,-2.58626089374824));
#55578=CARTESIAN_POINT('',(3.14378277984898,1.,-2.78507268004356));
#55579=CARTESIAN_POINT('Ctrl Pts',(3.14378277984898,1.,-2.78507268004356));
#55580=CARTESIAN_POINT('Ctrl Pts',(3.14226401019149,1.,-2.78466475036183));
#55581=CARTESIAN_POINT('Ctrl Pts',(3.13922819750185,1.,-2.78384588958965));
#55582=CARTESIAN_POINT('Ctrl Pts',(3.1346796583452,1.,-2.78260859420629));
#55583=CARTESIAN_POINT('Ctrl Pts',(3.12862530320194,1.,-2.78094085162947));
#55584=CARTESIAN_POINT('Ctrl Pts',(3.12107467038623,1.,-2.77882610147986));
#55585=CARTESIAN_POINT('Ctrl Pts',(3.11354142304692,1.,-2.77668121003225));
#55586=CARTESIAN_POINT('Ctrl Pts',(3.10602568032641,1.,-2.7745060912343));
#55587=CARTESIAN_POINT('Ctrl Pts',(3.09852761277432,1.,-2.77230064795679));
#55588=CARTESIAN_POINT('Ctrl Pts',(3.09104745381882,1.,-2.77006478033937));
#55589=CARTESIAN_POINT('Ctrl Pts',(3.08358548000904,1.,-2.76779837828843));
#55590=CARTESIAN_POINT('Ctrl Pts',(3.07614198408488,1.,-2.76550131064522));
#55591=CARTESIAN_POINT('Ctrl Pts',(3.06871724843121,1.,-2.76317341453415));
#55592=CARTESIAN_POINT('Ctrl Pts',(3.06131152247599,1.,-2.76081448760011));
#55593=CARTESIAN_POINT('Ctrl Pts',(3.05392498750112,1.,-2.75842427253164));
#55594=CARTESIAN_POINT('Ctrl Pts',(3.04655777351333,1.,-2.7560024745616));
#55595=CARTESIAN_POINT('Ctrl Pts',(3.03921001108158,1.,-2.75354880060473));
#55596=CARTESIAN_POINT('Ctrl Pts',(3.03188187589168,1.,-2.75106299523032));
#55597=CARTESIAN_POINT('Ctrl Pts',(3.02457362909199,1.,-2.74854487184099));
#55598=CARTESIAN_POINT('Ctrl Pts',(3.01728567646502,1.,-2.74599436193528));
#55599=CARTESIAN_POINT('Ctrl Pts',(3.01001855960041,1.,-2.7434115023978));
#55600=CARTESIAN_POINT('Ctrl Pts',(3.00277284351431,1.,-2.74079632883852));
#55601=CARTESIAN_POINT('Ctrl Pts',(2.99554902409741,1.,-2.73814878711609));
#55602=CARTESIAN_POINT('Ctrl Pts',(2.98834743696455,1.,-2.73546864694548));
#55603=CARTESIAN_POINT('Ctrl Pts',(2.98116814232175,1.,-2.73275539286537));
#55604=CARTESIAN_POINT('Ctrl Pts',(2.97401089032729,1.,-2.7300081921846));
#55605=CARTESIAN_POINT('Ctrl Pts',(2.96687537842492,1.,-2.72722614084112));
#55606=CARTESIAN_POINT('Ctrl Pts',(2.95976146492595,1.,-2.72440846811745));
#55607=CARTESIAN_POINT('Ctrl Pts',(2.95266939280617,1.,-2.72155475123361));
#55608=CARTESIAN_POINT('Ctrl Pts',(2.94560002559789,1.,-2.71866514227951));
#55609=CARTESIAN_POINT('Ctrl Pts',(2.93855503247248,1.,-2.71574054592575));
#55610=CARTESIAN_POINT('Ctrl Pts',(2.93153633192583,1.,-2.71278207520807));
#55611=CARTESIAN_POINT('Ctrl Pts',(2.92454558914774,1.,-2.70979055994751));
#55612=CARTESIAN_POINT('Ctrl Pts',(2.91758367994738,1.,-2.70676602302518));
#55613=CARTESIAN_POINT('Ctrl Pts',(2.91065019668331,1.,-2.70370719782114));
#55614=CARTESIAN_POINT('Ctrl Pts',(2.90374285605839,1.,-2.70061095078692));
#55615=CARTESIAN_POINT('Ctrl Pts',(2.89685866123668,1.,-2.69747340630621));
#55616=CARTESIAN_POINT('Ctrl Pts',(2.88999512410304,1.,-2.69429113011369));
#55617=CARTESIAN_POINT('Ctrl Pts',(2.88315153980464,1.,-2.69106236420197));
#55618=CARTESIAN_POINT('Ctrl Pts',(2.87633007243885,1.,-2.68778807801691));
#55619=CARTESIAN_POINT('Ctrl Pts',(2.8695373654725,1.,-2.68447353139611));
#55620=CARTESIAN_POINT('Ctrl Pts',(2.86278224277705,1.,-2.68112602796323));
#55621=CARTESIAN_POINT('Ctrl Pts',(2.85607274378031,1.,-2.67775201955736));
#55622=CARTESIAN_POINT('Ctrl Pts',(2.84941315703096,1.,-2.67435421039682));
#55623=CARTESIAN_POINT('Ctrl Pts',(2.84280157191314,1.,-2.67092916452117));
#55624=CARTESIAN_POINT('Ctrl Pts',(2.8362258685396,1.,-2.66746339678085));
#55625=CARTESIAN_POINT('Ctrl Pts',(2.82966813308969,1.,-2.66393764726902));
#55626=CARTESIAN_POINT('Ctrl Pts',(2.82311188135053,1.,-2.66033388273437));
#55627=CARTESIAN_POINT('Ctrl Pts',(2.81654896073874,1.,-2.65664198781335));
#55628=CARTESIAN_POINT('Ctrl Pts',(2.80998526078179,1.,-2.65286529532221));
#55629=CARTESIAN_POINT('Ctrl Pts',(2.80345029781191,1.,-2.64902988983373));
#55630=CARTESIAN_POINT('Ctrl Pts',(2.7969891067079,1.,-2.6451766779937));
#55631=CARTESIAN_POINT('Ctrl Pts',(2.79064495573275,1.,-2.64134450532632));
#55632=CARTESIAN_POINT('Ctrl Pts',(2.78444351041594,1.,-2.63755471430322));
#55633=CARTESIAN_POINT('Ctrl Pts',(2.77837943466423,1.,-2.63379800904575));
#55634=CARTESIAN_POINT('Ctrl Pts',(2.77239433377839,1.,-2.63001305229548));
#55635=CARTESIAN_POINT('Ctrl Pts',(2.76639078478898,1.,-2.6260995650624));
#55636=CARTESIAN_POINT('Ctrl Pts',(2.76027271596564,1.,-2.62195665834491));
#55637=CARTESIAN_POINT('Ctrl Pts',(2.75398025025967,1.,-2.61751580407608));
#55638=CARTESIAN_POINT('Ctrl Pts',(2.74752219567307,1.,-2.61277170105864));
#55639=CARTESIAN_POINT('Ctrl Pts',(2.74102110999284,1.,-2.60782480638629));
#55640=CARTESIAN_POINT('Ctrl Pts',(2.73470730109906,1.,-2.60287635689));
#55641=CARTESIAN_POINT('Ctrl Pts',(2.72886483481804,1.,-2.5981786903501));
#55642=CARTESIAN_POINT('Ctrl Pts',(2.72378896977273,1.,-2.59399625537407));
#55643=CARTESIAN_POINT('Ctrl Pts',(2.7197430895797,1.,-2.59056604771863));
#55644=CARTESIAN_POINT('Ctrl Pts',(2.7171186028189,1.,-2.58823792682724));
#55645=CARTESIAN_POINT('Ctrl Pts',(2.71591054189884,1.,-2.58706285424469));
#55646=CARTESIAN_POINT('Ctrl Pts',(2.71548946460616,1.,-2.58656037976884));
#55647=CARTESIAN_POINT('Ctrl Pts',(2.71540296615967,1.,-2.58638312917291));
#55648=CARTESIAN_POINT('Ctrl Pts',(2.71539546306824,1.,-2.58633475775051));
#55649=CARTESIAN_POINT('',(3.14378277984898,0.,-2.78507268004356));
#55650=CARTESIAN_POINT('Ctrl Pts',(2.97921217251145,-1.,-2.27745358485296));
#55651=CARTESIAN_POINT('Ctrl Pts',(2.97921217251145,1.,-2.27745358485296));
#55652=CARTESIAN_POINT('Ctrl Pts',(2.97919987915678,-1.,-2.27736742984319));
#55653=CARTESIAN_POINT('Ctrl Pts',(2.97919987915678,1.,-2.27736742984319));
#55654=CARTESIAN_POINT('Ctrl Pts',(2.97929608861798,-1.,-2.2773096118942));
#55655=CARTESIAN_POINT('Ctrl Pts',(2.97929608861798,1.,-2.2773096118942));
#55656=CARTESIAN_POINT('Ctrl Pts',(2.97980276183181,-1.,-2.27756633755188));
#55657=CARTESIAN_POINT('Ctrl Pts',(2.97980276183181,1.,-2.27756633755188));
#55658=CARTESIAN_POINT('Ctrl Pts',(2.98120357932994,-1.,-2.27859601334547));
#55659=CARTESIAN_POINT('Ctrl Pts',(2.98120357932994,1.,-2.27859601334547));
#55660=CARTESIAN_POINT('Ctrl Pts',(2.98413343613983,-1.,-2.28100472516679));
#55661=CARTESIAN_POINT('Ctrl Pts',(2.98413343613983,1.,-2.28100472516679));
#55662=CARTESIAN_POINT('Ctrl Pts',(2.9881543273478,-1.,-2.28446419115919));
#55663=CARTESIAN_POINT('Ctrl Pts',(2.9881543273478,1.,-2.28446419115919));
#55664=CARTESIAN_POINT('Ctrl Pts',(2.99307930984034,-1.,-2.28882328690362));
#55665=CARTESIAN_POINT('Ctrl Pts',(2.99307930984034,1.,-2.28882328690362));
#55666=CARTESIAN_POINT('Ctrl Pts',(2.99863310339691,-1.,-2.29385894577754));
#55667=CARTESIAN_POINT('Ctrl Pts',(2.99863310339691,1.,-2.29385894577754));
#55668=CARTESIAN_POINT('Ctrl Pts',(3.00450832658613,-1.,-2.29932091315775));
#55669=CARTESIAN_POINT('Ctrl Pts',(3.00450832658613,1.,-2.29932091315775));
#55670=CARTESIAN_POINT('Ctrl Pts',(3.01041131063823,-1.,-2.30496809486482));
#55671=CARTESIAN_POINT('Ctrl Pts',(3.01041131063823,1.,-2.30496809486482));
#55672=CARTESIAN_POINT('Ctrl Pts',(3.01610726819086,-1.,-2.31060449886629));
#55673=CARTESIAN_POINT('Ctrl Pts',(3.01610726819086,1.,-2.31060449886629));
#55674=CARTESIAN_POINT('Ctrl Pts',(3.0214778066816,-1.,-2.31612479121631));
#55675=CARTESIAN_POINT('Ctrl Pts',(3.0214778066816,1.,-2.31612479121631));
#55676=CARTESIAN_POINT('Ctrl Pts',(3.02652678416611,-1.,-2.32151944306402));
#55677=CARTESIAN_POINT('Ctrl Pts',(3.02652678416611,1.,-2.32151944306402));
#55678=CARTESIAN_POINT('Ctrl Pts',(3.03133125185136,-1.,-2.32683687412097));
#55679=CARTESIAN_POINT('Ctrl Pts',(3.03133125185136,1.,-2.32683687412097));
#55680=CARTESIAN_POINT('Ctrl Pts',(3.03600588555793,-1.,-2.33215619079829));
#55681=CARTESIAN_POINT('Ctrl Pts',(3.03600588555793,1.,-2.33215619079829));
#55682=CARTESIAN_POINT('Ctrl Pts',(3.04066496998544,-1.,-2.33755792953706));
#55683=CARTESIAN_POINT('Ctrl Pts',(3.04066496998544,1.,-2.33755792953706));
#55684=CARTESIAN_POINT('Ctrl Pts',(3.04537822217256,-1.,-2.34309017083977));
#55685=CARTESIAN_POINT('Ctrl Pts',(3.04537822217256,1.,-2.34309017083977));
#55686=CARTESIAN_POINT('Ctrl Pts',(3.05015565829918,-1.,-2.34875673090771));
#55687=CARTESIAN_POINT('Ctrl Pts',(3.05015565829918,1.,-2.34875673090771));
#55688=CARTESIAN_POINT('Ctrl Pts',(3.05497218368146,-1.,-2.35453559889474));
#55689=CARTESIAN_POINT('Ctrl Pts',(3.05497218368146,1.,-2.35453559889474));
#55690=CARTESIAN_POINT('Ctrl Pts',(3.0597826624004,-1.,-2.36039011602072));
#55691=CARTESIAN_POINT('Ctrl Pts',(3.0597826624004,1.,-2.36039011602072));
#55692=CARTESIAN_POINT('Ctrl Pts',(3.06453964643162,-1.,-2.36628220107009));
#55693=CARTESIAN_POINT('Ctrl Pts',(3.06453964643162,1.,-2.36628220107009));
#55694=CARTESIAN_POINT('Ctrl Pts',(3.069212754975,-1.,-2.37218678163178));
#55695=CARTESIAN_POINT('Ctrl Pts',(3.069212754975,1.,-2.37218678163178));
#55696=CARTESIAN_POINT('Ctrl Pts',(3.07379777492165,-1.,-2.37809856205548));
#55697=CARTESIAN_POINT('Ctrl Pts',(3.07379777492165,1.,-2.37809856205548));
#55698=CARTESIAN_POINT('Ctrl Pts',(3.07830597244326,-1.,-2.38402401216126));
#55699=CARTESIAN_POINT('Ctrl Pts',(3.07830597244326,1.,-2.38402401216126));
#55700=CARTESIAN_POINT('Ctrl Pts',(3.08275773747093,-1.,-2.38997659219199));
#55701=CARTESIAN_POINT('Ctrl Pts',(3.08275773747093,1.,-2.38997659219199));
#55702=CARTESIAN_POINT('Ctrl Pts',(3.08717489512914,-1.,-2.39597098250631));
#55703=CARTESIAN_POINT('Ctrl Pts',(3.08717489512914,1.,-2.39597098250631));
#55704=CARTESIAN_POINT('Ctrl Pts',(3.091572660511,-1.,-2.40201704423341));
#55705=CARTESIAN_POINT('Ctrl Pts',(3.091572660511,1.,-2.40201704423341));
#55706=CARTESIAN_POINT('Ctrl Pts',(3.09595472616076,-1.,-2.40811612696369));
#55707=CARTESIAN_POINT('Ctrl Pts',(3.09595472616076,1.,-2.40811612696369));
#55708=CARTESIAN_POINT('Ctrl Pts',(3.1003177502767,-1.,-2.41426441798057));
#55709=CARTESIAN_POINT('Ctrl Pts',(3.1003177502767,1.,-2.41426441798057));
#55710=CARTESIAN_POINT('Ctrl Pts',(3.10465410280896,-1.,-2.42045498612489));
#55711=CARTESIAN_POINT('Ctrl Pts',(3.10465410280896,1.,-2.42045498612489));
#55712=CARTESIAN_POINT('Ctrl Pts',(3.10895518969595,-1.,-2.42668025870015));
#55713=CARTESIAN_POINT('Ctrl Pts',(3.10895518969595,1.,-2.42668025870015));
#55714=CARTESIAN_POINT('Ctrl Pts',(3.11321477659018,-1.,-2.43293449685144));
#55715=CARTESIAN_POINT('Ctrl Pts',(3.11321477659018,1.,-2.43293449685144));
#55716=CARTESIAN_POINT('Ctrl Pts',(3.11743156744186,-1.,-2.43921571477977));
#55717=CARTESIAN_POINT('Ctrl Pts',(3.11743156744186,1.,-2.43921571477977));
#55718=CARTESIAN_POINT('Ctrl Pts',(3.12160740887768,-1.,-2.44552433364715));
#55719=CARTESIAN_POINT('Ctrl Pts',(3.12160740887768,1.,-2.44552433364715));
#55720=CARTESIAN_POINT('Ctrl Pts',(3.12574608210847,-1.,-2.45186227369846));
#55721=CARTESIAN_POINT('Ctrl Pts',(3.12574608210847,1.,-2.45186227369846));
#55722=CARTESIAN_POINT('Ctrl Pts',(3.12985188384371,-1.,-2.45823188859366));
#55723=CARTESIAN_POINT('Ctrl Pts',(3.12985188384371,1.,-2.45823188859366));
#55724=CARTESIAN_POINT('Ctrl Pts',(3.13392826623906,-1.,-2.46463494332374));
#55725=CARTESIAN_POINT('Ctrl Pts',(3.13392826623906,1.,-2.46463494332374));
#55726=CARTESIAN_POINT('Ctrl Pts',(3.13797654408943,-1.,-2.47107164236838));
#55727=CARTESIAN_POINT('Ctrl Pts',(3.13797654408943,1.,-2.47107164236838));
#55728=CARTESIAN_POINT('Ctrl Pts',(3.14199655778863,-1.,-2.47754112428043));
#55729=CARTESIAN_POINT('Ctrl Pts',(3.14199655778863,1.,-2.47754112428043));
#55730=CARTESIAN_POINT('Ctrl Pts',(3.14598722723896,-1.,-2.4840418741839));
#55731=CARTESIAN_POINT('Ctrl Pts',(3.14598722723896,1.,-2.4840418741839));
#55732=CARTESIAN_POINT('Ctrl Pts',(3.14994715298907,-1.,-2.49057217131988));
#55733=CARTESIAN_POINT('Ctrl Pts',(3.14994715298907,1.,-2.49057217131988));
#55734=CARTESIAN_POINT('Ctrl Pts',(3.15387518039046,-1.,-2.49713050858896));
#55735=CARTESIAN_POINT('Ctrl Pts',(3.15387518039046,1.,-2.49713050858896));
#55736=CARTESIAN_POINT('Ctrl Pts',(3.15777102413957,-1.,-2.50371605688252));
#55737=CARTESIAN_POINT('Ctrl Pts',(3.15777102413957,1.,-2.50371605688252));
#55738=CARTESIAN_POINT('Ctrl Pts',(3.16163506380157,-1.,-2.51032851007894));
#55739=CARTESIAN_POINT('Ctrl Pts',(3.16163506380157,1.,-2.51032851007894));
#55740=CARTESIAN_POINT('Ctrl Pts',(3.16546808277023,-1.,-2.51696788755577));
#55741=CARTESIAN_POINT('Ctrl Pts',(3.16546808277023,1.,-2.51696788755577));
#55742=CARTESIAN_POINT('Ctrl Pts',(3.16927102130735,-1.,-2.52363434671788));
#55743=CARTESIAN_POINT('Ctrl Pts',(3.16927102130735,1.,-2.52363434671788));
#55744=CARTESIAN_POINT('Ctrl Pts',(3.17304474093612,-1.,-2.53032800406941));
#55745=CARTESIAN_POINT('Ctrl Pts',(3.17304474093612,1.,-2.53032800406941));
#55746=CARTESIAN_POINT('Ctrl Pts',(3.17678974135318,-1.,-2.53704871950948));
#55747=CARTESIAN_POINT('Ctrl Pts',(3.17678974135318,1.,-2.53704871950948));
#55748=CARTESIAN_POINT('Ctrl Pts',(3.18050619750639,-1.,-2.54379612553051));
#55749=CARTESIAN_POINT('Ctrl Pts',(3.18050619750639,1.,-2.54379612553051));
#55750=CARTESIAN_POINT('Ctrl Pts',(3.18419408529594,-1.,-2.55056972387731));
#55751=CARTESIAN_POINT('Ctrl Pts',(3.18419408529594,1.,-2.55056972387731));
#55752=CARTESIAN_POINT('Ctrl Pts',(3.18785328116218,-1.,-2.55736896206056));
#55753=CARTESIAN_POINT('Ctrl Pts',(3.18785328116218,1.,-2.55736896206056));
#55754=CARTESIAN_POINT('Ctrl Pts',(3.19148366395139,-1.,-2.56419331092858));
#55755=CARTESIAN_POINT('Ctrl Pts',(3.19148366395139,1.,-2.56419331092858));
#55756=CARTESIAN_POINT('Ctrl Pts',(3.19508523784363,-1.,-2.57104235897899));
#55757=CARTESIAN_POINT('Ctrl Pts',(3.19508523784363,1.,-2.57104235897899));
#55758=CARTESIAN_POINT('Ctrl Pts',(3.19865814628682,-1.,-2.57791581908875));
#55759=CARTESIAN_POINT('Ctrl Pts',(3.19865814628682,1.,-2.57791581908875));
#55760=CARTESIAN_POINT('Ctrl Pts',(3.20220261408414,-1.,-2.58481347777729));
#55761=CARTESIAN_POINT('Ctrl Pts',(3.20220261408414,1.,-2.58481347777729));
#55762=CARTESIAN_POINT('Ctrl Pts',(3.2057189102873,-1.,-2.59173516023481));
#55763=CARTESIAN_POINT('Ctrl Pts',(3.2057189102873,1.,-2.59173516023481));
#55764=CARTESIAN_POINT('Ctrl Pts',(3.20920730569681,-1.,-2.59868069194342));
#55765=CARTESIAN_POINT('Ctrl Pts',(3.20920730569681,1.,-2.59868069194342));
#55766=CARTESIAN_POINT('Ctrl Pts',(3.21266802609681,-1.,-2.60564985360017));
#55767=CARTESIAN_POINT('Ctrl Pts',(3.21266802609681,1.,-2.60564985360017));
#55768=CARTESIAN_POINT('Ctrl Pts',(3.21610123233082,-1.,-2.61264236719171));
#55769=CARTESIAN_POINT('Ctrl Pts',(3.21610123233082,1.,-2.61264236719171));
#55770=CARTESIAN_POINT('Ctrl Pts',(3.21950704109321,-1.,-2.61965792832947));
#55771=CARTESIAN_POINT('Ctrl Pts',(3.21950704109321,1.,-2.61965792832947));
#55772=CARTESIAN_POINT('Ctrl Pts',(3.2228855361324,-1.,-2.62669622735912));
#55773=CARTESIAN_POINT('Ctrl Pts',(3.2228855361324,1.,-2.62669622735912));
#55774=CARTESIAN_POINT('Ctrl Pts',(3.2262367829246,-1.,-2.63375697391372));
#55775=CARTESIAN_POINT('Ctrl Pts',(3.2262367829246,1.,-2.63375697391372));
#55776=CARTESIAN_POINT('Ctrl Pts',(3.22956084358547,-1.,-2.64083992181823));
#55777=CARTESIAN_POINT('Ctrl Pts',(3.22956084358547,1.,-2.64083992181823));
#55778=CARTESIAN_POINT('Ctrl Pts',(3.23285778737096,-1.,-2.64794488743038));
#55779=CARTESIAN_POINT('Ctrl Pts',(3.23285778737096,1.,-2.64794488743038));
#55780=CARTESIAN_POINT('Ctrl Pts',(3.236127680639,-1.,-2.65507173961555));
#55781=CARTESIAN_POINT('Ctrl Pts',(3.236127680639,1.,-2.65507173961555));
#55782=CARTESIAN_POINT('Ctrl Pts',(3.23872200034785,-1.,-2.6607906631847));
#55783=CARTESIAN_POINT('Ctrl Pts',(3.23872200034785,1.,-2.6607906631847));
#55784=CARTESIAN_POINT('Ctrl Pts',(3.24065561086749,-1.,-2.66508964663997));
#55785=CARTESIAN_POINT('Ctrl Pts',(3.24065561086749,1.,-2.66508964663997));
#55786=CARTESIAN_POINT('Ctrl Pts',(3.24193929584471,-1.,-2.66795998539579));
#55787=CARTESIAN_POINT('Ctrl Pts',(3.24193929584471,1.,-2.66795998539579));
#55788=CARTESIAN_POINT('Ctrl Pts',(3.24257979115744,-1.,-2.66939624221984));
#55789=CARTESIAN_POINT('Ctrl Pts',(3.24257979115744,1.,-2.66939624221984));
#55790=CARTESIAN_POINT('',(2.97927412174279,1.,-2.27737254473521));
#55791=CARTESIAN_POINT('Ctrl Pts',(2.97927412174279,-1.,-2.27737254473521));
#55792=CARTESIAN_POINT('Ctrl Pts',(2.97927412174279,-0.666666666666667,
-2.27737254473521));
#55793=CARTESIAN_POINT('Ctrl Pts',(2.97927412174279,-0.333333333333333,
-2.27737254473521));
#55794=CARTESIAN_POINT('Ctrl Pts',(2.97927412174279,0.333333333333333,-2.27737254473521));
#55795=CARTESIAN_POINT('Ctrl Pts',(2.97927412174279,0.666666666666667,-2.27737254473521));
#55796=CARTESIAN_POINT('Ctrl Pts',(2.97927412174279,1.,-2.27737254473521));
#55797=CARTESIAN_POINT('',(3.24257979115744,1.,-2.66939624221984));
#55798=CARTESIAN_POINT('',(3.24257979115744,0.,-2.66939624221984));
#55799=CARTESIAN_POINT('Ctrl Pts',(2.97927412174279,1.,-2.27737254473521));
#55800=CARTESIAN_POINT('Ctrl Pts',(2.97932307137476,1.,-2.27737238849287));
#55801=CARTESIAN_POINT('Ctrl Pts',(2.9795116710597,1.,-2.27743009389684));
#55802=CARTESIAN_POINT('Ctrl Pts',(2.98007383024207,1.,-2.27776738270289));
#55803=CARTESIAN_POINT('Ctrl Pts',(2.9814234180956,1.,-2.27877674853766));
#55804=CARTESIAN_POINT('Ctrl Pts',(2.98413343613983,1.,-2.28100472516679));
#55805=CARTESIAN_POINT('Ctrl Pts',(2.9881543273478,1.,-2.28446419115919));
#55806=CARTESIAN_POINT('Ctrl Pts',(2.99307930984034,1.,-2.28882328690362));
#55807=CARTESIAN_POINT('Ctrl Pts',(2.99863310339691,1.,-2.29385894577754));
#55808=CARTESIAN_POINT('Ctrl Pts',(3.00450832658613,1.,-2.29932091315775));
#55809=CARTESIAN_POINT('Ctrl Pts',(3.01041131063823,1.,-2.30496809486482));
#55810=CARTESIAN_POINT('Ctrl Pts',(3.01610726819086,1.,-2.31060449886629));
#55811=CARTESIAN_POINT('Ctrl Pts',(3.0214778066816,1.,-2.31612479121631));
#55812=CARTESIAN_POINT('Ctrl Pts',(3.02652678416611,1.,-2.32151944306402));
#55813=CARTESIAN_POINT('Ctrl Pts',(3.03133125185136,1.,-2.32683687412097));
#55814=CARTESIAN_POINT('Ctrl Pts',(3.03600588555793,1.,-2.33215619079829));
#55815=CARTESIAN_POINT('Ctrl Pts',(3.04066496998544,1.,-2.33755792953706));
#55816=CARTESIAN_POINT('Ctrl Pts',(3.04537822217256,1.,-2.34309017083977));
#55817=CARTESIAN_POINT('Ctrl Pts',(3.05015565829918,1.,-2.34875673090771));
#55818=CARTESIAN_POINT('Ctrl Pts',(3.05497218368146,1.,-2.35453559889474));
#55819=CARTESIAN_POINT('Ctrl Pts',(3.0597826624004,1.,-2.36039011602072));
#55820=CARTESIAN_POINT('Ctrl Pts',(3.06453964643162,1.,-2.36628220107009));
#55821=CARTESIAN_POINT('Ctrl Pts',(3.069212754975,1.,-2.37218678163178));
#55822=CARTESIAN_POINT('Ctrl Pts',(3.07379777492165,1.,-2.37809856205548));
#55823=CARTESIAN_POINT('Ctrl Pts',(3.07830597244326,1.,-2.38402401216126));
#55824=CARTESIAN_POINT('Ctrl Pts',(3.08275773747093,1.,-2.38997659219199));
#55825=CARTESIAN_POINT('Ctrl Pts',(3.08717489512914,1.,-2.39597098250631));
#55826=CARTESIAN_POINT('Ctrl Pts',(3.091572660511,1.,-2.40201704423341));
#55827=CARTESIAN_POINT('Ctrl Pts',(3.09595472616076,1.,-2.40811612696369));
#55828=CARTESIAN_POINT('Ctrl Pts',(3.1003177502767,1.,-2.41426441798057));
#55829=CARTESIAN_POINT('Ctrl Pts',(3.10465410280896,1.,-2.42045498612489));
#55830=CARTESIAN_POINT('Ctrl Pts',(3.10895518969595,1.,-2.42668025870015));
#55831=CARTESIAN_POINT('Ctrl Pts',(3.11321477659018,1.,-2.43293449685144));
#55832=CARTESIAN_POINT('Ctrl Pts',(3.11743156744186,1.,-2.43921571477977));
#55833=CARTESIAN_POINT('Ctrl Pts',(3.12160740887768,1.,-2.44552433364715));
#55834=CARTESIAN_POINT('Ctrl Pts',(3.12574608210847,1.,-2.45186227369846));
#55835=CARTESIAN_POINT('Ctrl Pts',(3.12985188384371,1.,-2.45823188859366));
#55836=CARTESIAN_POINT('Ctrl Pts',(3.13392826623906,1.,-2.46463494332374));
#55837=CARTESIAN_POINT('Ctrl Pts',(3.13797654408943,1.,-2.47107164236838));
#55838=CARTESIAN_POINT('Ctrl Pts',(3.14199655778863,1.,-2.47754112428043));
#55839=CARTESIAN_POINT('Ctrl Pts',(3.14598722723896,1.,-2.4840418741839));
#55840=CARTESIAN_POINT('Ctrl Pts',(3.14994715298907,1.,-2.49057217131988));
#55841=CARTESIAN_POINT('Ctrl Pts',(3.15387518039046,1.,-2.49713050858896));
#55842=CARTESIAN_POINT('Ctrl Pts',(3.15777102413957,1.,-2.50371605688252));
#55843=CARTESIAN_POINT('Ctrl Pts',(3.16163506380157,1.,-2.51032851007894));
#55844=CARTESIAN_POINT('Ctrl Pts',(3.16546808277023,1.,-2.51696788755577));
#55845=CARTESIAN_POINT('Ctrl Pts',(3.16927102130735,1.,-2.52363434671788));
#55846=CARTESIAN_POINT('Ctrl Pts',(3.17304474093612,1.,-2.53032800406941));
#55847=CARTESIAN_POINT('Ctrl Pts',(3.17678974135318,1.,-2.53704871950948));
#55848=CARTESIAN_POINT('Ctrl Pts',(3.18050619750639,1.,-2.54379612553051));
#55849=CARTESIAN_POINT('Ctrl Pts',(3.18419408529594,1.,-2.55056972387731));
#55850=CARTESIAN_POINT('Ctrl Pts',(3.18785328116218,1.,-2.55736896206056));
#55851=CARTESIAN_POINT('Ctrl Pts',(3.19148366395139,1.,-2.56419331092858));
#55852=CARTESIAN_POINT('Ctrl Pts',(3.19508523784363,1.,-2.57104235897899));
#55853=CARTESIAN_POINT('Ctrl Pts',(3.19865814628682,1.,-2.57791581908875));
#55854=CARTESIAN_POINT('Ctrl Pts',(3.20220261408414,1.,-2.58481347777729));
#55855=CARTESIAN_POINT('Ctrl Pts',(3.2057189102873,1.,-2.59173516023481));
#55856=CARTESIAN_POINT('Ctrl Pts',(3.20920730569681,1.,-2.59868069194342));
#55857=CARTESIAN_POINT('Ctrl Pts',(3.21266802609681,1.,-2.60564985360017));
#55858=CARTESIAN_POINT('Ctrl Pts',(3.21610123233082,1.,-2.61264236719171));
#55859=CARTESIAN_POINT('Ctrl Pts',(3.21950704109321,1.,-2.61965792832947));
#55860=CARTESIAN_POINT('Ctrl Pts',(3.2228855361324,1.,-2.62669622735912));
#55861=CARTESIAN_POINT('Ctrl Pts',(3.2262367829246,1.,-2.63375697391372));
#55862=CARTESIAN_POINT('Ctrl Pts',(3.22956084358547,1.,-2.64083992181823));
#55863=CARTESIAN_POINT('Ctrl Pts',(3.23285778737096,1.,-2.64794488743038));
#55864=CARTESIAN_POINT('Ctrl Pts',(3.236127680639,1.,-2.65507173961555));
#55865=CARTESIAN_POINT('Ctrl Pts',(3.23872200034785,1.,-2.6607906631847));
#55866=CARTESIAN_POINT('Ctrl Pts',(3.24065561086749,1.,-2.66508964663997));
#55867=CARTESIAN_POINT('Ctrl Pts',(3.24193929584471,1.,-2.66795998539579));
#55868=CARTESIAN_POINT('Ctrl Pts',(3.24257979115744,1.,-2.66939624221984));
#55869=CARTESIAN_POINT('Origin',(3.24257979115744,0.,-2.66939624221984));
#55870=CARTESIAN_POINT('',(3.14378277984898,1.,-2.78507268004356));
#55871=CARTESIAN_POINT('Origin',(0.,0.,0.));
#55872=CARTESIAN_POINT('',(3.08655633322109,1.,-2.12971124846838));
#55873=CARTESIAN_POINT('Origin',(0.,1.,0.));
#55874=CARTESIAN_POINT('Ctrl Pts',(3.0865563332211,1.,-2.12971124846838));
#55875=CARTESIAN_POINT('Ctrl Pts',(3.0865563332211,0.666666666666667,-2.12971124846838));
#55876=CARTESIAN_POINT('Ctrl Pts',(3.0865563332211,0.333333333333333,-2.12971124846838));
#55877=CARTESIAN_POINT('Ctrl Pts',(3.0865563332211,-0.333333333333333,-2.12971124846838));
#55878=CARTESIAN_POINT('Ctrl Pts',(3.0865563332211,-0.666666666666667,-2.12971124846838));
#55879=CARTESIAN_POINT('Ctrl Pts',(3.0865563332211,-1.,-2.12971124846838));
#55880=CARTESIAN_POINT('Ctrl Pts',(3.54075895182139,-1.,-2.25898783642071));
#55881=CARTESIAN_POINT('Ctrl Pts',(3.54075895182139,1.,-2.25898783642071));
#55882=CARTESIAN_POINT('Ctrl Pts',(3.5391950664771,-1.,-2.25882251694918));
#55883=CARTESIAN_POINT('Ctrl Pts',(3.5391950664771,1.,-2.25882251694918));
#55884=CARTESIAN_POINT('Ctrl Pts',(3.53606853163247,-1.,-2.25848864344599));
#55885=CARTESIAN_POINT('Ctrl Pts',(3.53606853163247,1.,-2.25848864344599));
#55886=CARTESIAN_POINT('Ctrl Pts',(3.53138243689932,-1.,-2.25797812951166));
#55887=CARTESIAN_POINT('Ctrl Pts',(3.53138243689932,1.,-2.25797812951166));
#55888=CARTESIAN_POINT('Ctrl Pts',(3.52514172849666,-1.,-2.25727802942142));
#55889=CARTESIAN_POINT('Ctrl Pts',(3.52514172849666,1.,-2.25727802942142));
#55890=CARTESIAN_POINT('Ctrl Pts',(3.51735323669213,-1.,-2.25637049456061));
#55891=CARTESIAN_POINT('Ctrl Pts',(3.51735323669213,1.,-2.25637049456061));
#55892=CARTESIAN_POINT('Ctrl Pts',(3.50957720118209,-1.,-2.25543046980351));
#55893=CARTESIAN_POINT('Ctrl Pts',(3.50957720118209,1.,-2.25543046980351));
#55894=CARTESIAN_POINT('Ctrl Pts',(3.50181372618058,-1.,-2.25445785151923));
#55895=CARTESIAN_POINT('Ctrl Pts',(3.50181372618058,1.,-2.25445785151923));
#55896=CARTESIAN_POINT('Ctrl Pts',(3.49406296494309,-1.,-2.25345251709453));
#55897=CARTESIAN_POINT('Ctrl Pts',(3.49406296494309,1.,-2.25345251709453));
#55898=CARTESIAN_POINT('Ctrl Pts',(3.48632513240231,-1.,-2.25241433138231));
#55899=CARTESIAN_POINT('Ctrl Pts',(3.48632513240231,1.,-2.25241433138231));
#55900=CARTESIAN_POINT('Ctrl Pts',(3.47860048448015,-1.,-2.25134314238258));
#55901=CARTESIAN_POINT('Ctrl Pts',(3.47860048448015,1.,-2.25134314238258));
#55902=CARTESIAN_POINT('Ctrl Pts',(3.47088928979467,-1.,-2.25023877475674));
#55903=CARTESIAN_POINT('Ctrl Pts',(3.47088928979467,1.,-2.25023877475674));
#55904=CARTESIAN_POINT('Ctrl Pts',(3.46319180177474,-1.,-2.24910102345977));
#55905=CARTESIAN_POINT('Ctrl Pts',(3.46319180177474,1.,-2.24910102345977));
#55906=CARTESIAN_POINT('Ctrl Pts',(3.45550823512213,-1.,-2.24792964960874));
#55907=CARTESIAN_POINT('Ctrl Pts',(3.45550823512213,1.,-2.24792964960874));
#55908=CARTESIAN_POINT('Ctrl Pts',(3.44783872863448,-1.,-2.24672437070139));
#55909=CARTESIAN_POINT('Ctrl Pts',(3.44783872863448,1.,-2.24672437070139));
#55910=CARTESIAN_POINT('Ctrl Pts',(3.44018336460619,-1.,-2.24548487526212));
#55911=CARTESIAN_POINT('Ctrl Pts',(3.44018336460619,1.,-2.24548487526212));
#55912=CARTESIAN_POINT('Ctrl Pts',(3.43254222615007,-1.,-2.24421085338856));
#55913=CARTESIAN_POINT('Ctrl Pts',(3.43254222615007,1.,-2.24421085338856));
#55914=CARTESIAN_POINT('Ctrl Pts',(3.42491544683075,-1.,-2.24290202531144));
#55915=CARTESIAN_POINT('Ctrl Pts',(3.42491544683075,1.,-2.24290202531144));
#55916=CARTESIAN_POINT('Ctrl Pts',(3.41730325539119,-1.,-2.24155816587811));
#55917=CARTESIAN_POINT('Ctrl Pts',(3.41730325539119,1.,-2.24155816587811));
#55918=CARTESIAN_POINT('Ctrl Pts',(3.40970604190205,-1.,-2.24017914395211));
#55919=CARTESIAN_POINT('Ctrl Pts',(3.40970604190205,1.,-2.24017914395211));
#55920=CARTESIAN_POINT('Ctrl Pts',(3.40212434705511,-1.,-2.23876491124064));
#55921=CARTESIAN_POINT('Ctrl Pts',(3.40212434705511,1.,-2.23876491124064));
#55922=CARTESIAN_POINT('Ctrl Pts',(3.39455873448088,-1.,-2.23731541452727));
#55923=CARTESIAN_POINT('Ctrl Pts',(3.39455873448088,1.,-2.23731541452727));
#55924=CARTESIAN_POINT('Ctrl Pts',(3.38700968549522,-1.,-2.23583052276281));
#55925=CARTESIAN_POINT('Ctrl Pts',(3.38700968549522,1.,-2.23583052276281));
#55926=CARTESIAN_POINT('Ctrl Pts',(3.37947749555649,-1.,-2.23430995599572));
#55927=CARTESIAN_POINT('Ctrl Pts',(3.37947749555649,1.,-2.23430995599572));
#55928=CARTESIAN_POINT('Ctrl Pts',(3.37196214349356,-1.,-2.23275319569253));
#55929=CARTESIAN_POINT('Ctrl Pts',(3.37196214349356,1.,-2.23275319569253));
#55930=CARTESIAN_POINT('Ctrl Pts',(3.36446325227908,-1.,-2.23115945849777));
#55931=CARTESIAN_POINT('Ctrl Pts',(3.36446325227908,1.,-2.23115945849777));
#55932=CARTESIAN_POINT('Ctrl Pts',(3.35698038165529,-1.,-2.22952789881011));
#55933=CARTESIAN_POINT('Ctrl Pts',(3.35698038165529,1.,-2.22952789881011));
#55934=CARTESIAN_POINT('Ctrl Pts',(3.34951327111117,-1.,-2.22785777756588));
#55935=CARTESIAN_POINT('Ctrl Pts',(3.34951327111117,1.,-2.22785777756588));
#55936=CARTESIAN_POINT('Ctrl Pts',(3.34206209449371,-1.,-2.22614863918044));
#55937=CARTESIAN_POINT('Ctrl Pts',(3.34206209449371,1.,-2.22614863918044));
#55938=CARTESIAN_POINT('Ctrl Pts',(3.3346277284958,-1.,-2.224400498785));
#55939=CARTESIAN_POINT('Ctrl Pts',(3.3346277284958,1.,-2.224400498785));
#55940=CARTESIAN_POINT('Ctrl Pts',(3.32721196326019,-1.,-2.22261398879623));
#55941=CARTESIAN_POINT('Ctrl Pts',(3.32721196326019,1.,-2.22261398879623));
#55942=CARTESIAN_POINT('Ctrl Pts',(3.31981686778008,-1.,-2.22078990842768));
#55943=CARTESIAN_POINT('Ctrl Pts',(3.31981686778008,1.,-2.22078990842768));
#55944=CARTESIAN_POINT('Ctrl Pts',(3.31244421655662,-1.,-2.21892881679083));
#55945=CARTESIAN_POINT('Ctrl Pts',(3.31244421655662,1.,-2.21892881679083));
#55946=CARTESIAN_POINT('Ctrl Pts',(3.3050948781957,-1.,-2.21703059947837));
#55947=CARTESIAN_POINT('Ctrl Pts',(3.3050948781957,1.,-2.21703059947837));
#55948=CARTESIAN_POINT('Ctrl Pts',(3.29776825193162,-1.,-2.2150940692337));
#55949=CARTESIAN_POINT('Ctrl Pts',(3.29776825193162,1.,-2.2150940692337));
#55950=CARTESIAN_POINT('Ctrl Pts',(3.29046159238344,-1.,-2.21311648827391));
#55951=CARTESIAN_POINT('Ctrl Pts',(3.29046159238344,1.,-2.21311648827391));
#55952=CARTESIAN_POINT('Ctrl Pts',(3.28317133333127,-1.,-2.21109449750638));
#55953=CARTESIAN_POINT('Ctrl Pts',(3.28317133333127,1.,-2.21109449750638));
#55954=CARTESIAN_POINT('Ctrl Pts',(3.27589448005534,-1.,-2.20902509417425));
#55955=CARTESIAN_POINT('Ctrl Pts',(3.27589448005534,1.,-2.20902509417425));
#55956=CARTESIAN_POINT('Ctrl Pts',(3.2686300613678,-1.,-2.20690665217741));
#55957=CARTESIAN_POINT('Ctrl Pts',(3.2686300613678,1.,-2.20690665217741));
#55958=CARTESIAN_POINT('Ctrl Pts',(3.26138036637711,-1.,-2.20473979048682));
#55959=CARTESIAN_POINT('Ctrl Pts',(3.26138036637711,1.,-2.20473979048682));
#55960=CARTESIAN_POINT('Ctrl Pts',(3.25415277957789,-1.,-2.20252866491554));
#55961=CARTESIAN_POINT('Ctrl Pts',(3.25415277957789,1.,-2.20252866491554));
#55962=CARTESIAN_POINT('Ctrl Pts',(3.24695715874356,-1.,-2.20027910880993));
#55963=CARTESIAN_POINT('Ctrl Pts',(3.24695715874356,1.,-2.20027910880993));
#55964=CARTESIAN_POINT('Ctrl Pts',(3.23980245361323,-1.,-2.19799623693263));
#55965=CARTESIAN_POINT('Ctrl Pts',(3.23980245361323,1.,-2.19799623693263));
#55966=CARTESIAN_POINT('Ctrl Pts',(3.23269332296938,-1.,-2.19568204933172));
#55967=CARTESIAN_POINT('Ctrl Pts',(3.23269332296938,1.,-2.19568204933172));
#55968=CARTESIAN_POINT('Ctrl Pts',(3.22562734221636,-1.,-2.19333345123531));
#55969=CARTESIAN_POINT('Ctrl Pts',(3.22562734221636,1.,-2.19333345123531));
#55970=CARTESIAN_POINT('Ctrl Pts',(3.21859043114069,-1.,-2.1909390194865));
#55971=CARTESIAN_POINT('Ctrl Pts',(3.21859043114069,1.,-2.1909390194865));
#55972=CARTESIAN_POINT('Ctrl Pts',(3.21156188355736,-1.,-2.18848253363878));
#55973=CARTESIAN_POINT('Ctrl Pts',(3.21156188355736,1.,-2.18848253363878));
#55974=CARTESIAN_POINT('Ctrl Pts',(3.20452259717947,-1.,-2.18594876115914));
#55975=CARTESIAN_POINT('Ctrl Pts',(3.20452259717947,1.,-2.18594876115914));
#55976=CARTESIAN_POINT('Ctrl Pts',(3.197462937404,-1.,-2.18332898656595));
#55977=CARTESIAN_POINT('Ctrl Pts',(3.197462937404,1.,-2.18332898656595));
#55978=CARTESIAN_POINT('Ctrl Pts',(3.19038924261589,-1.,-2.18062558031789));
#55979=CARTESIAN_POINT('Ctrl Pts',(3.19038924261589,1.,-2.18062558031789));
#55980=CARTESIAN_POINT('Ctrl Pts',(3.18333474627851,-1.,-2.17785968847172));
#55981=CARTESIAN_POINT('Ctrl Pts',(3.18333474627851,1.,-2.17785968847172));
#55982=CARTESIAN_POINT('Ctrl Pts',(3.17635032802584,-1.,-2.17506466903736));
#55983=CARTESIAN_POINT('Ctrl Pts',(3.17635032802584,1.,-2.17506466903736));
#55984=CARTESIAN_POINT('Ctrl Pts',(3.16948480019555,-1.,-2.17227212063857));
#55985=CARTESIAN_POINT('Ctrl Pts',(3.16948480019555,1.,-2.17227212063857));
#55986=CARTESIAN_POINT('Ctrl Pts',(3.16276685102999,-1.,-2.16949910801237));
#55987=CARTESIAN_POINT('Ctrl Pts',(3.16276685102999,1.,-2.16949910801237));
#55988=CARTESIAN_POINT('Ctrl Pts',(3.15618975593627,-1.,-2.1667372844767));
#55989=CARTESIAN_POINT('Ctrl Pts',(3.15618975593627,1.,-2.1667372844767));
#55990=CARTESIAN_POINT('Ctrl Pts',(3.14968624388961,-1.,-2.16393520288009));
#55991=CARTESIAN_POINT('Ctrl Pts',(3.14968624388961,1.,-2.16393520288009));
#55992=CARTESIAN_POINT('Ctrl Pts',(3.14314440426882,-1.,-2.16100905914341));
#55993=CARTESIAN_POINT('Ctrl Pts',(3.14314440426882,1.,-2.16100905914341));
#55994=CARTESIAN_POINT('Ctrl Pts',(3.136453565629,-1.,-2.15787423530583));
#55995=CARTESIAN_POINT('Ctrl Pts',(3.136453565629,1.,-2.15787423530583));
#55996=CARTESIAN_POINT('Ctrl Pts',(3.12954386795575,-1.,-2.15447241382872));
#55997=CARTESIAN_POINT('Ctrl Pts',(3.12954386795575,1.,-2.15447241382872));
#55998=CARTESIAN_POINT('Ctrl Pts',(3.12242318152001,-1.,-2.15079698090627));
#55999=CARTESIAN_POINT('Ctrl Pts',(3.12242318152001,1.,-2.15079698090627));
#56000=CARTESIAN_POINT('Ctrl Pts',(3.11522827017075,-1.,-2.1469279845768));
#56001=CARTESIAN_POINT('Ctrl Pts',(3.11522827017075,1.,-2.1469279845768));
#56002=CARTESIAN_POINT('Ctrl Pts',(3.10821808669189,-1.,-2.14302815602195));
#56003=CARTESIAN_POINT('Ctrl Pts',(3.10821808669189,1.,-2.14302815602195));
#56004=CARTESIAN_POINT('Ctrl Pts',(3.1017126739137,-1.,-2.13930228863968));
#56005=CARTESIAN_POINT('Ctrl Pts',(3.1017126739137,1.,-2.13930228863968));
#56006=CARTESIAN_POINT('Ctrl Pts',(3.09604502421197,-1.,-2.13596538661154));
#56007=CARTESIAN_POINT('Ctrl Pts',(3.09604502421197,1.,-2.13596538661154));
#56008=CARTESIAN_POINT('Ctrl Pts',(3.09151235281832,-1.,-2.13321032560805));
#56009=CARTESIAN_POINT('Ctrl Pts',(3.09151235281832,1.,-2.13321032560805));
#56010=CARTESIAN_POINT('Ctrl Pts',(3.08831615619661,-1.,-2.13116819908264));
#56011=CARTESIAN_POINT('Ctrl Pts',(3.08831615619661,1.,-2.13116819908264));
#56012=CARTESIAN_POINT('Ctrl Pts',(3.08690399991003,-1.,-2.1301541297915));
#56013=CARTESIAN_POINT('Ctrl Pts',(3.08690399991003,1.,-2.1301541297915));
#56014=CARTESIAN_POINT('Ctrl Pts',(3.08650326866821,-1.,-2.12975158752197));
#56015=CARTESIAN_POINT('Ctrl Pts',(3.08650326866821,1.,-2.12975158752197));
#56016=CARTESIAN_POINT('Ctrl Pts',(3.08652852644876,-1.,-2.12964222015945));
#56017=CARTESIAN_POINT('Ctrl Pts',(3.08652852644876,1.,-2.12964222015945));
#56018=CARTESIAN_POINT('Ctrl Pts',(3.08661426358891,-1.,-2.12962728847314));
#56019=CARTESIAN_POINT('Ctrl Pts',(3.08661426358891,1.,-2.12962728847314));
#56020=CARTESIAN_POINT('',(3.54075895182139,1.,-2.25898783642071));
#56021=CARTESIAN_POINT('Ctrl Pts',(3.54075895182139,1.,-2.25898783642071));
#56022=CARTESIAN_POINT('Ctrl Pts',(3.5391950664771,1.,-2.25882251694918));
#56023=CARTESIAN_POINT('Ctrl Pts',(3.53606853163247,1.,-2.25848864344599));
#56024=CARTESIAN_POINT('Ctrl Pts',(3.53138243689932,1.,-2.25797812951166));
#56025=CARTESIAN_POINT('Ctrl Pts',(3.52514172849666,1.,-2.25727802942142));
#56026=CARTESIAN_POINT('Ctrl Pts',(3.51735323669213,1.,-2.25637049456061));
#56027=CARTESIAN_POINT('Ctrl Pts',(3.50957720118209,1.,-2.25543046980351));
#56028=CARTESIAN_POINT('Ctrl Pts',(3.50181372618058,1.,-2.25445785151923));
#56029=CARTESIAN_POINT('Ctrl Pts',(3.49406296494309,1.,-2.25345251709453));
#56030=CARTESIAN_POINT('Ctrl Pts',(3.48632513240231,1.,-2.25241433138231));
#56031=CARTESIAN_POINT('Ctrl Pts',(3.47860048448015,1.,-2.25134314238258));
#56032=CARTESIAN_POINT('Ctrl Pts',(3.47088928979467,1.,-2.25023877475674));
#56033=CARTESIAN_POINT('Ctrl Pts',(3.46319180177474,1.,-2.24910102345977));
#56034=CARTESIAN_POINT('Ctrl Pts',(3.45550823512213,1.,-2.24792964960874));
#56035=CARTESIAN_POINT('Ctrl Pts',(3.44783872863448,1.,-2.24672437070139));
#56036=CARTESIAN_POINT('Ctrl Pts',(3.44018336460619,1.,-2.24548487526212));
#56037=CARTESIAN_POINT('Ctrl Pts',(3.43254222615007,1.,-2.24421085338856));
#56038=CARTESIAN_POINT('Ctrl Pts',(3.42491544683075,1.,-2.24290202531144));
#56039=CARTESIAN_POINT('Ctrl Pts',(3.41730325539119,1.,-2.24155816587811));
#56040=CARTESIAN_POINT('Ctrl Pts',(3.40970604190205,1.,-2.24017914395211));
#56041=CARTESIAN_POINT('Ctrl Pts',(3.40212434705511,1.,-2.23876491124064));
#56042=CARTESIAN_POINT('Ctrl Pts',(3.39455873448088,1.,-2.23731541452727));
#56043=CARTESIAN_POINT('Ctrl Pts',(3.38700968549522,1.,-2.23583052276281));
#56044=CARTESIAN_POINT('Ctrl Pts',(3.37947749555649,1.,-2.23430995599572));
#56045=CARTESIAN_POINT('Ctrl Pts',(3.37196214349356,1.,-2.23275319569253));
#56046=CARTESIAN_POINT('Ctrl Pts',(3.36446325227908,1.,-2.23115945849777));
#56047=CARTESIAN_POINT('Ctrl Pts',(3.35698038165529,1.,-2.22952789881011));
#56048=CARTESIAN_POINT('Ctrl Pts',(3.34951327111117,1.,-2.22785777756588));
#56049=CARTESIAN_POINT('Ctrl Pts',(3.34206209449371,1.,-2.22614863918044));
#56050=CARTESIAN_POINT('Ctrl Pts',(3.3346277284958,1.,-2.224400498785));
#56051=CARTESIAN_POINT('Ctrl Pts',(3.32721196326019,1.,-2.22261398879623));
#56052=CARTESIAN_POINT('Ctrl Pts',(3.31981686778008,1.,-2.22078990842768));
#56053=CARTESIAN_POINT('Ctrl Pts',(3.31244421655662,1.,-2.21892881679083));
#56054=CARTESIAN_POINT('Ctrl Pts',(3.3050948781957,1.,-2.21703059947837));
#56055=CARTESIAN_POINT('Ctrl Pts',(3.29776825193162,1.,-2.2150940692337));
#56056=CARTESIAN_POINT('Ctrl Pts',(3.29046159238344,1.,-2.21311648827391));
#56057=CARTESIAN_POINT('Ctrl Pts',(3.28317133333127,1.,-2.21109449750638));
#56058=CARTESIAN_POINT('Ctrl Pts',(3.27589448005534,1.,-2.20902509417425));
#56059=CARTESIAN_POINT('Ctrl Pts',(3.2686300613678,1.,-2.20690665217741));
#56060=CARTESIAN_POINT('Ctrl Pts',(3.26138036637711,1.,-2.20473979048682));
#56061=CARTESIAN_POINT('Ctrl Pts',(3.25415277957789,1.,-2.20252866491554));
#56062=CARTESIAN_POINT('Ctrl Pts',(3.24695715874356,1.,-2.20027910880993));
#56063=CARTESIAN_POINT('Ctrl Pts',(3.23980245361323,1.,-2.19799623693263));
#56064=CARTESIAN_POINT('Ctrl Pts',(3.23269332296938,1.,-2.19568204933172));
#56065=CARTESIAN_POINT('Ctrl Pts',(3.22562734221636,1.,-2.19333345123531));
#56066=CARTESIAN_POINT('Ctrl Pts',(3.21859043114069,1.,-2.1909390194865));
#56067=CARTESIAN_POINT('Ctrl Pts',(3.21156188355736,1.,-2.18848253363878));
#56068=CARTESIAN_POINT('Ctrl Pts',(3.20452259717947,1.,-2.18594876115914));
#56069=CARTESIAN_POINT('Ctrl Pts',(3.197462937404,1.,-2.18332898656595));
#56070=CARTESIAN_POINT('Ctrl Pts',(3.19038924261589,1.,-2.18062558031789));
#56071=CARTESIAN_POINT('Ctrl Pts',(3.18333474627851,1.,-2.17785968847172));
#56072=CARTESIAN_POINT('Ctrl Pts',(3.17635032802584,1.,-2.17506466903736));
#56073=CARTESIAN_POINT('Ctrl Pts',(3.16948480019555,1.,-2.17227212063857));
#56074=CARTESIAN_POINT('Ctrl Pts',(3.16276685102999,1.,-2.16949910801237));
#56075=CARTESIAN_POINT('Ctrl Pts',(3.15618975593627,1.,-2.1667372844767));
#56076=CARTESIAN_POINT('Ctrl Pts',(3.14968624388961,1.,-2.16393520288009));
#56077=CARTESIAN_POINT('Ctrl Pts',(3.14314440426882,1.,-2.16100905914341));
#56078=CARTESIAN_POINT('Ctrl Pts',(3.136453565629,1.,-2.15787423530583));
#56079=CARTESIAN_POINT('Ctrl Pts',(3.12954386795575,1.,-2.15447241382872));
#56080=CARTESIAN_POINT('Ctrl Pts',(3.12242318152001,1.,-2.15079698090627));
#56081=CARTESIAN_POINT('Ctrl Pts',(3.11522827017075,1.,-2.1469279845768));
#56082=CARTESIAN_POINT('Ctrl Pts',(3.10821808669189,1.,-2.14302815602195));
#56083=CARTESIAN_POINT('Ctrl Pts',(3.1017126739137,1.,-2.13930228863968));
#56084=CARTESIAN_POINT('Ctrl Pts',(3.09604502421197,1.,-2.13596538661154));
#56085=CARTESIAN_POINT('Ctrl Pts',(3.09151235281832,1.,-2.13321032560805));
#56086=CARTESIAN_POINT('Ctrl Pts',(3.08855597949844,1.,-2.13132142793056));
#56087=CARTESIAN_POINT('Ctrl Pts',(3.08717896996213,1.,-2.13034980480519));
#56088=CARTESIAN_POINT('Ctrl Pts',(3.08668447250383,1.,-2.12991938762497));
#56089=CARTESIAN_POINT('Ctrl Pts',(3.0865713108946,1.,-2.1297578506162));
#56090=CARTESIAN_POINT('Ctrl Pts',(3.08655633322109,1.,-2.12971124846838));
#56091=CARTESIAN_POINT('',(3.54075895182139,0.,-2.25898783642071));
#56092=CARTESIAN_POINT('Ctrl Pts',(3.2988053601491,-1.,-1.7833628895577));
#56093=CARTESIAN_POINT('Ctrl Pts',(3.2988053601491,1.,-1.7833628895577));
#56094=CARTESIAN_POINT('Ctrl Pts',(3.29877974053316,-1.,-1.78327971836342));
#56095=CARTESIAN_POINT('Ctrl Pts',(3.29877974053316,1.,-1.78327971836342));
#56096=CARTESIAN_POINT('Ctrl Pts',(3.29886572077632,-1.,-1.78320756177373));
#56097=CARTESIAN_POINT('Ctrl Pts',(3.29886572077632,1.,-1.78320756177373));
#56098=CARTESIAN_POINT('Ctrl Pts',(3.29940631674303,-1.,-1.7833818655594));
#56099=CARTESIAN_POINT('Ctrl Pts',(3.29940631674303,1.,-1.7833818655594));
#56100=CARTESIAN_POINT('Ctrl Pts',(3.30095096463517,-1.,-1.78417972819938));
#56101=CARTESIAN_POINT('Ctrl Pts',(3.30095096463517,1.,-1.78417972819938));
#56102=CARTESIAN_POINT('Ctrl Pts',(3.30422155559112,-1.,-1.78610045419846));
#56103=CARTESIAN_POINT('Ctrl Pts',(3.30422155559112,1.,-1.78610045419846));
#56104=CARTESIAN_POINT('Ctrl Pts',(3.30873412266788,-1.,-1.78888832245873));
#56105=CARTESIAN_POINT('Ctrl Pts',(3.30873412266788,1.,-1.78888832245873));
#56106=CARTESIAN_POINT('Ctrl Pts',(3.31428038326424,-1.,-1.79242331349949));
#56107=CARTESIAN_POINT('Ctrl Pts',(3.31428038326424,1.,-1.79242331349949));
#56108=CARTESIAN_POINT('Ctrl Pts',(3.3205535510082,-1.,-1.79652817033251));
#56109=CARTESIAN_POINT('Ctrl Pts',(3.3205535510082,1.,-1.79652817033251));
#56110=CARTESIAN_POINT('Ctrl Pts',(3.32721088039578,-1.,-1.80100380443406));
#56111=CARTESIAN_POINT('Ctrl Pts',(3.32721088039578,1.,-1.80100380443406));
#56112=CARTESIAN_POINT('Ctrl Pts',(3.33392460276808,-1.,-1.80565802981102));
#56113=CARTESIAN_POINT('Ctrl Pts',(3.33392460276808,1.,-1.80565802981102));
#56114=CARTESIAN_POINT('Ctrl Pts',(3.34043216147606,-1.,-1.81033399625352));
#56115=CARTESIAN_POINT('Ctrl Pts',(3.34043216147606,1.,-1.81033399625352));
#56116=CARTESIAN_POINT('Ctrl Pts',(3.34660014370673,-1.,-1.81494618732853));
#56117=CARTESIAN_POINT('Ctrl Pts',(3.34660014370673,1.,-1.81494618732853));
#56118=CARTESIAN_POINT('Ctrl Pts',(3.35243086937598,-1.,-1.81948458796829));
#56119=CARTESIAN_POINT('Ctrl Pts',(3.35243086937598,1.,-1.81948458796829));
#56120=CARTESIAN_POINT('Ctrl Pts',(3.35800801557424,-1.,-1.82398496829301));
#56121=CARTESIAN_POINT('Ctrl Pts',(3.35800801557424,1.,-1.82398496829301));
#56122=CARTESIAN_POINT('Ctrl Pts',(3.36345722124158,-1.,-1.82850752153199));
#56123=CARTESIAN_POINT('Ctrl Pts',(3.36345722124158,1.,-1.82850752153199));
#56124=CARTESIAN_POINT('Ctrl Pts',(3.36890396271836,-1.,-1.83311391452322));
#56125=CARTESIAN_POINT('Ctrl Pts',(3.36890396271836,1.,-1.83311391452322));
#56126=CARTESIAN_POINT('Ctrl Pts',(3.37442462015853,-1.,-1.83784072967077));
#56127=CARTESIAN_POINT('Ctrl Pts',(3.37442462015853,1.,-1.83784072967077));
#56128=CARTESIAN_POINT('Ctrl Pts',(3.38002968341157,-1.,-1.84269016931643));
#56129=CARTESIAN_POINT('Ctrl Pts',(3.38002968341157,1.,-1.84269016931643));
#56130=CARTESIAN_POINT('Ctrl Pts',(3.38569092349592,-1.,-1.84764441927753));
#56131=CARTESIAN_POINT('Ctrl Pts',(3.38569092349592,1.,-1.84764441927753));
#56132=CARTESIAN_POINT('Ctrl Pts',(3.39135802549398,-1.,-1.85267433291769));
#56133=CARTESIAN_POINT('Ctrl Pts',(3.39135802549398,1.,-1.85267433291769));
#56134=CARTESIAN_POINT('Ctrl Pts',(3.39697816833067,-1.,-1.85774972037062));
#56135=CARTESIAN_POINT('Ctrl Pts',(3.39697816833067,1.,-1.85774972037062));
#56136=CARTESIAN_POINT('Ctrl Pts',(3.40251742305476,-1.,-1.86285057051245));
#56137=CARTESIAN_POINT('Ctrl Pts',(3.40251742305476,1.,-1.86285057051245));
#56138=CARTESIAN_POINT('Ctrl Pts',(3.40797080000549,-1.,-1.86797231196654));
#56139=CARTESIAN_POINT('Ctrl Pts',(3.40797080000549,1.,-1.86797231196654));
#56140=CARTESIAN_POINT('Ctrl Pts',(3.41335043875209,-1.,-1.87311957248121));
#56141=CARTESIAN_POINT('Ctrl Pts',(3.41335043875209,1.,-1.87311957248121));
#56142=CARTESIAN_POINT('Ctrl Pts',(3.41867858383771,-1.,-1.87830245689344));
#56143=CARTESIAN_POINT('Ctrl Pts',(3.41867858383771,1.,-1.87830245689344));
#56144=CARTESIAN_POINT('Ctrl Pts',(3.42397908819736,-1.,-1.8835320506206));
#56145=CARTESIAN_POINT('Ctrl Pts',(3.42397908819736,1.,-1.8835320506206));
#56146=CARTESIAN_POINT('Ctrl Pts',(3.42926852222158,-1.,-1.88881571322009));
#56147=CARTESIAN_POINT('Ctrl Pts',(3.42926852222158,1.,-1.88881571322009));
#56148=CARTESIAN_POINT('Ctrl Pts',(3.43455074411571,-1.,-1.89415420002542));
#56149=CARTESIAN_POINT('Ctrl Pts',(3.43455074411571,1.,-1.89415420002542));
#56150=CARTESIAN_POINT('Ctrl Pts',(3.4398218567809,-1.,-1.89954426803384));
#56151=CARTESIAN_POINT('Ctrl Pts',(3.4398218567809,1.,-1.89954426803384));
#56152=CARTESIAN_POINT('Ctrl Pts',(3.44507323983367,-1.,-1.90498026502305));
#56153=CARTESIAN_POINT('Ctrl Pts',(3.44507323983367,1.,-1.90498026502305));
#56154=CARTESIAN_POINT('Ctrl Pts',(3.45029522038888,-1.,-1.91045605593639));
#56155=CARTESIAN_POINT('Ctrl Pts',(3.45029522038888,1.,-1.91045605593639));
#56156=CARTESIAN_POINT('Ctrl Pts',(3.4554807430995,-1.,-1.91596694784064));
#56157=CARTESIAN_POINT('Ctrl Pts',(3.4554807430995,1.,-1.91596694784064));
#56158=CARTESIAN_POINT('Ctrl Pts',(3.46062821722485,-1.,-1.92151118213212));
#56159=CARTESIAN_POINT('Ctrl Pts',(3.46062821722485,1.,-1.92151118213212));
#56160=CARTESIAN_POINT('Ctrl Pts',(3.46573953254084,-1.,-1.92708888591158));
#56161=CARTESIAN_POINT('Ctrl Pts',(3.46573953254084,1.,-1.92708888591158));
#56162=CARTESIAN_POINT('Ctrl Pts',(3.47081872409781,-1.,-1.93270136427081));
#56163=CARTESIAN_POINT('Ctrl Pts',(3.47081872409781,1.,-1.93270136427081));
#56164=CARTESIAN_POINT('Ctrl Pts',(3.47587040389915,-1.,-1.93835026973887));
#56165=CARTESIAN_POINT('Ctrl Pts',(3.47587040389915,1.,-1.93835026973887));
#56166=CARTESIAN_POINT('Ctrl Pts',(3.48089825770416,-1.,-1.94403680554065));
#56167=CARTESIAN_POINT('Ctrl Pts',(3.48089825770416,1.,-1.94403680554065));
#56168=CARTESIAN_POINT('Ctrl Pts',(3.48590361610814,-1.,-1.94976096795911));
#56169=CARTESIAN_POINT('Ctrl Pts',(3.48590361610814,1.,-1.94976096795911));
#56170=CARTESIAN_POINT('Ctrl Pts',(3.49088618670987,-1.,-1.95552193112084));
#56171=CARTESIAN_POINT('Ctrl Pts',(3.49088618670987,1.,-1.95552193112084));
#56172=CARTESIAN_POINT('Ctrl Pts',(3.49584466573064,-1.,-1.961318367765));
#56173=CARTESIAN_POINT('Ctrl Pts',(3.49584466573064,1.,-1.961318367765));
#56174=CARTESIAN_POINT('Ctrl Pts',(3.50077740176267,-1.,-1.96714879724052));
#56175=CARTESIAN_POINT('Ctrl Pts',(3.50077740176267,1.,-1.96714879724052));
#56176=CARTESIAN_POINT('Ctrl Pts',(3.5056830186108,-1.,-1.97301191162968));
#56177=CARTESIAN_POINT('Ctrl Pts',(3.5056830186108,1.,-1.97301191162968));
#56178=CARTESIAN_POINT('Ctrl Pts',(3.51056110478287,-1.,-1.97890693666288));
#56179=CARTESIAN_POINT('Ctrl Pts',(3.51056110478287,1.,-1.97890693666288));
#56180=CARTESIAN_POINT('Ctrl Pts',(3.51541198728301,-1.,-1.9848335106103));
#56181=CARTESIAN_POINT('Ctrl Pts',(3.51541198728301,1.,-1.9848335106103));
#56182=CARTESIAN_POINT('Ctrl Pts',(3.52023644289142,-1.,-1.99079153006112));
#56183=CARTESIAN_POINT('Ctrl Pts',(3.52023644289142,1.,-1.99079153006112));
#56184=CARTESIAN_POINT('Ctrl Pts',(3.52503542491728,-1.,-1.99678100339296));
#56185=CARTESIAN_POINT('Ctrl Pts',(3.52503542491728,1.,-1.99678100339296));
#56186=CARTESIAN_POINT('Ctrl Pts',(3.52980980250224,-1.,-2.00280191090366));
#56187=CARTESIAN_POINT('Ctrl Pts',(3.52980980250224,1.,-2.00280191090366));
#56188=CARTESIAN_POINT('Ctrl Pts',(3.53456004727424,-1.,-2.00885403604746));
#56189=CARTESIAN_POINT('Ctrl Pts',(3.53456004727424,1.,-2.00885403604746));
#56190=CARTESIAN_POINT('Ctrl Pts',(3.53928627453642,-1.,-2.01493698847351));
#56191=CARTESIAN_POINT('Ctrl Pts',(3.53928627453642,1.,-2.01493698847351));
#56192=CARTESIAN_POINT('Ctrl Pts',(3.54398838254136,-1.,-2.02105027983104));
#56193=CARTESIAN_POINT('Ctrl Pts',(3.54398838254136,1.,-2.02105027983104));
#56194=CARTESIAN_POINT('Ctrl Pts',(3.54866616282227,-1.,-2.02719338376175));
#56195=CARTESIAN_POINT('Ctrl Pts',(3.54866616282227,1.,-2.02719338376175));
#56196=CARTESIAN_POINT('Ctrl Pts',(3.55331941293949,-1.,-2.03336579658133));
#56197=CARTESIAN_POINT('Ctrl Pts',(3.55331941293949,1.,-2.03336579658133));
#56198=CARTESIAN_POINT('Ctrl Pts',(3.55794807264844,-1.,-2.03956711119976));
#56199=CARTESIAN_POINT('Ctrl Pts',(3.55794807264844,1.,-2.03956711119976));
#56200=CARTESIAN_POINT('Ctrl Pts',(3.56255223871505,-1.,-2.04579702158876));
#56201=CARTESIAN_POINT('Ctrl Pts',(3.56255223871505,1.,-2.04579702158876));
#56202=CARTESIAN_POINT('Ctrl Pts',(3.56713209977904,-1.,-2.05205528172911));
#56203=CARTESIAN_POINT('Ctrl Pts',(3.56713209977904,1.,-2.05205528172911));
#56204=CARTESIAN_POINT('Ctrl Pts',(3.5716878942334,-1.,-2.05834167687425));
#56205=CARTESIAN_POINT('Ctrl Pts',(3.5716878942334,1.,-2.05834167687425));
#56206=CARTESIAN_POINT('Ctrl Pts',(3.57621986224402,-1.,-2.06465599229234));
#56207=CARTESIAN_POINT('Ctrl Pts',(3.57621986224402,1.,-2.06465599229234));
#56208=CARTESIAN_POINT('Ctrl Pts',(3.58072819250872,-1.,-2.07099797606));
#56209=CARTESIAN_POINT('Ctrl Pts',(3.58072819250872,1.,-2.07099797606));
#56210=CARTESIAN_POINT('Ctrl Pts',(3.58521300039988,-1.,-2.07736732842524));
#56211=CARTESIAN_POINT('Ctrl Pts',(3.58521300039988,1.,-2.07736732842524));
#56212=CARTESIAN_POINT('Ctrl Pts',(3.58967435355834,-1.,-2.08376373049196));
#56213=CARTESIAN_POINT('Ctrl Pts',(3.58967435355834,1.,-2.08376373049196));
#56214=CARTESIAN_POINT('Ctrl Pts',(3.5941122862608,-1.,-2.09018686331706));
#56215=CARTESIAN_POINT('Ctrl Pts',(3.5941122862608,1.,-2.09018686331706));
#56216=CARTESIAN_POINT('Ctrl Pts',(3.59852681775396,-1.,-2.09663642986579));
#56217=CARTESIAN_POINT('Ctrl Pts',(3.59852681775396,1.,-2.09663642986579));
#56218=CARTESIAN_POINT('Ctrl Pts',(3.60291797087849,-1.,-2.10311217727687));
#56219=CARTESIAN_POINT('Ctrl Pts',(3.60291797087849,1.,-2.10311217727687));
#56220=CARTESIAN_POINT('Ctrl Pts',(3.60728578530968,-1.,-2.10961391333497));
#56221=CARTESIAN_POINT('Ctrl Pts',(3.60728578530968,1.,-2.10961391333497));
#56222=CARTESIAN_POINT('Ctrl Pts',(3.61163030607452,-1.,-2.11614149813928));
#56223=CARTESIAN_POINT('Ctrl Pts',(3.61163030607452,1.,-2.11614149813928));
#56224=CARTESIAN_POINT('Ctrl Pts',(3.61508732215187,-1.,-2.12138417125349));
#56225=CARTESIAN_POINT('Ctrl Pts',(3.61508732215187,1.,-2.12138417125349));
#56226=CARTESIAN_POINT('Ctrl Pts',(3.61766963589442,-1.,-2.12532774376144));
#56227=CARTESIAN_POINT('Ctrl Pts',(3.61766963589442,1.,-2.12532774376144));
#56228=CARTESIAN_POINT('Ctrl Pts',(3.61938653648716,-1.,-2.12796193131142));
#56229=CARTESIAN_POINT('Ctrl Pts',(3.61938653648716,1.,-2.12796193131142));
#56230=CARTESIAN_POINT('Ctrl Pts',(3.62024382630768,-1.,-2.12928030988903));
#56231=CARTESIAN_POINT('Ctrl Pts',(3.62024382630768,1.,-2.12928030988903));
#56232=CARTESIAN_POINT('',(3.29885386921514,1.,-1.78327315618341));
#56233=CARTESIAN_POINT('Ctrl Pts',(3.29885386921513,-1.,-1.78327315618341));
#56234=CARTESIAN_POINT('Ctrl Pts',(3.29885386921513,-0.666666666666667,
-1.78327315618341));
#56235=CARTESIAN_POINT('Ctrl Pts',(3.29885386921513,-0.333333333333333,
-1.78327315618341));
#56236=CARTESIAN_POINT('Ctrl Pts',(3.29885386921513,0.333333333333333,-1.78327315618341));
#56237=CARTESIAN_POINT('Ctrl Pts',(3.29885386921513,0.666666666666667,-1.78327315618341));
#56238=CARTESIAN_POINT('Ctrl Pts',(3.29885386921513,1.,-1.78327315618341));
#56239=CARTESIAN_POINT('',(3.62024382630768,1.,-2.12928030988903));
#56240=CARTESIAN_POINT('',(3.62024382630768,0.,-2.12928030988903));
#56241=CARTESIAN_POINT('Ctrl Pts',(3.29885386921514,1.,-1.78327315618341));
#56242=CARTESIAN_POINT('Ctrl Pts',(3.29890219175423,1.,-1.78326534445518));
#56243=CARTESIAN_POINT('Ctrl Pts',(3.29909749657808,1.,-1.78329283591905));
#56244=CARTESIAN_POINT('Ctrl Pts',(3.299705498242,1.,-1.78353803106924));
#56245=CARTESIAN_POINT('Ctrl Pts',(3.30119637003394,1.,-1.78432384788174));
#56246=CARTESIAN_POINT('Ctrl Pts',(3.30422155559112,1.,-1.78610045419846));
#56247=CARTESIAN_POINT('Ctrl Pts',(3.30873412266788,1.,-1.78888832245873));
#56248=CARTESIAN_POINT('Ctrl Pts',(3.31428038326424,1.,-1.79242331349949));
#56249=CARTESIAN_POINT('Ctrl Pts',(3.3205535510082,1.,-1.79652817033251));
#56250=CARTESIAN_POINT('Ctrl Pts',(3.32721088039578,1.,-1.80100380443406));
#56251=CARTESIAN_POINT('Ctrl Pts',(3.33392460276808,1.,-1.80565802981102));
#56252=CARTESIAN_POINT('Ctrl Pts',(3.34043216147606,1.,-1.81033399625352));
#56253=CARTESIAN_POINT('Ctrl Pts',(3.34660014370673,1.,-1.81494618732853));
#56254=CARTESIAN_POINT('Ctrl Pts',(3.35243086937598,1.,-1.81948458796829));
#56255=CARTESIAN_POINT('Ctrl Pts',(3.35800801557424,1.,-1.82398496829301));
#56256=CARTESIAN_POINT('Ctrl Pts',(3.36345722124158,1.,-1.82850752153199));
#56257=CARTESIAN_POINT('Ctrl Pts',(3.36890396271836,1.,-1.83311391452322));
#56258=CARTESIAN_POINT('Ctrl Pts',(3.37442462015853,1.,-1.83784072967077));
#56259=CARTESIAN_POINT('Ctrl Pts',(3.38002968341157,1.,-1.84269016931643));
#56260=CARTESIAN_POINT('Ctrl Pts',(3.38569092349592,1.,-1.84764441927753));
#56261=CARTESIAN_POINT('Ctrl Pts',(3.39135802549398,1.,-1.85267433291769));
#56262=CARTESIAN_POINT('Ctrl Pts',(3.39697816833067,1.,-1.85774972037062));
#56263=CARTESIAN_POINT('Ctrl Pts',(3.40251742305476,1.,-1.86285057051245));
#56264=CARTESIAN_POINT('Ctrl Pts',(3.40797080000549,1.,-1.86797231196654));
#56265=CARTESIAN_POINT('Ctrl Pts',(3.41335043875209,1.,-1.87311957248121));
#56266=CARTESIAN_POINT('Ctrl Pts',(3.41867858383771,1.,-1.87830245689344));
#56267=CARTESIAN_POINT('Ctrl Pts',(3.42397908819736,1.,-1.8835320506206));
#56268=CARTESIAN_POINT('Ctrl Pts',(3.42926852222158,1.,-1.88881571322009));
#56269=CARTESIAN_POINT('Ctrl Pts',(3.43455074411571,1.,-1.89415420002542));
#56270=CARTESIAN_POINT('Ctrl Pts',(3.4398218567809,1.,-1.89954426803384));
#56271=CARTESIAN_POINT('Ctrl Pts',(3.44507323983367,1.,-1.90498026502305));
#56272=CARTESIAN_POINT('Ctrl Pts',(3.45029522038888,1.,-1.91045605593639));
#56273=CARTESIAN_POINT('Ctrl Pts',(3.4554807430995,1.,-1.91596694784064));
#56274=CARTESIAN_POINT('Ctrl Pts',(3.46062821722485,1.,-1.92151118213212));
#56275=CARTESIAN_POINT('Ctrl Pts',(3.46573953254084,1.,-1.92708888591158));
#56276=CARTESIAN_POINT('Ctrl Pts',(3.47081872409781,1.,-1.93270136427081));
#56277=CARTESIAN_POINT('Ctrl Pts',(3.47587040389915,1.,-1.93835026973887));
#56278=CARTESIAN_POINT('Ctrl Pts',(3.48089825770416,1.,-1.94403680554065));
#56279=CARTESIAN_POINT('Ctrl Pts',(3.48590361610814,1.,-1.94976096795911));
#56280=CARTESIAN_POINT('Ctrl Pts',(3.49088618670987,1.,-1.95552193112084));
#56281=CARTESIAN_POINT('Ctrl Pts',(3.49584466573064,1.,-1.961318367765));
#56282=CARTESIAN_POINT('Ctrl Pts',(3.50077740176267,1.,-1.96714879724052));
#56283=CARTESIAN_POINT('Ctrl Pts',(3.5056830186108,1.,-1.97301191162968));
#56284=CARTESIAN_POINT('Ctrl Pts',(3.51056110478287,1.,-1.97890693666288));
#56285=CARTESIAN_POINT('Ctrl Pts',(3.51541198728301,1.,-1.9848335106103));
#56286=CARTESIAN_POINT('Ctrl Pts',(3.52023644289142,1.,-1.99079153006112));
#56287=CARTESIAN_POINT('Ctrl Pts',(3.52503542491728,1.,-1.99678100339296));
#56288=CARTESIAN_POINT('Ctrl Pts',(3.52980980250224,1.,-2.00280191090366));
#56289=CARTESIAN_POINT('Ctrl Pts',(3.53456004727424,1.,-2.00885403604746));
#56290=CARTESIAN_POINT('Ctrl Pts',(3.53928627453642,1.,-2.01493698847351));
#56291=CARTESIAN_POINT('Ctrl Pts',(3.54398838254136,1.,-2.02105027983104));
#56292=CARTESIAN_POINT('Ctrl Pts',(3.54866616282227,1.,-2.02719338376175));
#56293=CARTESIAN_POINT('Ctrl Pts',(3.55331941293949,1.,-2.03336579658133));
#56294=CARTESIAN_POINT('Ctrl Pts',(3.55794807264844,1.,-2.03956711119976));
#56295=CARTESIAN_POINT('Ctrl Pts',(3.56255223871505,1.,-2.04579702158876));
#56296=CARTESIAN_POINT('Ctrl Pts',(3.56713209977904,1.,-2.05205528172911));
#56297=CARTESIAN_POINT('Ctrl Pts',(3.5716878942334,1.,-2.05834167687425));
#56298=CARTESIAN_POINT('Ctrl Pts',(3.57621986224402,1.,-2.06465599229234));
#56299=CARTESIAN_POINT('Ctrl Pts',(3.58072819250872,1.,-2.07099797606));
#56300=CARTESIAN_POINT('Ctrl Pts',(3.58521300039988,1.,-2.07736732842524));
#56301=CARTESIAN_POINT('Ctrl Pts',(3.58967435355834,1.,-2.08376373049196));
#56302=CARTESIAN_POINT('Ctrl Pts',(3.5941122862608,1.,-2.09018686331706));
#56303=CARTESIAN_POINT('Ctrl Pts',(3.59852681775396,1.,-2.09663642986579));
#56304=CARTESIAN_POINT('Ctrl Pts',(3.60291797087849,1.,-2.10311217727687));
#56305=CARTESIAN_POINT('Ctrl Pts',(3.60728578530968,1.,-2.10961391333497));
#56306=CARTESIAN_POINT('Ctrl Pts',(3.61163030607452,1.,-2.11614149813928));
#56307=CARTESIAN_POINT('Ctrl Pts',(3.61508732215187,1.,-2.12138417125349));
#56308=CARTESIAN_POINT('Ctrl Pts',(3.61766963589442,1.,-2.12532774376144));
#56309=CARTESIAN_POINT('Ctrl Pts',(3.61938653648716,1.,-2.12796193131142));
#56310=CARTESIAN_POINT('Ctrl Pts',(3.62024382630768,1.,-2.12928030988903));
#56311=CARTESIAN_POINT('Origin',(3.62024382630768,0.,-2.12928030988903));
#56312=CARTESIAN_POINT('',(3.54075895182139,1.,-2.25898783642071));
#56313=CARTESIAN_POINT('Origin',(0.,0.,0.));
#56314=CARTESIAN_POINT('',(3.38171594275687,1.,-1.62064718014256));
#56315=CARTESIAN_POINT('Origin',(0.,1.,0.));
#56316=CARTESIAN_POINT('Ctrl Pts',(3.38171594275687,1.,-1.62064718014256));
#56317=CARTESIAN_POINT('Ctrl Pts',(3.38171594275687,0.666666666666667,-1.62064718014256));
#56318=CARTESIAN_POINT('Ctrl Pts',(3.38171594275687,0.333333333333333,-1.62064718014256));
#56319=CARTESIAN_POINT('Ctrl Pts',(3.38171594275687,-0.333333333333333,
-1.62064718014256));
#56320=CARTESIAN_POINT('Ctrl Pts',(3.38171594275687,-0.666666666666667,
-1.62064718014255));
#56321=CARTESIAN_POINT('Ctrl Pts',(3.38171594275687,-1.,-1.62064718014255));
#56322=CARTESIAN_POINT('Ctrl Pts',(3.85054988729471,-1.,-1.67727921511438));
#56323=CARTESIAN_POINT('Ctrl Pts',(3.85054988729471,1.,-1.67727921511438));
#56324=CARTESIAN_POINT('Ctrl Pts',(3.84897939431104,-1.,-1.6773605765671));
#56325=CARTESIAN_POINT('Ctrl Pts',(3.84897939431104,1.,-1.6773605765671));
#56326=CARTESIAN_POINT('Ctrl Pts',(3.84583912297567,-1.,-1.67751991140661));
#56327=CARTESIAN_POINT('Ctrl Pts',(3.84583912297567,1.,-1.67751991140661));
#56328=CARTESIAN_POINT('Ctrl Pts',(3.8411308598706,-1.,-1.67774874946867));
#56329=CARTESIAN_POINT('Ctrl Pts',(3.8411308598706,1.,-1.67774874946867));
#56330=CARTESIAN_POINT('Ctrl Pts',(3.83485746516115,-1.,-1.67803353065273));
#56331=CARTESIAN_POINT('Ctrl Pts',(3.83485746516115,1.,-1.67803353065273));
#56332=CARTESIAN_POINT('Ctrl Pts',(3.82702289288453,-1.,-1.67835555760094));
#56333=CARTESIAN_POINT('Ctrl Pts',(3.82702289288453,1.,-1.67835555760094));
#56334=CARTESIAN_POINT('Ctrl Pts',(3.81919554100522,-1.,-1.67864354606363));
#56335=CARTESIAN_POINT('Ctrl Pts',(3.81919554100522,1.,-1.67864354606363));
#56336=CARTESIAN_POINT('Ctrl Pts',(3.81137549624273,-1.,-1.67889737738311));
#56337=CARTESIAN_POINT('Ctrl Pts',(3.81137549624273,1.,-1.67889737738311));
#56338=CARTESIAN_POINT('Ctrl Pts',(3.80356289078481,-1.,-1.67911690648128));
#56339=CARTESIAN_POINT('Ctrl Pts',(3.80356289078481,1.,-1.67911690648128));
#56340=CARTESIAN_POINT('Ctrl Pts',(3.7957579157763,-1.,-1.67930196625204));
#56341=CARTESIAN_POINT('Ctrl Pts',(3.7957579157763,1.,-1.67930196625204));
#56342=CARTESIAN_POINT('Ctrl Pts',(3.78796080021026,-1.,-1.67945236653175));
#56343=CARTESIAN_POINT('Ctrl Pts',(3.78796080021026,1.,-1.67945236653175));
#56344=CARTESIAN_POINT('Ctrl Pts',(3.78017178196859,-1.,-1.67956789211943));
#56345=CARTESIAN_POINT('Ctrl Pts',(3.78017178196859,1.,-1.67956789211943));
#56346=CARTESIAN_POINT('Ctrl Pts',(3.77239107928394,-1.,-1.67964830084946));
#56347=CARTESIAN_POINT('Ctrl Pts',(3.77239107928394,1.,-1.67964830084946));
#56348=CARTESIAN_POINT('Ctrl Pts',(3.76461886684523,-1.,-1.67969332319322));
#56349=CARTESIAN_POINT('Ctrl Pts',(3.76461886684523,1.,-1.67969332319322));
#56350=CARTESIAN_POINT('Ctrl Pts',(3.75685523754816,-1.,-1.67970265841379));
#56351=CARTESIAN_POINT('Ctrl Pts',(3.75685523754816,1.,-1.67970265841379));
#56352=CARTESIAN_POINT('Ctrl Pts',(3.74910022394845,-1.,-1.67967598599665));
#56353=CARTESIAN_POINT('Ctrl Pts',(3.74910022394845,1.,-1.67967598599665));
#56354=CARTESIAN_POINT('Ctrl Pts',(3.74135385965622,-1.,-1.67961298685316));
#56355=CARTESIAN_POINT('Ctrl Pts',(3.74135385965622,1.,-1.67961298685316));
#56356=CARTESIAN_POINT('Ctrl Pts',(3.73361623282617,-1.,-1.67951336376434));
#56357=CARTESIAN_POINT('Ctrl Pts',(3.73361623282617,1.,-1.67951336376434));
#56358=CARTESIAN_POINT('Ctrl Pts',(3.72588753416339,-1.,-1.67937685856627));
#56359=CARTESIAN_POINT('Ctrl Pts',(3.72588753416339,1.,-1.67937685856627));
#56360=CARTESIAN_POINT('Ctrl Pts',(3.71816812842188,-1.,-1.6792032807165));
#56361=CARTESIAN_POINT('Ctrl Pts',(3.71816812842188,1.,-1.6792032807165));
#56362=CARTESIAN_POINT('Ctrl Pts',(3.71045854208195,-1.,-1.67899249793398));
#56363=CARTESIAN_POINT('Ctrl Pts',(3.71045854208195,1.,-1.67899249793398));
#56364=CARTESIAN_POINT('Ctrl Pts',(3.70275932350998,-1.,-1.6787443694862));
#56365=CARTESIAN_POINT('Ctrl Pts',(3.70275932350998,1.,-1.6787443694862));
#56366=CARTESIAN_POINT('Ctrl Pts',(3.69507092759545,-1.,-1.67845869064304));
#56367=CARTESIAN_POINT('Ctrl Pts',(3.69507092759545,1.,-1.67845869064304));
#56368=CARTESIAN_POINT('Ctrl Pts',(3.68739360236505,-1.,-1.67813513867973));
#56369=CARTESIAN_POINT('Ctrl Pts',(3.68739360236505,1.,-1.67813513867973));
#56370=CARTESIAN_POINT('Ctrl Pts',(3.6797272457918,-1.,-1.67777320475872));
#56371=CARTESIAN_POINT('Ctrl Pts',(3.6797272457918,1.,-1.67777320475872));
#56372=CARTESIAN_POINT('Ctrl Pts',(3.67207136294639,-1.,-1.67737217414901));
#56373=CARTESIAN_POINT('Ctrl Pts',(3.67207136294639,1.,-1.67737217414901));
#56374=CARTESIAN_POINT('Ctrl Pts',(3.66442538671018,-1.,-1.67693128053153));
#56375=CARTESIAN_POINT('Ctrl Pts',(3.66442538671018,1.,-1.67693128053153));
#56376=CARTESIAN_POINT('Ctrl Pts',(3.65678894416442,-1.,-1.67644983469459));
#56377=CARTESIAN_POINT('Ctrl Pts',(3.65678894416442,1.,-1.67644983469459));
#56378=CARTESIAN_POINT('Ctrl Pts',(3.64916213574663,-1.,-1.6759273594669));
#56379=CARTESIAN_POINT('Ctrl Pts',(3.64916213574663,1.,-1.6759273594669));
#56380=CARTESIAN_POINT('Ctrl Pts',(3.6415458297232,-1.,-1.6753637326484));
#56381=CARTESIAN_POINT('Ctrl Pts',(3.6415458297232,1.,-1.6753637326484));
#56382=CARTESIAN_POINT('Ctrl Pts',(3.63394189312902,-1.,-1.67475929882962));
#56383=CARTESIAN_POINT('Ctrl Pts',(3.63394189312902,1.,-1.67475929882962));
#56384=CARTESIAN_POINT('Ctrl Pts',(3.62635249450908,-1.,-1.67411452372265));
#56385=CARTESIAN_POINT('Ctrl Pts',(3.62635249450908,1.,-1.67411452372265));
#56386=CARTESIAN_POINT('Ctrl Pts',(3.61877947398179,-1.,-1.67342968196223));
#56387=CARTESIAN_POINT('Ctrl Pts',(3.61877947398179,1.,-1.67342968196223));
#56388=CARTESIAN_POINT('Ctrl Pts',(3.61122367156182,-1.,-1.67270452466968));
#56389=CARTESIAN_POINT('Ctrl Pts',(3.61122367156182,1.,-1.67270452466968));
#56390=CARTESIAN_POINT('Ctrl Pts',(3.60368430815203,-1.,-1.67193797318598));
#56391=CARTESIAN_POINT('Ctrl Pts',(3.60368430815203,1.,-1.67193797318598));
#56392=CARTESIAN_POINT('Ctrl Pts',(3.59615824388808,-1.,-1.67112775290706));
#56393=CARTESIAN_POINT('Ctrl Pts',(3.59615824388808,1.,-1.67112775290706));
#56394=CARTESIAN_POINT('Ctrl Pts',(3.5886414309783,-1.,-1.67027110397602));
#56395=CARTESIAN_POINT('Ctrl Pts',(3.5886414309783,1.,-1.67027110397602));
#56396=CARTESIAN_POINT('Ctrl Pts',(3.58113044183823,-1.,-1.66936552908228));
#56397=CARTESIAN_POINT('Ctrl Pts',(3.58113044183823,1.,-1.66936552908228));
#56398=CARTESIAN_POINT('Ctrl Pts',(3.57362406285884,-1.,-1.66840957407299));
#56399=CARTESIAN_POINT('Ctrl Pts',(3.57362406285884,1.,-1.66840957407299));
#56400=CARTESIAN_POINT('Ctrl Pts',(3.56612465179429,-1.,-1.66740349220308));
#56401=CARTESIAN_POINT('Ctrl Pts',(3.56612465179429,1.,-1.66740349220308));
#56402=CARTESIAN_POINT('Ctrl Pts',(3.55864015233617,-1.,-1.66635023293121));
#56403=CARTESIAN_POINT('Ctrl Pts',(3.55864015233617,1.,-1.66635023293121));
#56404=CARTESIAN_POINT('Ctrl Pts',(3.5511812134288,-1.,-1.66525401569004));
#56405=CARTESIAN_POINT('Ctrl Pts',(3.5511812134288,1.,-1.66525401569004));
#56406=CARTESIAN_POINT('Ctrl Pts',(3.5437574747503,-1.,-1.66411849222334));
#56407=CARTESIAN_POINT('Ctrl Pts',(3.5437574747503,1.,-1.66411849222334));
#56408=CARTESIAN_POINT('Ctrl Pts',(3.53637385060225,-1.,-1.66294490916113));
#56409=CARTESIAN_POINT('Ctrl Pts',(3.53637385060225,1.,-1.66294490916113));
#56410=CARTESIAN_POINT('Ctrl Pts',(3.52902746211081,-1.,-1.66173058912365));
#56411=CARTESIAN_POINT('Ctrl Pts',(3.52902746211081,1.,-1.66173058912365));
#56412=CARTESIAN_POINT('Ctrl Pts',(3.52170261543787,-1.,-1.66046645222266));
#56413=CARTESIAN_POINT('Ctrl Pts',(3.52170261543787,1.,-1.66046645222266));
#56414=CARTESIAN_POINT('Ctrl Pts',(3.51437632188903,-1.,-1.65913971687324));
#56415=CARTESIAN_POINT('Ctrl Pts',(3.51437632188903,1.,-1.65913971687324));
#56416=CARTESIAN_POINT('Ctrl Pts',(3.5070273314651,-1.,-1.65773832633617));
#56417=CARTESIAN_POINT('Ctrl Pts',(3.5070273314651,1.,-1.65773832633617));
#56418=CARTESIAN_POINT('Ctrl Pts',(3.49964476477929,-1.,-1.65625517961583));
#56419=CARTESIAN_POINT('Ctrl Pts',(3.49964476477929,1.,-1.65625517961583));
#56420=CARTESIAN_POINT('Ctrl Pts',(3.49223525300194,-1.,-1.65469162644476));
#56421=CARTESIAN_POINT('Ctrl Pts',(3.49223525300194,1.,-1.65469162644476));
#56422=CARTESIAN_POINT('Ctrl Pts',(3.48483492840942,-1.,-1.65306335367762));
#56423=CARTESIAN_POINT('Ctrl Pts',(3.48483492840942,1.,-1.65306335367762));
#56424=CARTESIAN_POINT('Ctrl Pts',(3.47749926256543,-1.,-1.65139534930353));
#56425=CARTESIAN_POINT('Ctrl Pts',(3.47749926256543,1.,-1.65139534930353));
#56426=CARTESIAN_POINT('Ctrl Pts',(3.47028140996055,-1.,-1.64971118698285));
#56427=CARTESIAN_POINT('Ctrl Pts',(3.47028140996055,1.,-1.64971118698285));
#56428=CARTESIAN_POINT('Ctrl Pts',(3.46321237515029,-1.,-1.64802323352752));
#56429=CARTESIAN_POINT('Ctrl Pts',(3.46321237515029,1.,-1.64802323352752));
#56430=CARTESIAN_POINT('Ctrl Pts',(3.4562842106239,-1.,-1.64632429697506));
#56431=CARTESIAN_POINT('Ctrl Pts',(3.4562842106239,1.,-1.64632429697506));
#56432=CARTESIAN_POINT('Ctrl Pts',(3.44942242546693,-1.,-1.64457408708059));
#56433=CARTESIAN_POINT('Ctrl Pts',(3.44942242546693,1.,-1.64457408708059));
#56434=CARTESIAN_POINT('Ctrl Pts',(3.44250337701736,-1.,-1.64270733821042));
#56435=CARTESIAN_POINT('Ctrl Pts',(3.44250337701736,1.,-1.64270733821042));
#56436=CARTESIAN_POINT('Ctrl Pts',(3.43540451921397,-1.,-1.64065778701952));
#56437=CARTESIAN_POINT('Ctrl Pts',(3.43540451921397,1.,-1.64065778701952));
#56438=CARTESIAN_POINT('Ctrl Pts',(3.42804772926213,-1.,-1.6383787624689));
#56439=CARTESIAN_POINT('Ctrl Pts',(3.42804772926213,1.,-1.6383787624689));
#56440=CARTESIAN_POINT('Ctrl Pts',(3.4204397459095,-1.,-1.63586250099804));
#56441=CARTESIAN_POINT('Ctrl Pts',(3.4204397459095,1.,-1.63586250099804));
#56442=CARTESIAN_POINT('Ctrl Pts',(3.41272817148719,-1.,-1.63316667054156));
#56443=CARTESIAN_POINT('Ctrl Pts',(3.41272817148719,1.,-1.63316667054156));
#56444=CARTESIAN_POINT('Ctrl Pts',(3.40519422740596,-1.,-1.63041148964996));
#56445=CARTESIAN_POINT('Ctrl Pts',(3.40519422740596,1.,-1.63041148964996));
#56446=CARTESIAN_POINT('Ctrl Pts',(3.39818605298342,-1.,-1.62774916464571));
#56447=CARTESIAN_POINT('Ctrl Pts',(3.39818605298342,1.,-1.62774916464571));
#56448=CARTESIAN_POINT('Ctrl Pts',(3.39206617497078,-1.,-1.62533996116793));
#56449=CARTESIAN_POINT('Ctrl Pts',(3.39206617497078,1.,-1.62533996116793));
#56450=CARTESIAN_POINT('Ctrl Pts',(3.38715832178929,-1.,-1.62332788556183));
#56451=CARTESIAN_POINT('Ctrl Pts',(3.38715832178929,1.,-1.62332788556183));
#56452=CARTESIAN_POINT('Ctrl Pts',(3.38368201668123,-1.,-1.62181089631134));
#56453=CARTESIAN_POINT('Ctrl Pts',(3.38368201668123,1.,-1.62181089631134));
#56454=CARTESIAN_POINT('Ctrl Pts',(3.38212861099481,-1.,-1.62103022180917));
#56455=CARTESIAN_POINT('Ctrl Pts',(3.38212861099481,1.,-1.62103022180917));
#56456=CARTESIAN_POINT('Ctrl Pts',(3.38166984193496,-1.,-1.6206953236804));
#56457=CARTESIAN_POINT('Ctrl Pts',(3.38166984193496,1.,-1.6206953236804));
#56458=CARTESIAN_POINT('Ctrl Pts',(3.38167767992546,-1.,-1.62058335162421));
#56459=CARTESIAN_POINT('Ctrl Pts',(3.38167767992546,1.,-1.62058335162421));
#56460=CARTESIAN_POINT('Ctrl Pts',(3.38176002566879,-1.,-1.62055519152809));
#56461=CARTESIAN_POINT('Ctrl Pts',(3.38176002566879,1.,-1.62055519152809));
#56462=CARTESIAN_POINT('',(3.85054988729471,1.,-1.67727921511438));
#56463=CARTESIAN_POINT('Ctrl Pts',(3.85054988729471,1.,-1.67727921511438));
#56464=CARTESIAN_POINT('Ctrl Pts',(3.84897939431104,1.,-1.6773605765671));
#56465=CARTESIAN_POINT('Ctrl Pts',(3.84583912297567,1.,-1.67751991140661));
#56466=CARTESIAN_POINT('Ctrl Pts',(3.8411308598706,1.,-1.67774874946867));
#56467=CARTESIAN_POINT('Ctrl Pts',(3.83485746516115,1.,-1.67803353065273));
#56468=CARTESIAN_POINT('Ctrl Pts',(3.82702289288453,1.,-1.67835555760094));
#56469=CARTESIAN_POINT('Ctrl Pts',(3.81919554100522,1.,-1.67864354606363));
#56470=CARTESIAN_POINT('Ctrl Pts',(3.81137549624273,1.,-1.67889737738311));
#56471=CARTESIAN_POINT('Ctrl Pts',(3.80356289078481,1.,-1.67911690648128));
#56472=CARTESIAN_POINT('Ctrl Pts',(3.7957579157763,1.,-1.67930196625204));
#56473=CARTESIAN_POINT('Ctrl Pts',(3.78796080021026,1.,-1.67945236653175));
#56474=CARTESIAN_POINT('Ctrl Pts',(3.78017178196859,1.,-1.67956789211943));
#56475=CARTESIAN_POINT('Ctrl Pts',(3.77239107928394,1.,-1.67964830084946));
#56476=CARTESIAN_POINT('Ctrl Pts',(3.76461886684523,1.,-1.67969332319322));
#56477=CARTESIAN_POINT('Ctrl Pts',(3.75685523754816,1.,-1.67970265841379));
#56478=CARTESIAN_POINT('Ctrl Pts',(3.74910022394845,1.,-1.67967598599665));
#56479=CARTESIAN_POINT('Ctrl Pts',(3.74135385965622,1.,-1.67961298685316));
#56480=CARTESIAN_POINT('Ctrl Pts',(3.73361623282617,1.,-1.67951336376434));
#56481=CARTESIAN_POINT('Ctrl Pts',(3.72588753416339,1.,-1.67937685856627));
#56482=CARTESIAN_POINT('Ctrl Pts',(3.71816812842188,1.,-1.6792032807165));
#56483=CARTESIAN_POINT('Ctrl Pts',(3.71045854208195,1.,-1.67899249793398));
#56484=CARTESIAN_POINT('Ctrl Pts',(3.70275932350998,1.,-1.6787443694862));
#56485=CARTESIAN_POINT('Ctrl Pts',(3.69507092759545,1.,-1.67845869064304));
#56486=CARTESIAN_POINT('Ctrl Pts',(3.68739360236505,1.,-1.67813513867973));
#56487=CARTESIAN_POINT('Ctrl Pts',(3.6797272457918,1.,-1.67777320475872));
#56488=CARTESIAN_POINT('Ctrl Pts',(3.67207136294639,1.,-1.67737217414901));
#56489=CARTESIAN_POINT('Ctrl Pts',(3.66442538671018,1.,-1.67693128053153));
#56490=CARTESIAN_POINT('Ctrl Pts',(3.65678894416442,1.,-1.67644983469459));
#56491=CARTESIAN_POINT('Ctrl Pts',(3.64916213574663,1.,-1.6759273594669));
#56492=CARTESIAN_POINT('Ctrl Pts',(3.6415458297232,1.,-1.6753637326484));
#56493=CARTESIAN_POINT('Ctrl Pts',(3.63394189312902,1.,-1.67475929882962));
#56494=CARTESIAN_POINT('Ctrl Pts',(3.62635249450908,1.,-1.67411452372265));
#56495=CARTESIAN_POINT('Ctrl Pts',(3.61877947398179,1.,-1.67342968196223));
#56496=CARTESIAN_POINT('Ctrl Pts',(3.61122367156182,1.,-1.67270452466968));
#56497=CARTESIAN_POINT('Ctrl Pts',(3.60368430815203,1.,-1.67193797318598));
#56498=CARTESIAN_POINT('Ctrl Pts',(3.59615824388808,1.,-1.67112775290706));
#56499=CARTESIAN_POINT('Ctrl Pts',(3.5886414309783,1.,-1.67027110397602));
#56500=CARTESIAN_POINT('Ctrl Pts',(3.58113044183823,1.,-1.66936552908228));
#56501=CARTESIAN_POINT('Ctrl Pts',(3.57362406285884,1.,-1.66840957407299));
#56502=CARTESIAN_POINT('Ctrl Pts',(3.56612465179429,1.,-1.66740349220308));
#56503=CARTESIAN_POINT('Ctrl Pts',(3.55864015233617,1.,-1.66635023293121));
#56504=CARTESIAN_POINT('Ctrl Pts',(3.5511812134288,1.,-1.66525401569004));
#56505=CARTESIAN_POINT('Ctrl Pts',(3.5437574747503,1.,-1.66411849222334));
#56506=CARTESIAN_POINT('Ctrl Pts',(3.53637385060225,1.,-1.66294490916113));
#56507=CARTESIAN_POINT('Ctrl Pts',(3.52902746211081,1.,-1.66173058912365));
#56508=CARTESIAN_POINT('Ctrl Pts',(3.52170261543787,1.,-1.66046645222266));
#56509=CARTESIAN_POINT('Ctrl Pts',(3.51437632188903,1.,-1.65913971687324));
#56510=CARTESIAN_POINT('Ctrl Pts',(3.5070273314651,1.,-1.65773832633617));
#56511=CARTESIAN_POINT('Ctrl Pts',(3.49964476477929,1.,-1.65625517961583));
#56512=CARTESIAN_POINT('Ctrl Pts',(3.49223525300194,1.,-1.65469162644476));
#56513=CARTESIAN_POINT('Ctrl Pts',(3.48483492840942,1.,-1.65306335367762));
#56514=CARTESIAN_POINT('Ctrl Pts',(3.47749926256543,1.,-1.65139534930353));
#56515=CARTESIAN_POINT('Ctrl Pts',(3.47028140996055,1.,-1.64971118698285));
#56516=CARTESIAN_POINT('Ctrl Pts',(3.46321237515029,1.,-1.64802323352752));
#56517=CARTESIAN_POINT('Ctrl Pts',(3.4562842106239,1.,-1.64632429697506));
#56518=CARTESIAN_POINT('Ctrl Pts',(3.44942242546693,1.,-1.64457408708059));
#56519=CARTESIAN_POINT('Ctrl Pts',(3.44250337701736,1.,-1.64270733821042));
#56520=CARTESIAN_POINT('Ctrl Pts',(3.43540451921397,1.,-1.64065778701952));
#56521=CARTESIAN_POINT('Ctrl Pts',(3.42804772926213,1.,-1.6383787624689));
#56522=CARTESIAN_POINT('Ctrl Pts',(3.4204397459095,1.,-1.63586250099804));
#56523=CARTESIAN_POINT('Ctrl Pts',(3.41272817148719,1.,-1.63316667054156));
#56524=CARTESIAN_POINT('Ctrl Pts',(3.40519422740596,1.,-1.63041148964996));
#56525=CARTESIAN_POINT('Ctrl Pts',(3.39818605298342,1.,-1.62774916464571));
#56526=CARTESIAN_POINT('Ctrl Pts',(3.39206617497078,1.,-1.62533996116793));
#56527=CARTESIAN_POINT('Ctrl Pts',(3.38715832178929,1.,-1.62332788556183));
#56528=CARTESIAN_POINT('Ctrl Pts',(3.3839428576331,1.,-1.62192472202795));
#56529=CARTESIAN_POINT('Ctrl Pts',(3.38243080602536,1.,-1.62118047294574));
#56530=CARTESIAN_POINT('Ctrl Pts',(3.38187506457001,1.,-1.62083271136059));
#56531=CARTESIAN_POINT('Ctrl Pts',(3.38173802621242,1.,-1.62069086551627));
#56532=CARTESIAN_POINT('Ctrl Pts',(3.38171594275687,1.,-1.62064718014256));
#56533=CARTESIAN_POINT('',(3.85054988729471,0.,-1.67727921511438));
#56534=CARTESIAN_POINT('Ctrl Pts',(3.53717101171257,-1.,-1.24535988127942));
#56535=CARTESIAN_POINT('Ctrl Pts',(3.53717101171257,1.,-1.24535988127942));
#56536=CARTESIAN_POINT('Ctrl Pts',(3.53713269667534,-1.,-1.24528174185147));
#56537=CARTESIAN_POINT('Ctrl Pts',(3.53713269667534,1.,-1.24528174185147));
#56538=CARTESIAN_POINT('Ctrl Pts',(3.53720633058152,-1.,-1.2451970233558));
#56539=CARTESIAN_POINT('Ctrl Pts',(3.53720633058152,1.,-1.2451970233558));
#56540=CARTESIAN_POINT('Ctrl Pts',(3.53776753803428,-1.,-1.24528461333177));
#56541=CARTESIAN_POINT('Ctrl Pts',(3.53776753803428,1.,-1.24528461333177));
#56542=CARTESIAN_POINT('Ctrl Pts',(3.53941798196293,-1.,-1.24583101679199));
#56543=CARTESIAN_POINT('Ctrl Pts',(3.53941798196293,1.,-1.24583101679199));
#56544=CARTESIAN_POINT('Ctrl Pts',(3.54294877426113,-1.,-1.2472164623202));
#56545=CARTESIAN_POINT('Ctrl Pts',(3.54294877426113,1.,-1.2472164623202));
#56546=CARTESIAN_POINT('Ctrl Pts',(3.54784190282889,-1.,-1.24926408627938));
#56547=CARTESIAN_POINT('Ctrl Pts',(3.54784190282889,1.,-1.24926408627938));
#56548=CARTESIAN_POINT('Ctrl Pts',(3.5538728741862,-1.,-1.25188792940508));
#56549=CARTESIAN_POINT('Ctrl Pts',(3.5538728741862,1.,-1.25188792940508));
#56550=CARTESIAN_POINT('Ctrl Pts',(3.56071094990825,-1.,-1.25496090899873));
#56551=CARTESIAN_POINT('Ctrl Pts',(3.56071094990825,1.,-1.25496090899873));
#56552=CARTESIAN_POINT('Ctrl Pts',(3.56798645995025,-1.,-1.25834000485626));
#56553=CARTESIAN_POINT('Ctrl Pts',(3.56798645995025,1.,-1.25834000485626));
#56554=CARTESIAN_POINT('Ctrl Pts',(3.5753456065164,-1.,-1.26188667142784));
#56555=CARTESIAN_POINT('Ctrl Pts',(3.5753456065164,1.,-1.26188667142784));
#56556=CARTESIAN_POINT('Ctrl Pts',(3.58250452868699,-1.,-1.26548706249891));
#56557=CARTESIAN_POINT('Ctrl Pts',(3.58250452868699,1.,-1.26548706249891));
#56558=CARTESIAN_POINT('Ctrl Pts',(3.5893180784647,-1.,-1.26907758484766));
#56559=CARTESIAN_POINT('Ctrl Pts',(3.5893180784647,1.,-1.26907758484766));
#56560=CARTESIAN_POINT('Ctrl Pts',(3.59578698050164,-1.,-1.27264798379365));
#56561=CARTESIAN_POINT('Ctrl Pts',(3.59578698050164,1.,-1.27264798379365));
#56562=CARTESIAN_POINT('Ctrl Pts',(3.60199947736404,-1.,-1.27622049908664));
#56563=CARTESIAN_POINT('Ctrl Pts',(3.60199947736404,1.,-1.27622049908664));
#56564=CARTESIAN_POINT('Ctrl Pts',(3.60808907746372,-1.,-1.27983492861703));
#56565=CARTESIAN_POINT('Ctrl Pts',(3.60808907746372,1.,-1.27983492861703));
#56566=CARTESIAN_POINT('Ctrl Pts',(3.61418935913793,-1.,-1.28353255117754));
#56567=CARTESIAN_POINT('Ctrl Pts',(3.61418935913793,1.,-1.28353255117754));
#56568=CARTESIAN_POINT('Ctrl Pts',(3.62038148492295,-1.,-1.2873375502936));
#56569=CARTESIAN_POINT('Ctrl Pts',(3.62038148492295,1.,-1.2873375502936));
#56570=CARTESIAN_POINT('Ctrl Pts',(3.62667616004299,-1.,-1.29125046021853));
#56571=CARTESIAN_POINT('Ctrl Pts',(3.62667616004299,1.,-1.29125046021853));
#56572=CARTESIAN_POINT('Ctrl Pts',(3.63304271630995,-1.,-1.29525810207744));
#56573=CARTESIAN_POINT('Ctrl Pts',(3.63304271630995,1.,-1.29525810207744));
#56574=CARTESIAN_POINT('Ctrl Pts',(3.6394268987279,-1.,-1.29933955906463));
#56575=CARTESIAN_POINT('Ctrl Pts',(3.6394268987279,1.,-1.29933955906463));
#56576=CARTESIAN_POINT('Ctrl Pts',(3.64577181380125,-1.,-1.30347327603778));
#56577=CARTESIAN_POINT('Ctrl Pts',(3.64577181380125,1.,-1.30347327603778));
#56578=CARTESIAN_POINT('Ctrl Pts',(3.65204081987101,-1.,-1.30764479590051));
#56579=CARTESIAN_POINT('Ctrl Pts',(3.65204081987101,1.,-1.30764479590051));
#56580=CARTESIAN_POINT('Ctrl Pts',(3.65822827358655,-1.,-1.31185038411231));
#56581=CARTESIAN_POINT('Ctrl Pts',(3.65822827358655,1.,-1.31185038411231));
#56582=CARTESIAN_POINT('Ctrl Pts',(3.66434688899822,-1.,-1.31609271239922));
#56583=CARTESIAN_POINT('Ctrl Pts',(3.66434688899822,1.,-1.31609271239922));
#56584=CARTESIAN_POINT('Ctrl Pts',(3.67042021752668,-1.,-1.3203782813777));
#56585=CARTESIAN_POINT('Ctrl Pts',(3.67042021752668,1.,-1.3203782813777));
#56586=CARTESIAN_POINT('Ctrl Pts',(3.67647355257906,-1.,-1.32471430856413));
#56587=CARTESIAN_POINT('Ctrl Pts',(3.67647355257906,1.,-1.32471430856413));
#56588=CARTESIAN_POINT('Ctrl Pts',(3.68252441182534,-1.,-1.32910547072734));
#56589=CARTESIAN_POINT('Ctrl Pts',(3.68252441182534,1.,-1.32910547072734));
#56590=CARTESIAN_POINT('Ctrl Pts',(3.68857672413013,-1.,-1.33355191034515));
#56591=CARTESIAN_POINT('Ctrl Pts',(3.68857672413013,1.,-1.33355191034515));
#56592=CARTESIAN_POINT('Ctrl Pts',(3.69462613305692,-1.,-1.33805103398214));
#56593=CARTESIAN_POINT('Ctrl Pts',(3.69462613305692,1.,-1.33805103398214));
#56594=CARTESIAN_POINT('Ctrl Pts',(3.70066324015112,-1.,-1.3425986075293));
#56595=CARTESIAN_POINT('Ctrl Pts',(3.70066324015112,1.,-1.3425986075293));
#56596=CARTESIAN_POINT('Ctrl Pts',(3.7066775318825,-1.,-1.34719008463535));
#56597=CARTESIAN_POINT('Ctrl Pts',(3.7066775318825,1.,-1.34719008463535));
#56598=CARTESIAN_POINT('Ctrl Pts',(3.71266130563061,-1.,-1.35182193384426));
#56599=CARTESIAN_POINT('Ctrl Pts',(3.71266130563061,1.,-1.35182193384426));
#56600=CARTESIAN_POINT('Ctrl Pts',(3.71861271513318,-1.,-1.35649266705038));
#56601=CARTESIAN_POINT('Ctrl Pts',(3.71861271513318,1.,-1.35649266705038));
#56602=CARTESIAN_POINT('Ctrl Pts',(3.72453364678279,-1.,-1.36120211416354));
#56603=CARTESIAN_POINT('Ctrl Pts',(3.72453364678279,1.,-1.36120211416354));
#56604=CARTESIAN_POINT('Ctrl Pts',(3.73042829011293,-1.,-1.36595093298674));
#56605=CARTESIAN_POINT('Ctrl Pts',(3.73042829011293,1.,-1.36595093298674));
#56606=CARTESIAN_POINT('Ctrl Pts',(3.73630145885809,-1.,-1.37074003422739));
#56607=CARTESIAN_POINT('Ctrl Pts',(3.73630145885809,1.,-1.37074003422739));
#56608=CARTESIAN_POINT('Ctrl Pts',(3.7421569816256,-1.,-1.3755700297169));
#56609=CARTESIAN_POINT('Ctrl Pts',(3.7421569816256,1.,-1.3755700297169));
#56610=CARTESIAN_POINT('Ctrl Pts',(3.74799617204744,-1.,-1.38044070763302));
#56611=CARTESIAN_POINT('Ctrl Pts',(3.74799617204744,1.,-1.38044070763302));
#56612=CARTESIAN_POINT('Ctrl Pts',(3.75381861212728,-1.,-1.38535129801185));
#56613=CARTESIAN_POINT('Ctrl Pts',(3.75381861212728,1.,-1.38535129801185));
#56614=CARTESIAN_POINT('Ctrl Pts',(3.75962280650875,-1.,-1.39030069388926));
#56615=CARTESIAN_POINT('Ctrl Pts',(3.75962280650875,1.,-1.39030069388926));
#56616=CARTESIAN_POINT('Ctrl Pts',(3.76540689249078,-1.,-1.39528769118054));
#56617=CARTESIAN_POINT('Ctrl Pts',(3.76540689249078,1.,-1.39528769118054));
#56618=CARTESIAN_POINT('Ctrl Pts',(3.77116930621804,-1.,-1.40031121335495));
#56619=CARTESIAN_POINT('Ctrl Pts',(3.77116930621804,1.,-1.40031121335495));
#56620=CARTESIAN_POINT('Ctrl Pts',(3.77690952014209,-1.,-1.40537056004702));
#56621=CARTESIAN_POINT('Ctrl Pts',(3.77690952014209,1.,-1.40537056004702));
#56622=CARTESIAN_POINT('Ctrl Pts',(3.78262780065406,-1.,-1.41046532282567));
#56623=CARTESIAN_POINT('Ctrl Pts',(3.78262780065406,1.,-1.41046532282567));
#56624=CARTESIAN_POINT('Ctrl Pts',(3.78832489879369,-1.,-1.41559527803808));
#56625=CARTESIAN_POINT('Ctrl Pts',(3.78832489879369,1.,-1.41559527803808));
#56626=CARTESIAN_POINT('Ctrl Pts',(3.7940017574439,-1.,-1.42076028482828));
#56627=CARTESIAN_POINT('Ctrl Pts',(3.7940017574439,1.,-1.42076028482828));
#56628=CARTESIAN_POINT('Ctrl Pts',(3.79965923196365,-1.,-1.42596018777301));
#56629=CARTESIAN_POINT('Ctrl Pts',(3.79965923196365,1.,-1.42596018777301));
#56630=CARTESIAN_POINT('Ctrl Pts',(3.80529775429916,-1.,-1.43119469921364));
#56631=CARTESIAN_POINT('Ctrl Pts',(3.80529775429916,1.,-1.43119469921364));
#56632=CARTESIAN_POINT('Ctrl Pts',(3.81091737726965,-1.,-1.43646341556783));
#56633=CARTESIAN_POINT('Ctrl Pts',(3.81091737726965,1.,-1.43646341556783));
#56634=CARTESIAN_POINT('Ctrl Pts',(3.8165179239855,-1.,-1.44176587041401));
#56635=CARTESIAN_POINT('Ctrl Pts',(3.8165179239855,1.,-1.44176587041401));
#56636=CARTESIAN_POINT('Ctrl Pts',(3.82209910620591,-1.,-1.44710157648562));
#56637=CARTESIAN_POINT('Ctrl Pts',(3.82209910620591,1.,-1.44710157648562));
#56638=CARTESIAN_POINT('Ctrl Pts',(3.82766064519,-1.,-1.45247006796807));
#56639=CARTESIAN_POINT('Ctrl Pts',(3.82766064519,1.,-1.45247006796807));
#56640=CARTESIAN_POINT('Ctrl Pts',(3.83320241775199,-1.,-1.45787095220763));
#56641=CARTESIAN_POINT('Ctrl Pts',(3.83320241775199,1.,-1.45787095220763));
#56642=CARTESIAN_POINT('Ctrl Pts',(3.83872447159309,-1.,-1.46330391180621));
#56643=CARTESIAN_POINT('Ctrl Pts',(3.83872447159309,1.,-1.46330391180621));
#56644=CARTESIAN_POINT('Ctrl Pts',(3.84422695454469,-1.,-1.46876867426375));
#56645=CARTESIAN_POINT('Ctrl Pts',(3.84422695454469,1.,-1.46876867426375));
#56646=CARTESIAN_POINT('Ctrl Pts',(3.84971006847096,-1.,-1.47426499018467));
#56647=CARTESIAN_POINT('Ctrl Pts',(3.84971006847096,1.,-1.47426499018467));
#56648=CARTESIAN_POINT('Ctrl Pts',(3.85517401698952,-1.,-1.47979260991063));
#56649=CARTESIAN_POINT('Ctrl Pts',(3.85517401698952,1.,-1.47979260991063));
#56650=CARTESIAN_POINT('Ctrl Pts',(3.86061894706551,-1.,-1.48535125510102));
#56651=CARTESIAN_POINT('Ctrl Pts',(3.86061894706551,1.,-1.48535125510102));
#56652=CARTESIAN_POINT('Ctrl Pts',(3.86604492575933,-1.,-1.49094061164604));
#56653=CARTESIAN_POINT('Ctrl Pts',(3.86604492575933,1.,-1.49094061164604));
#56654=CARTESIAN_POINT('Ctrl Pts',(3.8714519699927,-1.,-1.4965603539944));
#56655=CARTESIAN_POINT('Ctrl Pts',(3.8714519699927,1.,-1.4965603539944));
#56656=CARTESIAN_POINT('Ctrl Pts',(3.87684006372665,-1.,-1.50221016176766));
#56657=CARTESIAN_POINT('Ctrl Pts',(3.87684006372665,1.,-1.50221016176766));
#56658=CARTESIAN_POINT('Ctrl Pts',(3.88220917950443,-1.,-1.50788973857719));
#56659=CARTESIAN_POINT('Ctrl Pts',(3.88220917950443,1.,-1.50788973857719));
#56660=CARTESIAN_POINT('Ctrl Pts',(3.88755930032927,-1.,-1.51359883110181));
#56661=CARTESIAN_POINT('Ctrl Pts',(3.88755930032927,1.,-1.51359883110181));
#56662=CARTESIAN_POINT('Ctrl Pts',(3.89289043531893,-1.,-1.51933724328609));
#56663=CARTESIAN_POINT('Ctrl Pts',(3.89289043531893,1.,-1.51933724328609));
#56664=CARTESIAN_POINT('Ctrl Pts',(3.8982026070607,-1.,-1.52510482990784));
#56665=CARTESIAN_POINT('Ctrl Pts',(3.8982026070607,1.,-1.52510482990784));
#56666=CARTESIAN_POINT('Ctrl Pts',(3.90243719629755,-1.,-1.5297421605556));
#56667=CARTESIAN_POINT('Ctrl Pts',(3.90243719629755,1.,-1.5297421605556));
#56668=CARTESIAN_POINT('Ctrl Pts',(3.90560462812846,-1.,-1.53323321827311));
#56669=CARTESIAN_POINT('Ctrl Pts',(3.90560462812846,1.,-1.53323321827311));
#56670=CARTESIAN_POINT('Ctrl Pts',(3.90771246854607,-1.,-1.53556639217742));
#56671=CARTESIAN_POINT('Ctrl Pts',(3.90771246854607,1.,-1.53556639217742));
#56672=CARTESIAN_POINT('Ctrl Pts',(3.90876544355381,-1.,-1.53673442965256));
#56673=CARTESIAN_POINT('Ctrl Pts',(3.90876544355381,1.,-1.53673442965256));
#56674=CARTESIAN_POINT('',(3.5372048861591,1.,-1.24526366418208));
#56675=CARTESIAN_POINT('Ctrl Pts',(3.5372048861591,-1.,-1.24526366418208));
#56676=CARTESIAN_POINT('Ctrl Pts',(3.5372048861591,-0.666666666666667,-1.24526366418208));
#56677=CARTESIAN_POINT('Ctrl Pts',(3.5372048861591,-0.333333333333333,-1.24526366418208));
#56678=CARTESIAN_POINT('Ctrl Pts',(3.5372048861591,0.333333333333333,-1.24526366418208));
#56679=CARTESIAN_POINT('Ctrl Pts',(3.5372048861591,0.666666666666667,-1.24526366418208));
#56680=CARTESIAN_POINT('Ctrl Pts',(3.5372048861591,1.,-1.24526366418208));
#56681=CARTESIAN_POINT('',(3.90876544355381,1.,-1.53673442965256));
#56682=CARTESIAN_POINT('',(3.90876544355381,0.,-1.53673442965256));
#56683=CARTESIAN_POINT('Ctrl Pts',(3.5372048861591,1.,-1.24526366418208));
#56684=CARTESIAN_POINT('Ctrl Pts',(3.53725139174402,1.,-1.24524838931864));
#56685=CARTESIAN_POINT('Ctrl Pts',(3.53744859265385,1.,-1.24524498991133));
#56686=CARTESIAN_POINT('Ctrl Pts',(3.53808746578052,1.,-1.2453920538873));
#56687=CARTESIAN_POINT('Ctrl Pts',(3.53968291129942,1.,-1.24593497225964));
#56688=CARTESIAN_POINT('Ctrl Pts',(3.54294877426113,1.,-1.2472164623202));
#56689=CARTESIAN_POINT('Ctrl Pts',(3.54784190282889,1.,-1.24926408627938));
#56690=CARTESIAN_POINT('Ctrl Pts',(3.5538728741862,1.,-1.25188792940508));
#56691=CARTESIAN_POINT('Ctrl Pts',(3.56071094990825,1.,-1.25496090899873));
#56692=CARTESIAN_POINT('Ctrl Pts',(3.56798645995025,1.,-1.25834000485626));
#56693=CARTESIAN_POINT('Ctrl Pts',(3.5753456065164,1.,-1.26188667142784));
#56694=CARTESIAN_POINT('Ctrl Pts',(3.58250452868699,1.,-1.26548706249891));
#56695=CARTESIAN_POINT('Ctrl Pts',(3.5893180784647,1.,-1.26907758484766));
#56696=CARTESIAN_POINT('Ctrl Pts',(3.59578698050164,1.,-1.27264798379365));
#56697=CARTESIAN_POINT('Ctrl Pts',(3.60199947736404,1.,-1.27622049908664));
#56698=CARTESIAN_POINT('Ctrl Pts',(3.60808907746372,1.,-1.27983492861703));
#56699=CARTESIAN_POINT('Ctrl Pts',(3.61418935913793,1.,-1.28353255117754));
#56700=CARTESIAN_POINT('Ctrl Pts',(3.62038148492295,1.,-1.2873375502936));
#56701=CARTESIAN_POINT('Ctrl Pts',(3.62667616004299,1.,-1.29125046021853));
#56702=CARTESIAN_POINT('Ctrl Pts',(3.63304271630995,1.,-1.29525810207744));
#56703=CARTESIAN_POINT('Ctrl Pts',(3.6394268987279,1.,-1.29933955906463));
#56704=CARTESIAN_POINT('Ctrl Pts',(3.64577181380125,1.,-1.30347327603778));
#56705=CARTESIAN_POINT('Ctrl Pts',(3.65204081987101,1.,-1.30764479590051));
#56706=CARTESIAN_POINT('Ctrl Pts',(3.65822827358655,1.,-1.31185038411231));
#56707=CARTESIAN_POINT('Ctrl Pts',(3.66434688899822,1.,-1.31609271239922));
#56708=CARTESIAN_POINT('Ctrl Pts',(3.67042021752668,1.,-1.3203782813777));
#56709=CARTESIAN_POINT('Ctrl Pts',(3.67647355257906,1.,-1.32471430856413));
#56710=CARTESIAN_POINT('Ctrl Pts',(3.68252441182534,1.,-1.32910547072734));
#56711=CARTESIAN_POINT('Ctrl Pts',(3.68857672413013,1.,-1.33355191034515));
#56712=CARTESIAN_POINT('Ctrl Pts',(3.69462613305692,1.,-1.33805103398214));
#56713=CARTESIAN_POINT('Ctrl Pts',(3.70066324015112,1.,-1.3425986075293));
#56714=CARTESIAN_POINT('Ctrl Pts',(3.7066775318825,1.,-1.34719008463535));
#56715=CARTESIAN_POINT('Ctrl Pts',(3.71266130563061,1.,-1.35182193384426));
#56716=CARTESIAN_POINT('Ctrl Pts',(3.71861271513318,1.,-1.35649266705038));
#56717=CARTESIAN_POINT('Ctrl Pts',(3.72453364678279,1.,-1.36120211416354));
#56718=CARTESIAN_POINT('Ctrl Pts',(3.73042829011293,1.,-1.36595093298674));
#56719=CARTESIAN_POINT('Ctrl Pts',(3.73630145885809,1.,-1.37074003422739));
#56720=CARTESIAN_POINT('Ctrl Pts',(3.7421569816256,1.,-1.3755700297169));
#56721=CARTESIAN_POINT('Ctrl Pts',(3.74799617204744,1.,-1.38044070763302));
#56722=CARTESIAN_POINT('Ctrl Pts',(3.75381861212728,1.,-1.38535129801185));
#56723=CARTESIAN_POINT('Ctrl Pts',(3.75962280650875,1.,-1.39030069388926));
#56724=CARTESIAN_POINT('Ctrl Pts',(3.76540689249078,1.,-1.39528769118054));
#56725=CARTESIAN_POINT('Ctrl Pts',(3.77116930621804,1.,-1.40031121335495));
#56726=CARTESIAN_POINT('Ctrl Pts',(3.77690952014209,1.,-1.40537056004702));
#56727=CARTESIAN_POINT('Ctrl Pts',(3.78262780065406,1.,-1.41046532282567));
#56728=CARTESIAN_POINT('Ctrl Pts',(3.78832489879369,1.,-1.41559527803808));
#56729=CARTESIAN_POINT('Ctrl Pts',(3.7940017574439,1.,-1.42076028482828));
#56730=CARTESIAN_POINT('Ctrl Pts',(3.79965923196365,1.,-1.42596018777301));
#56731=CARTESIAN_POINT('Ctrl Pts',(3.80529775429916,1.,-1.43119469921364));
#56732=CARTESIAN_POINT('Ctrl Pts',(3.81091737726965,1.,-1.43646341556783));
#56733=CARTESIAN_POINT('Ctrl Pts',(3.8165179239855,1.,-1.44176587041401));
#56734=CARTESIAN_POINT('Ctrl Pts',(3.82209910620591,1.,-1.44710157648562));
#56735=CARTESIAN_POINT('Ctrl Pts',(3.82766064519,1.,-1.45247006796807));
#56736=CARTESIAN_POINT('Ctrl Pts',(3.83320241775199,1.,-1.45787095220763));
#56737=CARTESIAN_POINT('Ctrl Pts',(3.83872447159309,1.,-1.46330391180621));
#56738=CARTESIAN_POINT('Ctrl Pts',(3.84422695454469,1.,-1.46876867426375));
#56739=CARTESIAN_POINT('Ctrl Pts',(3.84971006847096,1.,-1.47426499018467));
#56740=CARTESIAN_POINT('Ctrl Pts',(3.85517401698952,1.,-1.47979260991063));
#56741=CARTESIAN_POINT('Ctrl Pts',(3.86061894706551,1.,-1.48535125510102));
#56742=CARTESIAN_POINT('Ctrl Pts',(3.86604492575933,1.,-1.49094061164604));
#56743=CARTESIAN_POINT('Ctrl Pts',(3.8714519699927,1.,-1.4965603539944));
#56744=CARTESIAN_POINT('Ctrl Pts',(3.87684006372665,1.,-1.50221016176766));
#56745=CARTESIAN_POINT('Ctrl Pts',(3.88220917950443,1.,-1.50788973857719));
#56746=CARTESIAN_POINT('Ctrl Pts',(3.88755930032927,1.,-1.51359883110181));
#56747=CARTESIAN_POINT('Ctrl Pts',(3.89289043531893,1.,-1.51933724328609));
#56748=CARTESIAN_POINT('Ctrl Pts',(3.8982026070607,1.,-1.52510482990784));
#56749=CARTESIAN_POINT('Ctrl Pts',(3.90243719629755,1.,-1.5297421605556));
#56750=CARTESIAN_POINT('Ctrl Pts',(3.90560462812846,1.,-1.53323321827311));
#56751=CARTESIAN_POINT('Ctrl Pts',(3.90771246854607,1.,-1.53556639217742));
#56752=CARTESIAN_POINT('Ctrl Pts',(3.90876544355381,1.,-1.53673442965256));
#56753=CARTESIAN_POINT('Origin',(3.90876544355381,0.,-1.53673442965256));
#56754=CARTESIAN_POINT('',(3.85054988729471,1.,-1.67727921511438));
#56755=CARTESIAN_POINT('Origin',(0.,0.,0.));
#56756=CARTESIAN_POINT('',(3.59360648251021,1.,-1.071677399622));
#56757=CARTESIAN_POINT('Origin',(0.,1.,0.));
#56758=CARTESIAN_POINT('Ctrl Pts',(3.59360648251021,1.,-1.071677399622));
#56759=CARTESIAN_POINT('Ctrl Pts',(3.59360648251021,0.666666666666667,-1.071677399622));
#56760=CARTESIAN_POINT('Ctrl Pts',(3.59360648251021,0.333333333333333,-1.071677399622));
#56761=CARTESIAN_POINT('Ctrl Pts',(3.59360648251021,-0.333333333333333,
-1.071677399622));
#56762=CARTESIAN_POINT('Ctrl Pts',(3.59360648251021,-0.666666666666667,
-1.071677399622));
#56763=CARTESIAN_POINT('Ctrl Pts',(3.59360648251021,-1.,-1.071677399622));
#56764=CARTESIAN_POINT('Ctrl Pts',(4.06552750530042,-1.,-1.05427041296137));
#56765=CARTESIAN_POINT('Ctrl Pts',(4.06552750530042,1.,-1.05427041296137));
#56766=CARTESIAN_POINT('Ctrl Pts',(4.06398907542679,-1.,-1.05459645194934));
#56767=CARTESIAN_POINT('Ctrl Pts',(4.06398907542679,1.,-1.05459645194934));
#56768=CARTESIAN_POINT('Ctrl Pts',(4.06091239150293,-1.,-1.05524507177901));
#56769=CARTESIAN_POINT('Ctrl Pts',(4.06091239150293,1.,-1.05524507177901));
#56770=CARTESIAN_POINT('Ctrl Pts',(4.05629789308941,-1.,-1.0562076270849));
#56771=CARTESIAN_POINT('Ctrl Pts',(4.05629789308941,1.,-1.0562076270849));
#56772=CARTESIAN_POINT('Ctrl Pts',(4.05014628387112,-1.,-1.05747027728537));
#56773=CARTESIAN_POINT('Ctrl Pts',(4.05014628387112,1.,-1.05747027728537));
#56774=CARTESIAN_POINT('Ctrl Pts',(4.04245854429333,-1.,-1.0590139366704));
#56775=CARTESIAN_POINT('Ctrl Pts',(4.04245854429333,1.,-1.0590139366704));
#56776=CARTESIAN_POINT('Ctrl Pts',(4.03477261142549,-1.,-1.06052284712114));
#56777=CARTESIAN_POINT('Ctrl Pts',(4.03477261142549,1.,-1.06052284712114));
#56778=CARTESIAN_POINT('Ctrl Pts',(4.02708855235732,-1.,-1.06199687787488));
#56779=CARTESIAN_POINT('Ctrl Pts',(4.02708855235732,1.,-1.06199687787488));
#56780=CARTESIAN_POINT('Ctrl Pts',(4.0194064749539,-1.,-1.06343586496094));
#56781=CARTESIAN_POINT('Ctrl Pts',(4.0194064749539,1.,-1.06343586496094));
#56782=CARTESIAN_POINT('Ctrl Pts',(4.0117265418656,-1.,-1.06483961342894));
#56783=CARTESIAN_POINT('Ctrl Pts',(4.0117265418656,1.,-1.06483961342894));
#56784=CARTESIAN_POINT('Ctrl Pts',(4.00404894951804,-1.,-1.06620789963406));
#56785=CARTESIAN_POINT('Ctrl Pts',(4.00404894951804,1.,-1.06620789963406));
#56786=CARTESIAN_POINT('Ctrl Pts',(3.99637389919958,-1.,-1.06754047381188));
#56787=CARTESIAN_POINT('Ctrl Pts',(3.99637389919958,1.,-1.06754047381188));
#56788=CARTESIAN_POINT('Ctrl Pts',(3.98870156857298,-1.,-1.06883706263912));
#56789=CARTESIAN_POINT('Ctrl Pts',(3.98870156857298,1.,-1.06883706263912));
#56790=CARTESIAN_POINT('Ctrl Pts',(3.98103208801289,-1.,-1.07009737257815));
#56791=CARTESIAN_POINT('Ctrl Pts',(3.98103208801289,1.,-1.07009737257815));
#56792=CARTESIAN_POINT('Ctrl Pts',(3.97336550222571,-1.,-1.07132109206252));
#56793=CARTESIAN_POINT('Ctrl Pts',(3.97336550222571,1.,-1.07132109206252));
#56794=CARTESIAN_POINT('Ctrl Pts',(3.96570179322681,-1.,-1.07250789943095));
#56795=CARTESIAN_POINT('Ctrl Pts',(3.96570179322681,1.,-1.07250789943095));
#56796=CARTESIAN_POINT('Ctrl Pts',(3.95804094429606,-1.,-1.07365747426551));
#56797=CARTESIAN_POINT('Ctrl Pts',(3.95804094429606,1.,-1.07365747426551));
#56798=CARTESIAN_POINT('Ctrl Pts',(3.95038299600754,-1.,-1.07476950921607));
#56799=CARTESIAN_POINT('Ctrl Pts',(3.95038299600754,1.,-1.07476950921607));
#56800=CARTESIAN_POINT('Ctrl Pts',(3.94272809633271,-1.,-1.07584371946428));
#56801=CARTESIAN_POINT('Ctrl Pts',(3.94272809633271,1.,-1.07584371946428));
#56802=CARTESIAN_POINT('Ctrl Pts',(3.93507657572743,-1.,-1.07687985975348));
#56803=CARTESIAN_POINT('Ctrl Pts',(3.93507657572743,1.,-1.07687985975348));
#56804=CARTESIAN_POINT('Ctrl Pts',(3.92742893349684,-1.,-1.07787771707155));
#56805=CARTESIAN_POINT('Ctrl Pts',(3.92742893349684,1.,-1.07787771707155));
#56806=CARTESIAN_POINT('Ctrl Pts',(3.91978568924062,-1.,-1.07883706663524));
#56807=CARTESIAN_POINT('Ctrl Pts',(3.91978568924062,1.,-1.07883706663524));
#56808=CARTESIAN_POINT('Ctrl Pts',(3.91214726022096,-1.,-1.0797576350746));
#56809=CARTESIAN_POINT('Ctrl Pts',(3.91214726022096,1.,-1.0797576350746));
#56810=CARTESIAN_POINT('Ctrl Pts',(3.90451384092564,-1.,-1.08063906483823));
#56811=CARTESIAN_POINT('Ctrl Pts',(3.90451384092564,1.,-1.08063906483823));
#56812=CARTESIAN_POINT('Ctrl Pts',(3.89688525098408,-1.,-1.08148086931373));
#56813=CARTESIAN_POINT('Ctrl Pts',(3.89688525098408,1.,-1.08148086931373));
#56814=CARTESIAN_POINT('Ctrl Pts',(3.88926088975182,-1.,-1.08228241999363));
#56815=CARTESIAN_POINT('Ctrl Pts',(3.88926088975182,1.,-1.08228241999363));
#56816=CARTESIAN_POINT('Ctrl Pts',(3.88164007721365,-1.,-1.08304304871042));
#56817=CARTESIAN_POINT('Ctrl Pts',(3.88164007721365,1.,-1.08304304871042));
#56818=CARTESIAN_POINT('Ctrl Pts',(3.87402233722563,-1.,-1.0837621330751));
#56819=CARTESIAN_POINT('Ctrl Pts',(3.87402233722563,1.,-1.0837621330751));
#56820=CARTESIAN_POINT('Ctrl Pts',(3.86640769434269,-1.,-1.08443918607926));
#56821=CARTESIAN_POINT('Ctrl Pts',(3.86640769434269,1.,-1.08443918607926));
#56822=CARTESIAN_POINT('Ctrl Pts',(3.85879698702511,-1.,-1.08507395120054));
#56823=CARTESIAN_POINT('Ctrl Pts',(3.85879698702511,1.,-1.08507395120054));
#56824=CARTESIAN_POINT('Ctrl Pts',(3.85119211322732,-1.,-1.08566647671838));
#56825=CARTESIAN_POINT('Ctrl Pts',(3.85119211322732,1.,-1.08566647671838));
#56826=CARTESIAN_POINT('Ctrl Pts',(3.84359528764934,-1.,-1.08621688337601));
#56827=CARTESIAN_POINT('Ctrl Pts',(3.84359528764934,1.,-1.08621688337601));
#56828=CARTESIAN_POINT('Ctrl Pts',(3.83600837071702,-1.,-1.08672515456901));
#56829=CARTESIAN_POINT('Ctrl Pts',(3.83600837071702,1.,-1.08672515456901));
#56830=CARTESIAN_POINT('Ctrl Pts',(3.82843215316985,-1.,-1.08719091307558));
#56831=CARTESIAN_POINT('Ctrl Pts',(3.82843215316985,1.,-1.08719091307558));
#56832=CARTESIAN_POINT('Ctrl Pts',(3.82086569676321,-1.,-1.08761321539442));
#56833=CARTESIAN_POINT('Ctrl Pts',(3.82086569676321,1.,-1.08761321539442));
#56834=CARTESIAN_POINT('Ctrl Pts',(3.81330554446324,-1.,-1.08799030610861));
#56835=CARTESIAN_POINT('Ctrl Pts',(3.81330554446324,1.,-1.08799030610861));
#56836=CARTESIAN_POINT('Ctrl Pts',(3.80574726657656,-1.,-1.08832009255378));
#56837=CARTESIAN_POINT('Ctrl Pts',(3.80574726657656,1.,-1.08832009255378));
#56838=CARTESIAN_POINT('Ctrl Pts',(3.79818708705252,-1.,-1.08860064435776));
#56839=CARTESIAN_POINT('Ctrl Pts',(3.79818708705252,1.,-1.08860064435776));
#56840=CARTESIAN_POINT('Ctrl Pts',(3.79062357974401,-1.,-1.08883071512097));
#56841=CARTESIAN_POINT('Ctrl Pts',(3.79062357974401,1.,-1.08883071512097));
#56842=CARTESIAN_POINT('Ctrl Pts',(3.78305911299511,-1.,-1.08901018614638));
#56843=CARTESIAN_POINT('Ctrl Pts',(3.78305911299511,1.,-1.08901018614638));
#56844=CARTESIAN_POINT('Ctrl Pts',(3.7755019940944,-1.,-1.08914072791275));
#56845=CARTESIAN_POINT('Ctrl Pts',(3.7755019940944,1.,-1.08914072791275));
#56846=CARTESIAN_POINT('Ctrl Pts',(3.76796340094469,-1.,-1.08922484204263));
#56847=CARTESIAN_POINT('Ctrl Pts',(3.76796340094469,1.,-1.08922484204263));
#56848=CARTESIAN_POINT('Ctrl Pts',(3.76045342580226,-1.,-1.08926462734287));
#56849=CARTESIAN_POINT('Ctrl Pts',(3.76045342580226,1.,-1.08926462734287));
#56850=CARTESIAN_POINT('Ctrl Pts',(3.75297711748138,-1.,-1.08926054632927));
#56851=CARTESIAN_POINT('Ctrl Pts',(3.75297711748138,1.,-1.08926054632927));
#56852=CARTESIAN_POINT('Ctrl Pts',(3.74553121371745,-1.,-1.08921040494013));
#56853=CARTESIAN_POINT('Ctrl Pts',(3.74553121371745,1.,-1.08921040494013));
#56854=CARTESIAN_POINT('Ctrl Pts',(3.73809879348209,-1.,-1.08910769013288));
#56855=CARTESIAN_POINT('Ctrl Pts',(3.73809879348209,1.,-1.08910769013288));
#56856=CARTESIAN_POINT('Ctrl Pts',(3.73065515162949,-1.,-1.08894337390925));
#56857=CARTESIAN_POINT('Ctrl Pts',(3.73065515162949,1.,-1.08894337390925));
#56858=CARTESIAN_POINT('Ctrl Pts',(3.72317741369364,-1.,-1.08870887220072));
#56859=CARTESIAN_POINT('Ctrl Pts',(3.72317741369364,1.,-1.08870887220072));
#56860=CARTESIAN_POINT('Ctrl Pts',(3.71565372339063,-1.,-1.08839887334777));
#56861=CARTESIAN_POINT('Ctrl Pts',(3.71565372339063,1.,-1.08839887334777));
#56862=CARTESIAN_POINT('Ctrl Pts',(3.70809084139476,-1.,-1.0880136731219));
#56863=CARTESIAN_POINT('Ctrl Pts',(3.70809084139476,1.,-1.0880136731219));
#56864=CARTESIAN_POINT('Ctrl Pts',(3.70052690909884,-1.,-1.08756311291324));
#56865=CARTESIAN_POINT('Ctrl Pts',(3.70052690909884,1.,-1.08756311291324));
#56866=CARTESIAN_POINT('Ctrl Pts',(3.69302062410229,-1.,-1.08706319540292));
#56867=CARTESIAN_POINT('Ctrl Pts',(3.69302062410229,1.,-1.08706319540292));
#56868=CARTESIAN_POINT('Ctrl Pts',(3.68562817420864,-1.,-1.08652888882609));
#56869=CARTESIAN_POINT('Ctrl Pts',(3.68562817420864,1.,-1.08652888882609));
#56870=CARTESIAN_POINT('Ctrl Pts',(3.67838211685148,-1.,-1.08596755755768));
#56871=CARTESIAN_POINT('Ctrl Pts',(3.67838211685148,1.,-1.08596755755768));
#56872=CARTESIAN_POINT('Ctrl Pts',(3.67127347729632,-1.,-1.0853733414448));
#56873=CARTESIAN_POINT('Ctrl Pts',(3.67127347729632,1.,-1.0853733414448));
#56874=CARTESIAN_POINT('Ctrl Pts',(3.66422237895256,-1.,-1.0847180992287));
#56875=CARTESIAN_POINT('Ctrl Pts',(3.66422237895256,1.,-1.0847180992287));
#56876=CARTESIAN_POINT('Ctrl Pts',(3.65709649161004,-1.,-1.08395671077761));
#56877=CARTESIAN_POINT('Ctrl Pts',(3.65709649161004,1.,-1.08395671077761));
#56878=CARTESIAN_POINT('Ctrl Pts',(3.64976441208197,-1.,-1.08304289898577));
#56879=CARTESIAN_POINT('Ctrl Pts',(3.64976441208197,1.,-1.08304289898577));
#56880=CARTESIAN_POINT('Ctrl Pts',(3.64214167843595,-1.,-1.08194278850972));
#56881=CARTESIAN_POINT('Ctrl Pts',(3.64214167843595,1.,-1.08194278850972));
#56882=CARTESIAN_POINT('Ctrl Pts',(3.63423373196602,-1.,-1.08064765719887));
#56883=CARTESIAN_POINT('Ctrl Pts',(3.63423373196602,1.,-1.08064765719887));
#56884=CARTESIAN_POINT('Ctrl Pts',(3.62619537902616,-1.,-1.07919137290816));
#56885=CARTESIAN_POINT('Ctrl Pts',(3.62619537902616,1.,-1.07919137290816));
#56886=CARTESIAN_POINT('Ctrl Pts',(3.61832318504957,-1.,-1.07764868137729));
#56887=CARTESIAN_POINT('Ctrl Pts',(3.61832318504957,1.,-1.07764868137729));
#56888=CARTESIAN_POINT('Ctrl Pts',(3.61098481349577,-1.,-1.07611545402841));
#56889=CARTESIAN_POINT('Ctrl Pts',(3.61098481349577,1.,-1.07611545402841));
#56890=CARTESIAN_POINT('Ctrl Pts',(3.6045633988796,-1.,-1.0746932716863));
#56891=CARTESIAN_POINT('Ctrl Pts',(3.6045633988796,1.,-1.0746932716863));
#56892=CARTESIAN_POINT('Ctrl Pts',(3.59940121154383,-1.,-1.0734737254567));
#56893=CARTESIAN_POINT('Ctrl Pts',(3.59940121154383,1.,-1.0734737254567));
#56894=CARTESIAN_POINT('Ctrl Pts',(3.59573039611837,-1.,-1.07251922679108));
#56895=CARTESIAN_POINT('Ctrl Pts',(3.59573039611837,1.,-1.07251922679108));
#56896=CARTESIAN_POINT('Ctrl Pts',(3.59407399103556,-1.,-1.07199116987503));
#56897=CARTESIAN_POINT('Ctrl Pts',(3.59407399103556,1.,-1.07199116987503));
#56898=CARTESIAN_POINT('Ctrl Pts',(3.59356848057451,-1.,-1.07173216219041));
#56899=CARTESIAN_POINT('Ctrl Pts',(3.59356848057451,1.,-1.07173216219041));
#56900=CARTESIAN_POINT('Ctrl Pts',(3.59355870577763,-1.,-1.07162034256419));
#56901=CARTESIAN_POINT('Ctrl Pts',(3.59355870577763,1.,-1.07162034256419));
#56902=CARTESIAN_POINT('Ctrl Pts',(3.59363563249864,-1.,-1.07157964745328));
#56903=CARTESIAN_POINT('Ctrl Pts',(3.59363563249864,1.,-1.07157964745328));
#56904=CARTESIAN_POINT('',(4.06552750530042,1.,-1.05427041296137));
#56905=CARTESIAN_POINT('Ctrl Pts',(4.06552750530042,1.,-1.05427041296137));
#56906=CARTESIAN_POINT('Ctrl Pts',(4.06398907542679,1.,-1.05459645194934));
#56907=CARTESIAN_POINT('Ctrl Pts',(4.06091239150293,1.,-1.05524507177901));
#56908=CARTESIAN_POINT('Ctrl Pts',(4.05629789308941,1.,-1.0562076270849));
#56909=CARTESIAN_POINT('Ctrl Pts',(4.05014628387112,1.,-1.05747027728537));
#56910=CARTESIAN_POINT('Ctrl Pts',(4.04245854429333,1.,-1.0590139366704));
#56911=CARTESIAN_POINT('Ctrl Pts',(4.03477261142549,1.,-1.06052284712114));
#56912=CARTESIAN_POINT('Ctrl Pts',(4.02708855235732,1.,-1.06199687787488));
#56913=CARTESIAN_POINT('Ctrl Pts',(4.0194064749539,1.,-1.06343586496094));
#56914=CARTESIAN_POINT('Ctrl Pts',(4.0117265418656,1.,-1.06483961342894));
#56915=CARTESIAN_POINT('Ctrl Pts',(4.00404894951804,1.,-1.06620789963406));
#56916=CARTESIAN_POINT('Ctrl Pts',(3.99637389919958,1.,-1.06754047381188));
#56917=CARTESIAN_POINT('Ctrl Pts',(3.98870156857298,1.,-1.06883706263912));
#56918=CARTESIAN_POINT('Ctrl Pts',(3.98103208801289,1.,-1.07009737257815));
#56919=CARTESIAN_POINT('Ctrl Pts',(3.97336550222571,1.,-1.07132109206252));
#56920=CARTESIAN_POINT('Ctrl Pts',(3.96570179322681,1.,-1.07250789943095));
#56921=CARTESIAN_POINT('Ctrl Pts',(3.95804094429606,1.,-1.07365747426551));
#56922=CARTESIAN_POINT('Ctrl Pts',(3.95038299600754,1.,-1.07476950921607));
#56923=CARTESIAN_POINT('Ctrl Pts',(3.94272809633271,1.,-1.07584371946428));
#56924=CARTESIAN_POINT('Ctrl Pts',(3.93507657572743,1.,-1.07687985975348));
#56925=CARTESIAN_POINT('Ctrl Pts',(3.92742893349684,1.,-1.07787771707155));
#56926=CARTESIAN_POINT('Ctrl Pts',(3.91978568924062,1.,-1.07883706663524));
#56927=CARTESIAN_POINT('Ctrl Pts',(3.91214726022096,1.,-1.0797576350746));
#56928=CARTESIAN_POINT('Ctrl Pts',(3.90451384092564,1.,-1.08063906483823));
#56929=CARTESIAN_POINT('Ctrl Pts',(3.89688525098408,1.,-1.08148086931373));
#56930=CARTESIAN_POINT('Ctrl Pts',(3.88926088975182,1.,-1.08228241999363));
#56931=CARTESIAN_POINT('Ctrl Pts',(3.88164007721365,1.,-1.08304304871042));
#56932=CARTESIAN_POINT('Ctrl Pts',(3.87402233722563,1.,-1.0837621330751));
#56933=CARTESIAN_POINT('Ctrl Pts',(3.86640769434269,1.,-1.08443918607926));
#56934=CARTESIAN_POINT('Ctrl Pts',(3.85879698702511,1.,-1.08507395120054));
#56935=CARTESIAN_POINT('Ctrl Pts',(3.85119211322732,1.,-1.08566647671838));
#56936=CARTESIAN_POINT('Ctrl Pts',(3.84359528764934,1.,-1.08621688337601));
#56937=CARTESIAN_POINT('Ctrl Pts',(3.83600837071702,1.,-1.08672515456901));
#56938=CARTESIAN_POINT('Ctrl Pts',(3.82843215316985,1.,-1.08719091307558));
#56939=CARTESIAN_POINT('Ctrl Pts',(3.82086569676321,1.,-1.08761321539442));
#56940=CARTESIAN_POINT('Ctrl Pts',(3.81330554446324,1.,-1.08799030610861));
#56941=CARTESIAN_POINT('Ctrl Pts',(3.80574726657656,1.,-1.08832009255378));
#56942=CARTESIAN_POINT('Ctrl Pts',(3.79818708705252,1.,-1.08860064435776));
#56943=CARTESIAN_POINT('Ctrl Pts',(3.79062357974401,1.,-1.08883071512097));
#56944=CARTESIAN_POINT('Ctrl Pts',(3.78305911299511,1.,-1.08901018614638));
#56945=CARTESIAN_POINT('Ctrl Pts',(3.7755019940944,1.,-1.08914072791275));
#56946=CARTESIAN_POINT('Ctrl Pts',(3.76796340094469,1.,-1.08922484204263));
#56947=CARTESIAN_POINT('Ctrl Pts',(3.76045342580226,1.,-1.08926462734287));
#56948=CARTESIAN_POINT('Ctrl Pts',(3.75297711748138,1.,-1.08926054632927));
#56949=CARTESIAN_POINT('Ctrl Pts',(3.74553121371745,1.,-1.08921040494013));
#56950=CARTESIAN_POINT('Ctrl Pts',(3.73809879348209,1.,-1.08910769013288));
#56951=CARTESIAN_POINT('Ctrl Pts',(3.73065515162949,1.,-1.08894337390925));
#56952=CARTESIAN_POINT('Ctrl Pts',(3.72317741369364,1.,-1.08870887220072));
#56953=CARTESIAN_POINT('Ctrl Pts',(3.71565372339063,1.,-1.08839887334777));
#56954=CARTESIAN_POINT('Ctrl Pts',(3.70809084139476,1.,-1.0880136731219));
#56955=CARTESIAN_POINT('Ctrl Pts',(3.70052690909884,1.,-1.08756311291324));
#56956=CARTESIAN_POINT('Ctrl Pts',(3.69302062410229,1.,-1.08706319540292));
#56957=CARTESIAN_POINT('Ctrl Pts',(3.68562817420864,1.,-1.08652888882609));
#56958=CARTESIAN_POINT('Ctrl Pts',(3.67838211685148,1.,-1.08596755755768));
#56959=CARTESIAN_POINT('Ctrl Pts',(3.67127347729632,1.,-1.0853733414448));
#56960=CARTESIAN_POINT('Ctrl Pts',(3.66422237895256,1.,-1.0847180992287));
#56961=CARTESIAN_POINT('Ctrl Pts',(3.65709649161004,1.,-1.08395671077761));
#56962=CARTESIAN_POINT('Ctrl Pts',(3.64976441208197,1.,-1.08304289898577));
#56963=CARTESIAN_POINT('Ctrl Pts',(3.64214167843595,1.,-1.08194278850972));
#56964=CARTESIAN_POINT('Ctrl Pts',(3.63423373196602,1.,-1.08064765719887));
#56965=CARTESIAN_POINT('Ctrl Pts',(3.62619537902616,1.,-1.07919137290816));
#56966=CARTESIAN_POINT('Ctrl Pts',(3.61832318504957,1.,-1.07764868137729));
#56967=CARTESIAN_POINT('Ctrl Pts',(3.61098481349577,1.,-1.07611545402841));
#56968=CARTESIAN_POINT('Ctrl Pts',(3.6045633988796,1.,-1.0746932716863));
#56969=CARTESIAN_POINT('Ctrl Pts',(3.59940121154383,1.,-1.0734737254567));
#56970=CARTESIAN_POINT('Ctrl Pts',(3.59600583195037,1.,-1.07259084660947));
#56971=CARTESIAN_POINT('Ctrl Pts',(3.59439597,1.,-1.07209229745284));
#56972=CARTESIAN_POINT('Ctrl Pts',(3.59379266874663,1.,-1.07183575450716));
#56973=CARTESIAN_POINT('Ctrl Pts',(3.59363512797985,1.,-1.07171709254271));
#56974=CARTESIAN_POINT('Ctrl Pts',(3.59360648251021,1.,-1.071677399622));
#56975=CARTESIAN_POINT('',(4.06552750530042,0.,-1.05427041296137));
#56976=CARTESIAN_POINT('Origin',(4.10104028313088,0.,-0.906349047628866));
#56977=CARTESIAN_POINT('',(4.10104028313088,1.,-0.906349047628866));
#56978=CARTESIAN_POINT('',(4.06552750530042,1.,-1.05427041296137));
#56979=CARTESIAN_POINT('',(4.10104028313088,0.,-0.906349047628866));
#56980=CARTESIAN_POINT('Ctrl Pts',(3.68843977377012,-1.,-0.676691979611561));
#56981=CARTESIAN_POINT('Ctrl Pts',(3.68843977377012,1.,-0.676691979611561));
#56982=CARTESIAN_POINT('Ctrl Pts',(3.68838970675497,-1.,-0.67662079600199));
#56983=CARTESIAN_POINT('Ctrl Pts',(3.68838970675497,1.,-0.67662079600199));
#56984=CARTESIAN_POINT('Ctrl Pts',(3.68844918121303,-1.,-0.676525601650856));
#56985=CARTESIAN_POINT('Ctrl Pts',(3.68844918121303,1.,-0.676525601650856));
#56986=CARTESIAN_POINT('Ctrl Pts',(3.68901718136181,-1.,-0.676524321061226));
#56987=CARTESIAN_POINT('Ctrl Pts',(3.68901718136181,1.,-0.676524321061226));
#56988=CARTESIAN_POINT('Ctrl Pts',(3.69073278191994,-1.,-0.676805811075091));
#56989=CARTESIAN_POINT('Ctrl Pts',(3.69073278191994,1.,-0.676805811075091));
#56990=CARTESIAN_POINT('Ctrl Pts',(3.69443683573598,-1.,-0.677621861865498));
#56991=CARTESIAN_POINT('Ctrl Pts',(3.69443683573598,1.,-0.677621861865498));
#56992=CARTESIAN_POINT('Ctrl Pts',(3.69959004073005,-1.,-0.678878822226027));
#56993=CARTESIAN_POINT('Ctrl Pts',(3.69959004073005,1.,-0.678878822226027));
#56994=CARTESIAN_POINT('Ctrl Pts',(3.70595722031785,-1.,-0.680526909710877));
#56995=CARTESIAN_POINT('Ctrl Pts',(3.70595722031785,1.,-0.680526909710877));
#56996=CARTESIAN_POINT('Ctrl Pts',(3.71319182789943,-1.,-0.68249234510893));
#56997=CARTESIAN_POINT('Ctrl Pts',(3.71319182789943,1.,-0.68249234510893));
#56998=CARTESIAN_POINT('Ctrl Pts',(3.7209063713926,-1.,-0.684691698167848));
#56999=CARTESIAN_POINT('Ctrl Pts',(3.7209063713926,1.,-0.684691698167848));
#57000=CARTESIAN_POINT('Ctrl Pts',(3.72872973554051,-1.,-0.687043475232355));
#57001=CARTESIAN_POINT('Ctrl Pts',(3.72872973554051,1.,-0.687043475232355));
#57002=CARTESIAN_POINT('Ctrl Pts',(3.73636374475077,-1.,-0.689479637354814));
#57003=CARTESIAN_POINT('Ctrl Pts',(3.73636374475077,1.,-0.689479637354814));
#57004=CARTESIAN_POINT('Ctrl Pts',(3.74365508986712,-1.,-0.69196008040082));
#57005=CARTESIAN_POINT('Ctrl Pts',(3.74365508986712,1.,-0.69196008040082));
#57006=CARTESIAN_POINT('Ctrl Pts',(3.75060288243455,-1.,-0.694474562581493));
#57007=CARTESIAN_POINT('Ctrl Pts',(3.75060288243455,1.,-0.694474562581493));
#57008=CARTESIAN_POINT('Ctrl Pts',(3.75729775767023,-1.,-0.697031245659744));
#57009=CARTESIAN_POINT('Ctrl Pts',(3.75729775767023,1.,-0.697031245659744));
#57010=CARTESIAN_POINT('Ctrl Pts',(3.76387780603759,-1.,-0.699648552230917));
#57011=CARTESIAN_POINT('Ctrl Pts',(3.76387780603759,1.,-0.699648552230917));
#57012=CARTESIAN_POINT('Ctrl Pts',(3.77048141872872,-1.,-0.702346356621552));
#57013=CARTESIAN_POINT('Ctrl Pts',(3.77048141872872,1.,-0.702346356621552));
#57014=CARTESIAN_POINT('Ctrl Pts',(3.77719254217129,-1.,-0.705135847999817));
#57015=CARTESIAN_POINT('Ctrl Pts',(3.77719254217129,1.,-0.705135847999817));
#57016=CARTESIAN_POINT('Ctrl Pts',(3.78402183336605,-1.,-0.708015879375459));
#57017=CARTESIAN_POINT('Ctrl Pts',(3.78402183336605,1.,-0.708015879375459));
#57018=CARTESIAN_POINT('Ctrl Pts',(3.79093694007094,-1.,-0.710978231689017));
#57019=CARTESIAN_POINT('Ctrl Pts',(3.79093694007094,1.,-0.710978231689017));
#57020=CARTESIAN_POINT('Ctrl Pts',(3.79788100314975,-1.,-0.714010733006641));
#57021=CARTESIAN_POINT('Ctrl Pts',(3.79788100314975,1.,-0.714010733006641));
#57022=CARTESIAN_POINT('Ctrl Pts',(3.80479445759309,-1.,-0.717100993669115));
#57023=CARTESIAN_POINT('Ctrl Pts',(3.80479445759309,1.,-0.717100993669115));
#57024=CARTESIAN_POINT('Ctrl Pts',(3.81163885127344,-1.,-0.720240466589236));
#57025=CARTESIAN_POINT('Ctrl Pts',(3.81163885127344,1.,-0.720240466589236));
#57026=CARTESIAN_POINT('Ctrl Pts',(3.81840802610835,-1.,-0.723426346019423));
#57027=CARTESIAN_POINT('Ctrl Pts',(3.81840802610835,1.,-0.723426346019423));
#57028=CARTESIAN_POINT('Ctrl Pts',(3.82511495756713,-1.,-0.726659281876664));
#57029=CARTESIAN_POINT('Ctrl Pts',(3.82511495756713,1.,-0.726659281876664));
#57030=CARTESIAN_POINT('Ctrl Pts',(3.83178392403383,-1.,-0.729942010490168));
#57031=CARTESIAN_POINT('Ctrl Pts',(3.83178392403383,1.,-0.729942010490168));
#57032=CARTESIAN_POINT('Ctrl Pts',(3.83844103658009,-1.,-0.733277703756078));
#57033=CARTESIAN_POINT('Ctrl Pts',(3.83844103658009,1.,-0.733277703756078));
#57034=CARTESIAN_POINT('Ctrl Pts',(3.84510432881213,-1.,-0.736668240497118));
#57035=CARTESIAN_POINT('Ctrl Pts',(3.84510432881213,1.,-0.736668240497118));
#57036=CARTESIAN_POINT('Ctrl Pts',(3.85177770351215,-1.,-0.740113146827137));
#57037=CARTESIAN_POINT('Ctrl Pts',(3.85177770351215,1.,-0.740113146827137));
#57038=CARTESIAN_POINT('Ctrl Pts',(3.85845645217594,-1.,-0.743610542737013));
#57039=CARTESIAN_POINT('Ctrl Pts',(3.85845645217594,1.,-0.743610542737013));
#57040=CARTESIAN_POINT('Ctrl Pts',(3.86513062969889,-1.,-0.747157716488871));
#57041=CARTESIAN_POINT('Ctrl Pts',(3.86513062969889,1.,-0.747157716488871));
#57042=CARTESIAN_POINT('Ctrl Pts',(3.87178914078374,-1.,-0.750751822383028));
#57043=CARTESIAN_POINT('Ctrl Pts',(3.87178914078374,1.,-0.750751822383028));
#57044=CARTESIAN_POINT('Ctrl Pts',(3.87842382520065,-1.,-0.754390577396857));
#57045=CARTESIAN_POINT('Ctrl Pts',(3.87842382520065,1.,-0.754390577396857));
#57046=CARTESIAN_POINT('Ctrl Pts',(3.88503262662689,-1.,-0.758072800564801));
#57047=CARTESIAN_POINT('Ctrl Pts',(3.88503262662689,1.,-0.758072800564801));
#57048=CARTESIAN_POINT('Ctrl Pts',(3.89161738162245,-1.,-0.76179802879397));
#57049=CARTESIAN_POINT('Ctrl Pts',(3.89161738162245,1.,-0.76179802879397));
#57050=CARTESIAN_POINT('Ctrl Pts',(3.89818233104378,-1.,-0.765566256401296));
#57051=CARTESIAN_POINT('Ctrl Pts',(3.89818233104378,1.,-0.765566256401296));
#57052=CARTESIAN_POINT('Ctrl Pts',(3.90473237182633,-1.,-0.769377629847874));
#57053=CARTESIAN_POINT('Ctrl Pts',(3.90473237182633,1.,-0.769377629847874));
#57054=CARTESIAN_POINT('Ctrl Pts',(3.91127138115243,-1.,-0.773232154506321));
#57055=CARTESIAN_POINT('Ctrl Pts',(3.91127138115243,1.,-0.773232154506321));
#57056=CARTESIAN_POINT('Ctrl Pts',(3.9178006233448,-1.,-0.777129415664956));
#57057=CARTESIAN_POINT('Ctrl Pts',(3.9178006233448,1.,-0.777129415664956));
#57058=CARTESIAN_POINT('Ctrl Pts',(3.92431956510441,-1.,-0.781068718228451));
#57059=CARTESIAN_POINT('Ctrl Pts',(3.92431956510441,1.,-0.781068718228451));
#57060=CARTESIAN_POINT('Ctrl Pts',(3.93082655631789,-1.,-0.785049202786508));
#57061=CARTESIAN_POINT('Ctrl Pts',(3.93082655631789,1.,-0.785049202786508));
#57062=CARTESIAN_POINT('Ctrl Pts',(3.93731956885676,-1.,-0.789069971469333));
#57063=CARTESIAN_POINT('Ctrl Pts',(3.93731956885676,1.,-0.789069971469333));
#57064=CARTESIAN_POINT('Ctrl Pts',(3.94379688971283,-1.,-0.793130205640961));
#57065=CARTESIAN_POINT('Ctrl Pts',(3.94379688971283,1.,-0.793130205640961));
#57066=CARTESIAN_POINT('Ctrl Pts',(3.95025788827136,-1.,-0.797229296085316));
#57067=CARTESIAN_POINT('Ctrl Pts',(3.95025788827136,1.,-0.797229296085316));
#57068=CARTESIAN_POINT('Ctrl Pts',(3.95670276375108,-1.,-0.80136679772705));
#57069=CARTESIAN_POINT('Ctrl Pts',(3.95670276375108,1.,-0.80136679772705));
#57070=CARTESIAN_POINT('Ctrl Pts',(3.96313222295815,-1.,-0.805542372178362));
#57071=CARTESIAN_POINT('Ctrl Pts',(3.96313222295815,1.,-0.805542372178362));
#57072=CARTESIAN_POINT('Ctrl Pts',(3.96954717513232,-1.,-0.809755732818091));
#57073=CARTESIAN_POINT('Ctrl Pts',(3.96954717513232,1.,-0.809755732818091));
#57074=CARTESIAN_POINT('Ctrl Pts',(3.97594844078811,-1.,-0.814006592328844));
#57075=CARTESIAN_POINT('Ctrl Pts',(3.97594844078811,1.,-0.814006592328844));
#57076=CARTESIAN_POINT('Ctrl Pts',(3.98233640155404,-1.,-0.818294599022294));
#57077=CARTESIAN_POINT('Ctrl Pts',(3.98233640155404,1.,-0.818294599022294));
#57078=CARTESIAN_POINT('Ctrl Pts',(3.98871104646485,-1.,-0.822619346022119));
#57079=CARTESIAN_POINT('Ctrl Pts',(3.98871104646485,1.,-0.822619346022119));
#57080=CARTESIAN_POINT('Ctrl Pts',(3.99507212784431,-1.,-0.82698040032079));
#57081=CARTESIAN_POINT('Ctrl Pts',(3.99507212784431,1.,-0.82698040032079));
#57082=CARTESIAN_POINT('Ctrl Pts',(4.00141928477507,-1.,-0.831377325741623));
#57083=CARTESIAN_POINT('Ctrl Pts',(4.00141928477507,1.,-0.831377325741623));
#57084=CARTESIAN_POINT('Ctrl Pts',(4.00775216907856,-1.,-0.835809705809646));
#57085=CARTESIAN_POINT('Ctrl Pts',(4.00775216907856,1.,-0.835809705809646));
#57086=CARTESIAN_POINT('Ctrl Pts',(4.01407059766103,-1.,-0.840277171975855));
#57087=CARTESIAN_POINT('Ctrl Pts',(4.01407059766103,1.,-0.840277171975855));
#57088=CARTESIAN_POINT('Ctrl Pts',(4.02037456798441,-1.,-0.844779403287746));
#57089=CARTESIAN_POINT('Ctrl Pts',(4.02037456798441,1.,-0.844779403287746));
#57090=CARTESIAN_POINT('Ctrl Pts',(4.02666418343164,-1.,-0.849316107474245));
#57091=CARTESIAN_POINT('Ctrl Pts',(4.02666418343164,1.,-0.849316107474245));
#57092=CARTESIAN_POINT('Ctrl Pts',(4.03293960436756,-1.,-0.853887006631755));
#57093=CARTESIAN_POINT('Ctrl Pts',(4.03293960436756,1.,-0.853887006631755));
#57094=CARTESIAN_POINT('Ctrl Pts',(4.03920099284773,-1.,-0.858491822322828));
#57095=CARTESIAN_POINT('Ctrl Pts',(4.03920099284773,1.,-0.858491822322828));
#57096=CARTESIAN_POINT('Ctrl Pts',(4.04544845048584,-1.,-0.863130256643259));
#57097=CARTESIAN_POINT('Ctrl Pts',(4.04544845048584,1.,-0.863130256643259));
#57098=CARTESIAN_POINT('Ctrl Pts',(4.05168199437909,-1.,-0.867801988859918));
#57099=CARTESIAN_POINT('Ctrl Pts',(4.05168199437909,1.,-0.867801988859918));
#57100=CARTESIAN_POINT('Ctrl Pts',(4.0579015903134,-1.,-0.872506694782446));
#57101=CARTESIAN_POINT('Ctrl Pts',(4.0579015903134,1.,-0.872506694782446));
#57102=CARTESIAN_POINT('Ctrl Pts',(4.06410717232905,-1.,-0.877244060485838));
#57103=CARTESIAN_POINT('Ctrl Pts',(4.06410717232905,1.,-0.877244060485838));
#57104=CARTESIAN_POINT('Ctrl Pts',(4.07029866694192,-1.,-0.882013797525692));
#57105=CARTESIAN_POINT('Ctrl Pts',(4.07029866694192,1.,-0.882013797525692));
#57106=CARTESIAN_POINT('Ctrl Pts',(4.07647601773635,-1.,-0.886815658358501));
#57107=CARTESIAN_POINT('Ctrl Pts',(4.07647601773635,1.,-0.886815658358501));
#57108=CARTESIAN_POINT('Ctrl Pts',(4.08263920304799,-1.,-0.891649447916278));
#57109=CARTESIAN_POINT('Ctrl Pts',(4.08263920304799,1.,-0.891649447916278));
#57110=CARTESIAN_POINT('Ctrl Pts',(4.08878822246833,-1.,-0.896515019231334));
#57111=CARTESIAN_POINT('Ctrl Pts',(4.08878822246833,1.,-0.896515019231334));
#57112=CARTESIAN_POINT('Ctrl Pts',(4.09369611522387,-1.,-0.900432820941675));
#57113=CARTESIAN_POINT('Ctrl Pts',(4.09369611522387,1.,-0.900432820941675));
#57114=CARTESIAN_POINT('Ctrl Pts',(4.09737067245935,-1.,-0.903385402441588));
#57115=CARTESIAN_POINT('Ctrl Pts',(4.09737067245935,1.,-0.903385402441588));
#57116=CARTESIAN_POINT('Ctrl Pts',(4.09981755067523,-1.,-0.905360112215337));
#57117=CARTESIAN_POINT('Ctrl Pts',(4.09981755067523,1.,-0.905360112215337));
#57118=CARTESIAN_POINT('Ctrl Pts',(4.10104028313088,-1.,-0.906349047628866));
#57119=CARTESIAN_POINT('Ctrl Pts',(4.10104028313088,1.,-0.906349047628866));
#57120=CARTESIAN_POINT('',(3.68845817949586,1.,-0.676591647975427));
#57121=CARTESIAN_POINT('Ctrl Pts',(3.68845817949586,-1.,-0.676591647975429));
#57122=CARTESIAN_POINT('Ctrl Pts',(3.68845817949586,-0.666666666666667,
-0.676591647975429));
#57123=CARTESIAN_POINT('Ctrl Pts',(3.68845817949586,-0.333333333333333,
-0.676591647975429));
#57124=CARTESIAN_POINT('Ctrl Pts',(3.68845817949586,0.333333333333333,-0.676591647975429));
#57125=CARTESIAN_POINT('Ctrl Pts',(3.68845817949586,0.666666666666667,-0.676591647975429));
#57126=CARTESIAN_POINT('Ctrl Pts',(3.68845817949586,1.,-0.676591647975429));
#57127=CARTESIAN_POINT('Ctrl Pts',(3.68845817949586,1.,-0.676591647975428));
#57128=CARTESIAN_POINT('Ctrl Pts',(3.68850172300477,1.,-0.676569286094606));
#57129=CARTESIAN_POINT('Ctrl Pts',(3.68869596425969,1.,-0.676535079520807));
#57130=CARTESIAN_POINT('Ctrl Pts',(3.68934997767243,1.,-0.676580391119397));
#57131=CARTESIAN_POINT('Ctrl Pts',(3.69101071175464,1.,-0.676867042599402));
#57132=CARTESIAN_POINT('Ctrl Pts',(3.69443683573598,1.,-0.677621861865498));
#57133=CARTESIAN_POINT('Ctrl Pts',(3.69959004073005,1.,-0.678878822226027));
#57134=CARTESIAN_POINT('Ctrl Pts',(3.70595722031785,1.,-0.680526909710877));
#57135=CARTESIAN_POINT('Ctrl Pts',(3.71319182789943,1.,-0.68249234510893));
#57136=CARTESIAN_POINT('Ctrl Pts',(3.7209063713926,1.,-0.684691698167848));
#57137=CARTESIAN_POINT('Ctrl Pts',(3.72872973554051,1.,-0.687043475232355));
#57138=CARTESIAN_POINT('Ctrl Pts',(3.73636374475077,1.,-0.689479637354814));
#57139=CARTESIAN_POINT('Ctrl Pts',(3.74365508986712,1.,-0.69196008040082));
#57140=CARTESIAN_POINT('Ctrl Pts',(3.75060288243455,1.,-0.694474562581493));
#57141=CARTESIAN_POINT('Ctrl Pts',(3.75729775767023,1.,-0.697031245659744));
#57142=CARTESIAN_POINT('Ctrl Pts',(3.76387780603759,1.,-0.699648552230917));
#57143=CARTESIAN_POINT('Ctrl Pts',(3.77048141872872,1.,-0.702346356621552));
#57144=CARTESIAN_POINT('Ctrl Pts',(3.77719254217129,1.,-0.705135847999817));
#57145=CARTESIAN_POINT('Ctrl Pts',(3.78402183336605,1.,-0.708015879375459));
#57146=CARTESIAN_POINT('Ctrl Pts',(3.79093694007094,1.,-0.710978231689017));
#57147=CARTESIAN_POINT('Ctrl Pts',(3.79788100314975,1.,-0.714010733006641));
#57148=CARTESIAN_POINT('Ctrl Pts',(3.80479445759309,1.,-0.717100993669115));
#57149=CARTESIAN_POINT('Ctrl Pts',(3.81163885127344,1.,-0.720240466589236));
#57150=CARTESIAN_POINT('Ctrl Pts',(3.81840802610835,1.,-0.723426346019423));
#57151=CARTESIAN_POINT('Ctrl Pts',(3.82511495756713,1.,-0.726659281876664));
#57152=CARTESIAN_POINT('Ctrl Pts',(3.83178392403383,1.,-0.729942010490168));
#57153=CARTESIAN_POINT('Ctrl Pts',(3.83844103658009,1.,-0.733277703756078));
#57154=CARTESIAN_POINT('Ctrl Pts',(3.84510432881213,1.,-0.736668240497118));
#57155=CARTESIAN_POINT('Ctrl Pts',(3.85177770351215,1.,-0.740113146827137));
#57156=CARTESIAN_POINT('Ctrl Pts',(3.85845645217594,1.,-0.743610542737013));
#57157=CARTESIAN_POINT('Ctrl Pts',(3.86513062969889,1.,-0.747157716488871));
#57158=CARTESIAN_POINT('Ctrl Pts',(3.87178914078374,1.,-0.750751822383028));
#57159=CARTESIAN_POINT('Ctrl Pts',(3.87842382520065,1.,-0.754390577396857));
#57160=CARTESIAN_POINT('Ctrl Pts',(3.88503262662689,1.,-0.758072800564801));
#57161=CARTESIAN_POINT('Ctrl Pts',(3.89161738162245,1.,-0.76179802879397));
#57162=CARTESIAN_POINT('Ctrl Pts',(3.89818233104378,1.,-0.765566256401296));
#57163=CARTESIAN_POINT('Ctrl Pts',(3.90473237182633,1.,-0.769377629847874));
#57164=CARTESIAN_POINT('Ctrl Pts',(3.91127138115243,1.,-0.773232154506321));
#57165=CARTESIAN_POINT('Ctrl Pts',(3.9178006233448,1.,-0.777129415664956));
#57166=CARTESIAN_POINT('Ctrl Pts',(3.92431956510441,1.,-0.781068718228451));
#57167=CARTESIAN_POINT('Ctrl Pts',(3.93082655631789,1.,-0.785049202786508));
#57168=CARTESIAN_POINT('Ctrl Pts',(3.93731956885676,1.,-0.789069971469333));
#57169=CARTESIAN_POINT('Ctrl Pts',(3.94379688971283,1.,-0.793130205640961));
#57170=CARTESIAN_POINT('Ctrl Pts',(3.95025788827136,1.,-0.797229296085316));
#57171=CARTESIAN_POINT('Ctrl Pts',(3.95670276375108,1.,-0.80136679772705));
#57172=CARTESIAN_POINT('Ctrl Pts',(3.96313222295815,1.,-0.805542372178362));
#57173=CARTESIAN_POINT('Ctrl Pts',(3.96954717513232,1.,-0.809755732818091));
#57174=CARTESIAN_POINT('Ctrl Pts',(3.97594844078811,1.,-0.814006592328844));
#57175=CARTESIAN_POINT('Ctrl Pts',(3.98233640155404,1.,-0.818294599022294));
#57176=CARTESIAN_POINT('Ctrl Pts',(3.98871104646485,1.,-0.822619346022119));
#57177=CARTESIAN_POINT('Ctrl Pts',(3.99507212784431,1.,-0.82698040032079));
#57178=CARTESIAN_POINT('Ctrl Pts',(4.00141928477507,1.,-0.831377325741623));
#57179=CARTESIAN_POINT('Ctrl Pts',(4.00775216907856,1.,-0.835809705809646));
#57180=CARTESIAN_POINT('Ctrl Pts',(4.01407059766103,1.,-0.840277171975855));
#57181=CARTESIAN_POINT('Ctrl Pts',(4.02037456798441,1.,-0.844779403287746));
#57182=CARTESIAN_POINT('Ctrl Pts',(4.02666418343164,1.,-0.849316107474245));
#57183=CARTESIAN_POINT('Ctrl Pts',(4.03293960436756,1.,-0.853887006631755));
#57184=CARTESIAN_POINT('Ctrl Pts',(4.03920099284773,1.,-0.858491822322828));
#57185=CARTESIAN_POINT('Ctrl Pts',(4.04544845048584,1.,-0.863130256643259));
#57186=CARTESIAN_POINT('Ctrl Pts',(4.05168199437909,1.,-0.867801988859918));
#57187=CARTESIAN_POINT('Ctrl Pts',(4.0579015903134,1.,-0.872506694782446));
#57188=CARTESIAN_POINT('Ctrl Pts',(4.06410717232905,1.,-0.877244060485838));
#57189=CARTESIAN_POINT('Ctrl Pts',(4.07029866694192,1.,-0.882013797525692));
#57190=CARTESIAN_POINT('Ctrl Pts',(4.07647601773635,1.,-0.886815658358501));
#57191=CARTESIAN_POINT('Ctrl Pts',(4.08263920304799,1.,-0.891649447916278));
#57192=CARTESIAN_POINT('Ctrl Pts',(4.08878822246833,1.,-0.896515019231334));
#57193=CARTESIAN_POINT('Ctrl Pts',(4.09369611522387,1.,-0.900432820941675));
#57194=CARTESIAN_POINT('Ctrl Pts',(4.09737067245935,1.,-0.903385402441588));
#57195=CARTESIAN_POINT('Ctrl Pts',(4.09981755067523,1.,-0.905360112215337));
#57196=CARTESIAN_POINT('Ctrl Pts',(4.10104028313088,1.,-0.906349047628866));
#57197=CARTESIAN_POINT('Origin',(0.,0.,0.));
#57198=CARTESIAN_POINT('',(3.71701050416802,1.,-0.496319364829374));
#57199=CARTESIAN_POINT('Origin',(0.,1.,0.));
#57200=CARTESIAN_POINT('Ctrl Pts',(3.71701050416802,1.,-0.496319364829374));
#57201=CARTESIAN_POINT('Ctrl Pts',(3.71701050416802,0.666666666666667,-0.496319364829374));
#57202=CARTESIAN_POINT('Ctrl Pts',(3.71701050416802,0.333333333333333,-0.496319364829374));
#57203=CARTESIAN_POINT('Ctrl Pts',(3.71701050416802,-0.333333333333333,
-0.496319364829374));
#57204=CARTESIAN_POINT('Ctrl Pts',(3.71701050416802,-0.666666666666667,
-0.496319364829374));
#57205=CARTESIAN_POINT('Ctrl Pts',(3.71701050416802,-1.,-0.496319364829374));
#57206=CARTESIAN_POINT('Ctrl Pts',(3.74888690736767,-1.,-0.0913616755937424));
#57207=CARTESIAN_POINT('Ctrl Pts',(3.74888690736767,1.,-0.0913616755937424));
#57208=CARTESIAN_POINT('Ctrl Pts',(3.74882632119067,-1.,-0.0912992005792589));
#57209=CARTESIAN_POINT('Ctrl Pts',(3.74882632119067,1.,-0.0912992005792589));
#57210=CARTESIAN_POINT('Ctrl Pts',(3.74887017174206,-1.,-0.0911958743735238));
#57211=CARTESIAN_POINT('Ctrl Pts',(3.74887017174206,1.,-0.0911958743735238));
#57212=CARTESIAN_POINT('Ctrl Pts',(3.74943097853811,-1.,-0.0911057547506604));
#57213=CARTESIAN_POINT('Ctrl Pts',(3.74943097853811,1.,-0.0911057547506604));
#57214=CARTESIAN_POINT('Ctrl Pts',(3.75116949194623,-1.,-0.0911154000998146));
#57215=CARTESIAN_POINT('Ctrl Pts',(3.75116949194623,1.,-0.0911154000998146));
#57216=CARTESIAN_POINT('Ctrl Pts',(3.75495560118212,-1.,-0.0913419622736402));
#57217=CARTESIAN_POINT('Ctrl Pts',(3.75495560118212,1.,-0.0913419622736402));
#57218=CARTESIAN_POINT('Ctrl Pts',(3.76024199359303,-1.,-0.0917773084998339));
#57219=CARTESIAN_POINT('Ctrl Pts',(3.76024199359303,1.,-0.0917773084998339));
#57220=CARTESIAN_POINT('Ctrl Pts',(3.76678860031841,-1.,-0.0924090589602695));
#57221=CARTESIAN_POINT('Ctrl Pts',(3.76678860031841,1.,-0.0924090589602695));
#57222=CARTESIAN_POINT('Ctrl Pts',(3.77424159971059,-1.,-0.0932185546203182));
#57223=CARTESIAN_POINT('Ctrl Pts',(3.77424159971059,1.,-0.0932185546203182));
#57224=CARTESIAN_POINT('Ctrl Pts',(3.782205218991,-1.,-0.0941840095090818));
#57225=CARTESIAN_POINT('Ctrl Pts',(3.782205218991,1.,-0.0941840095090818));
#57226=CARTESIAN_POINT('Ctrl Pts',(3.79030016353111,-1.,-0.0952829885100805));
#57227=CARTESIAN_POINT('Ctrl Pts',(3.79030016353111,1.,-0.0952829885100805));
#57228=CARTESIAN_POINT('Ctrl Pts',(3.79822128513845,-1.,-0.0964949352873135));
#57229=CARTESIAN_POINT('Ctrl Pts',(3.79822128513845,1.,-0.0964949352873135));
#57230=CARTESIAN_POINT('Ctrl Pts',(3.80581088847809,-1.,-0.0978042222906647));
#57231=CARTESIAN_POINT('Ctrl Pts',(3.80581088847809,1.,-0.0978042222906647));
#57232=CARTESIAN_POINT('Ctrl Pts',(3.81306649386461,-1.,-0.0992008728096518));
#57233=CARTESIAN_POINT('Ctrl Pts',(3.81306649386461,1.,-0.0992008728096518));
#57234=CARTESIAN_POINT('Ctrl Pts',(3.82007889742625,-1.,-0.100678769650632));
#57235=CARTESIAN_POINT('Ctrl Pts',(3.82007889742625,1.,-0.100678769650632));
#57236=CARTESIAN_POINT('Ctrl Pts',(3.82698737143255,-1.,-0.102234506488457));
#57237=CARTESIAN_POINT('Ctrl Pts',(3.82698737143255,1.,-0.102234506488457));
#57238=CARTESIAN_POINT('Ctrl Pts',(3.83393171228002,-1.,-0.103866063811623));
#57239=CARTESIAN_POINT('Ctrl Pts',(3.83393171228002,1.,-0.103866063811623));
#57240=CARTESIAN_POINT('Ctrl Pts',(3.84099658324803,-1.,-0.105571360916569));
#57241=CARTESIAN_POINT('Ctrl Pts',(3.84099658324803,1.,-0.105571360916569));
#57242=CARTESIAN_POINT('Ctrl Pts',(3.84819233070317,-1.,-0.107347597812184));
#57243=CARTESIAN_POINT('Ctrl Pts',(3.84819233070317,1.,-0.107347597812184));
#57244=CARTESIAN_POINT('Ctrl Pts',(3.855485714969,-1.,-0.109191717634944));
#57245=CARTESIAN_POINT('Ctrl Pts',(3.855485714969,1.,-0.109191717634944));
#57246=CARTESIAN_POINT('Ctrl Pts',(3.86281867282965,-1.,-0.111100593036261));
#57247=CARTESIAN_POINT('Ctrl Pts',(3.86281867282965,1.,-0.111100593036261));
#57248=CARTESIAN_POINT('Ctrl Pts',(3.87013043445014,-1.,-0.113071304914562));
#57249=CARTESIAN_POINT('Ctrl Pts',(3.87013043445014,1.,-0.113071304914562));
#57250=CARTESIAN_POINT('Ctrl Pts',(3.87738168405343,-1.,-0.11510142664947));
#57251=CARTESIAN_POINT('Ctrl Pts',(3.87738168405343,1.,-0.11510142664947));
#57252=CARTESIAN_POINT('Ctrl Pts',(3.88456590045767,-1.,-0.117189150373144));
#57253=CARTESIAN_POINT('Ctrl Pts',(3.88456590045767,1.,-0.117189150373144));
#57254=CARTESIAN_POINT('Ctrl Pts',(3.89169600105201,-1.,-0.119333088190418));
#57255=CARTESIAN_POINT('Ctrl Pts',(3.89169600105201,1.,-0.119333088190418));
#57256=CARTESIAN_POINT('Ctrl Pts',(3.89879639336952,-1.,-0.121532144765723));
#57257=CARTESIAN_POINT('Ctrl Pts',(3.89879639336952,1.,-0.121532144765723));
#57258=CARTESIAN_POINT('Ctrl Pts',(3.90589336320508,-1.,-0.123785368272378));
#57259=CARTESIAN_POINT('Ctrl Pts',(3.90589336320508,1.,-0.123785368272378));
#57260=CARTESIAN_POINT('Ctrl Pts',(3.91300501605392,-1.,-0.126091793324137));
#57261=CARTESIAN_POINT('Ctrl Pts',(3.91300501605392,1.,-0.126091793324137));
#57262=CARTESIAN_POINT('Ctrl Pts',(3.92013513251642,-1.,-0.128450341339528));
#57263=CARTESIAN_POINT('Ctrl Pts',(3.92013513251642,1.,-0.128450341339528));
#57264=CARTESIAN_POINT('Ctrl Pts',(3.9272787679596,-1.,-0.130859892027799));
#57265=CARTESIAN_POINT('Ctrl Pts',(3.9272787679596,1.,-0.130859892027799));
#57266=CARTESIAN_POINT('Ctrl Pts',(3.93442567551035,-1.,-0.13331932279419));
#57267=CARTESIAN_POINT('Ctrl Pts',(3.93442567551035,1.,-0.13331932279419));
#57268=CARTESIAN_POINT('Ctrl Pts',(3.94156445130744,-1.,-0.135827558661188));
#57269=CARTESIAN_POINT('Ctrl Pts',(3.94156445130744,1.,-0.135827558661188));
#57270=CARTESIAN_POINT('Ctrl Pts',(3.94868667844355,-1.,-0.138383621255159));
#57271=CARTESIAN_POINT('Ctrl Pts',(3.94868667844355,1.,-0.138383621255159));
#57272=CARTESIAN_POINT('Ctrl Pts',(3.95579014116899,-1.,-0.140986665829937));
#57273=CARTESIAN_POINT('Ctrl Pts',(3.95579014116899,1.,-0.140986665829937));
#57274=CARTESIAN_POINT('Ctrl Pts',(3.96287658098896,-1.,-0.143635947692791));
#57275=CARTESIAN_POINT('Ctrl Pts',(3.96287658098896,1.,-0.143635947692791));
#57276=CARTESIAN_POINT('Ctrl Pts',(3.96995018565891,-1.,-0.146330797814514));
#57277=CARTESIAN_POINT('Ctrl Pts',(3.96995018565891,1.,-0.146330797814514));
#57278=CARTESIAN_POINT('Ctrl Pts',(3.97701581473643,-1.,-0.149070594803544));
#57279=CARTESIAN_POINT('Ctrl Pts',(3.97701581473643,1.,-0.149070594803544));
#57280=CARTESIAN_POINT('Ctrl Pts',(3.9840772985098,-1.,-0.151854737441406));
#57281=CARTESIAN_POINT('Ctrl Pts',(3.9840772985098,1.,-0.151854737441406));
#57282=CARTESIAN_POINT('Ctrl Pts',(3.99113582086059,-1.,-0.154682618338563));
#57283=CARTESIAN_POINT('Ctrl Pts',(3.99113582086059,1.,-0.154682618338563));
#57284=CARTESIAN_POINT('Ctrl Pts',(3.99819074631874,-1.,-0.15755363438381));
#57285=CARTESIAN_POINT('Ctrl Pts',(3.99819074631874,1.,-0.15755363438381));
#57286=CARTESIAN_POINT('Ctrl Pts',(4.00524031064509,-1.,-0.160467194882219));
#57287=CARTESIAN_POINT('Ctrl Pts',(4.00524031064509,1.,-0.160467194882219));
#57288=CARTESIAN_POINT('Ctrl Pts',(4.01228237022301,-1.,-0.163422730287459));
#57289=CARTESIAN_POINT('Ctrl Pts',(4.01228237022301,1.,-0.163422730287459));
#57290=CARTESIAN_POINT('Ctrl Pts',(4.01931510507143,-1.,-0.166419700015848));
#57291=CARTESIAN_POINT('Ctrl Pts',(4.01931510507143,1.,-0.166419700015848));
#57292=CARTESIAN_POINT('Ctrl Pts',(4.0263377970371,-1.,-0.169457601001653));
#57293=CARTESIAN_POINT('Ctrl Pts',(4.0263377970371,1.,-0.169457601001653));
#57294=CARTESIAN_POINT('Ctrl Pts',(4.03335057326093,-1.,-0.172535962484467));
#57295=CARTESIAN_POINT('Ctrl Pts',(4.03335057326093,1.,-0.172535962484467));
#57296=CARTESIAN_POINT('Ctrl Pts',(4.04035407891161,-1.,-0.175654339673758));
#57297=CARTESIAN_POINT('Ctrl Pts',(4.04035407891161,1.,-0.175654339673758));
#57298=CARTESIAN_POINT('Ctrl Pts',(4.04734916719722,-1.,-0.178812307240716));
#57299=CARTESIAN_POINT('Ctrl Pts',(4.04734916719722,1.,-0.178812307240716));
#57300=CARTESIAN_POINT('Ctrl Pts',(4.05433660358402,-1.,-0.18200945304855));
#57301=CARTESIAN_POINT('Ctrl Pts',(4.05433660358402,1.,-0.18200945304855));
#57302=CARTESIAN_POINT('Ctrl Pts',(4.06131670998589,-1.,-0.185245370038948));
#57303=CARTESIAN_POINT('Ctrl Pts',(4.06131670998589,1.,-0.185245370038948));
#57304=CARTESIAN_POINT('Ctrl Pts',(4.06828941192308,-1.,-0.188519658060256));
#57305=CARTESIAN_POINT('Ctrl Pts',(4.06828941192308,1.,-0.188519658060256));
#57306=CARTESIAN_POINT('Ctrl Pts',(4.07525439703137,-1.,-0.191831928181081));
#57307=CARTESIAN_POINT('Ctrl Pts',(4.07525439703137,1.,-0.191831928181081));
#57308=CARTESIAN_POINT('Ctrl Pts',(4.08221124060385,-1.,-0.195181806054714));
#57309=CARTESIAN_POINT('Ctrl Pts',(4.08221124060385,1.,-0.195181806054714));
#57310=CARTESIAN_POINT('Ctrl Pts',(4.08915953359753,-1.,-0.198568934800811));
#57311=CARTESIAN_POINT('Ctrl Pts',(4.08915953359753,1.,-0.198568934800811));
#57312=CARTESIAN_POINT('Ctrl Pts',(4.09609903751912,-1.,-0.201992979049985));
#57313=CARTESIAN_POINT('Ctrl Pts',(4.09609903751912,1.,-0.201992979049985));
#57314=CARTESIAN_POINT('Ctrl Pts',(4.10302969965374,-1.,-0.205453622198233));
#57315=CARTESIAN_POINT('Ctrl Pts',(4.10302969965374,1.,-0.205453622198233));
#57316=CARTESIAN_POINT('Ctrl Pts',(4.10995157639026,-1.,-0.208950559400172));
#57317=CARTESIAN_POINT('Ctrl Pts',(4.10995157639026,1.,-0.208950559400172));
#57318=CARTESIAN_POINT('Ctrl Pts',(4.11686478264545,-1.,-0.212483491087068));
#57319=CARTESIAN_POINT('Ctrl Pts',(4.11686478264545,1.,-0.212483491087068));
#57320=CARTESIAN_POINT('Ctrl Pts',(4.12376943492249,-1.,-0.216052116898425));
#57321=CARTESIAN_POINT('Ctrl Pts',(4.12376943492249,1.,-0.216052116898425));
#57322=CARTESIAN_POINT('Ctrl Pts',(4.13066558698156,-1.,-0.219656126701852));
#57323=CARTESIAN_POINT('Ctrl Pts',(4.13066558698156,1.,-0.219656126701852));
#57324=CARTESIAN_POINT('Ctrl Pts',(4.13755320553563,-1.,-0.223295201038384));
#57325=CARTESIAN_POINT('Ctrl Pts',(4.13755320553563,1.,-0.223295201038384));
#57326=CARTESIAN_POINT('Ctrl Pts',(4.14443220607733,-1.,-0.226969025061244));
#57327=CARTESIAN_POINT('Ctrl Pts',(4.14443220607733,1.,-0.226969025061244));
#57328=CARTESIAN_POINT('Ctrl Pts',(4.15130247435029,-1.,-0.230677299028738));
#57329=CARTESIAN_POINT('Ctrl Pts',(4.15130247435029,1.,-0.230677299028738));
#57330=CARTESIAN_POINT('Ctrl Pts',(4.1581638926525,-1.,-0.234419749543143));
#57331=CARTESIAN_POINT('Ctrl Pts',(4.1581638926525,1.,-0.234419749543143));
#57332=CARTESIAN_POINT('Ctrl Pts',(4.1650163665385,-1.,-0.238196140933977));
#57333=CARTESIAN_POINT('Ctrl Pts',(4.1650163665385,1.,-0.238196140933977));
#57334=CARTESIAN_POINT('Ctrl Pts',(4.17185984409533,-1.,-0.242006283923912));
#57335=CARTESIAN_POINT('Ctrl Pts',(4.17185984409533,1.,-0.242006283923912));
#57336=CARTESIAN_POINT('Ctrl Pts',(4.17869430192868,-1.,-0.245850033418584));
#57337=CARTESIAN_POINT('Ctrl Pts',(4.17869430192868,1.,-0.245850033418584));
#57338=CARTESIAN_POINT('Ctrl Pts',(4.18415464959491,-1.,-0.248951836910964));
#57339=CARTESIAN_POINT('Ctrl Pts',(4.18415464959491,1.,-0.248951836910964));
#57340=CARTESIAN_POINT('Ctrl Pts',(4.18824585244066,-1.,-0.251293239837693));
#57341=CARTESIAN_POINT('Ctrl Pts',(4.18824585244066,1.,-0.251293239837693));
#57342=CARTESIAN_POINT('Ctrl Pts',(4.19097151819241,-1.,-0.252860861572566));
#57343=CARTESIAN_POINT('Ctrl Pts',(4.19097151819241,1.,-0.252860861572566));
#57344=CARTESIAN_POINT('Ctrl Pts',(4.1923339003649,-1.,-0.253646344052521));
#57345=CARTESIAN_POINT('Ctrl Pts',(4.1923339003649,1.,-0.253646344052521));
#57346=CARTESIAN_POINT('',(3.74888939116255,1.,-0.0912596999166826));
#57347=CARTESIAN_POINT('Ctrl Pts',(3.74888939116255,-1.,-0.0912596999166829));
#57348=CARTESIAN_POINT('Ctrl Pts',(3.74888939116255,-0.666666666666667,
-0.0912596999166829));
#57349=CARTESIAN_POINT('Ctrl Pts',(3.74888939116255,-0.333333333333333,
-0.0912596999166829));
#57350=CARTESIAN_POINT('Ctrl Pts',(3.74888939116255,0.333333333333333,-0.0912596999166829));
#57351=CARTESIAN_POINT('Ctrl Pts',(3.74888939116255,0.666666666666667,-0.0912596999166829));
#57352=CARTESIAN_POINT('Ctrl Pts',(3.74888939116255,1.,-0.0912596999166829));
#57353=CARTESIAN_POINT('',(4.1923339003649,1.,-0.253646344052521));
#57354=CARTESIAN_POINT('',(4.1923339003649,0.,-0.253646344052521));
#57355=CARTESIAN_POINT('Ctrl Pts',(3.74888939116255,1.,-0.0912596999166826));
#57356=CARTESIAN_POINT('Ctrl Pts',(3.74892890040974,1.,-0.0912308016421984));
#57357=CARTESIAN_POINT('Ctrl Pts',(3.74911539914542,1.,-0.0911666301812821));
#57358=CARTESIAN_POINT('Ctrl Pts',(3.74976844886346,1.,-0.0911090736805514));
#57359=CARTESIAN_POINT('Ctrl Pts',(3.75145357872422,1.,-0.091132399957443));
#57360=CARTESIAN_POINT('Ctrl Pts',(3.75495560118212,1.,-0.0913419622736402));
#57361=CARTESIAN_POINT('Ctrl Pts',(3.76024199359303,1.,-0.0917773084998339));
#57362=CARTESIAN_POINT('Ctrl Pts',(3.76678860031841,1.,-0.0924090589602695));
#57363=CARTESIAN_POINT('Ctrl Pts',(3.77424159971059,1.,-0.0932185546203182));
#57364=CARTESIAN_POINT('Ctrl Pts',(3.782205218991,1.,-0.0941840095090818));
#57365=CARTESIAN_POINT('Ctrl Pts',(3.79030016353111,1.,-0.0952829885100805));
#57366=CARTESIAN_POINT('Ctrl Pts',(3.79822128513845,1.,-0.0964949352873135));
#57367=CARTESIAN_POINT('Ctrl Pts',(3.80581088847809,1.,-0.0978042222906647));
#57368=CARTESIAN_POINT('Ctrl Pts',(3.81306649386461,1.,-0.0992008728096518));
#57369=CARTESIAN_POINT('Ctrl Pts',(3.82007889742625,1.,-0.100678769650632));
#57370=CARTESIAN_POINT('Ctrl Pts',(3.82698737143255,1.,-0.102234506488457));
#57371=CARTESIAN_POINT('Ctrl Pts',(3.83393171228002,1.,-0.103866063811623));
#57372=CARTESIAN_POINT('Ctrl Pts',(3.84099658324803,1.,-0.105571360916569));
#57373=CARTESIAN_POINT('Ctrl Pts',(3.84819233070317,1.,-0.107347597812184));
#57374=CARTESIAN_POINT('Ctrl Pts',(3.855485714969,1.,-0.109191717634944));
#57375=CARTESIAN_POINT('Ctrl Pts',(3.86281867282965,1.,-0.111100593036261));
#57376=CARTESIAN_POINT('Ctrl Pts',(3.87013043445014,1.,-0.113071304914562));
#57377=CARTESIAN_POINT('Ctrl Pts',(3.87738168405343,1.,-0.11510142664947));
#57378=CARTESIAN_POINT('Ctrl Pts',(3.88456590045767,1.,-0.117189150373144));
#57379=CARTESIAN_POINT('Ctrl Pts',(3.89169600105201,1.,-0.119333088190418));
#57380=CARTESIAN_POINT('Ctrl Pts',(3.89879639336952,1.,-0.121532144765723));
#57381=CARTESIAN_POINT('Ctrl Pts',(3.90589336320508,1.,-0.123785368272378));
#57382=CARTESIAN_POINT('Ctrl Pts',(3.91300501605392,1.,-0.126091793324137));
#57383=CARTESIAN_POINT('Ctrl Pts',(3.92013513251642,1.,-0.128450341339528));
#57384=CARTESIAN_POINT('Ctrl Pts',(3.9272787679596,1.,-0.130859892027799));
#57385=CARTESIAN_POINT('Ctrl Pts',(3.93442567551035,1.,-0.13331932279419));
#57386=CARTESIAN_POINT('Ctrl Pts',(3.94156445130744,1.,-0.135827558661188));
#57387=CARTESIAN_POINT('Ctrl Pts',(3.94868667844355,1.,-0.138383621255159));
#57388=CARTESIAN_POINT('Ctrl Pts',(3.95579014116899,1.,-0.140986665829937));
#57389=CARTESIAN_POINT('Ctrl Pts',(3.96287658098896,1.,-0.143635947692791));
#57390=CARTESIAN_POINT('Ctrl Pts',(3.96995018565891,1.,-0.146330797814514));
#57391=CARTESIAN_POINT('Ctrl Pts',(3.97701581473643,1.,-0.149070594803544));
#57392=CARTESIAN_POINT('Ctrl Pts',(3.9840772985098,1.,-0.151854737441406));
#57393=CARTESIAN_POINT('Ctrl Pts',(3.99113582086059,1.,-0.154682618338563));
#57394=CARTESIAN_POINT('Ctrl Pts',(3.99819074631874,1.,-0.15755363438381));
#57395=CARTESIAN_POINT('Ctrl Pts',(4.00524031064509,1.,-0.160467194882219));
#57396=CARTESIAN_POINT('Ctrl Pts',(4.01228237022301,1.,-0.163422730287459));
#57397=CARTESIAN_POINT('Ctrl Pts',(4.01931510507143,1.,-0.166419700015848));
#57398=CARTESIAN_POINT('Ctrl Pts',(4.0263377970371,1.,-0.169457601001653));
#57399=CARTESIAN_POINT('Ctrl Pts',(4.03335057326093,1.,-0.172535962484467));
#57400=CARTESIAN_POINT('Ctrl Pts',(4.04035407891161,1.,-0.175654339673758));
#57401=CARTESIAN_POINT('Ctrl Pts',(4.04734916719722,1.,-0.178812307240716));
#57402=CARTESIAN_POINT('Ctrl Pts',(4.05433660358402,1.,-0.18200945304855));
#57403=CARTESIAN_POINT('Ctrl Pts',(4.06131670998589,1.,-0.185245370038948));
#57404=CARTESIAN_POINT('Ctrl Pts',(4.06828941192308,1.,-0.188519658060256));
#57405=CARTESIAN_POINT('Ctrl Pts',(4.07525439703137,1.,-0.191831928181081));
#57406=CARTESIAN_POINT('Ctrl Pts',(4.08221124060385,1.,-0.195181806054714));
#57407=CARTESIAN_POINT('Ctrl Pts',(4.08915953359753,1.,-0.198568934800811));
#57408=CARTESIAN_POINT('Ctrl Pts',(4.09609903751912,1.,-0.201992979049985));
#57409=CARTESIAN_POINT('Ctrl Pts',(4.10302969965374,1.,-0.205453622198233));
#57410=CARTESIAN_POINT('Ctrl Pts',(4.10995157639026,1.,-0.208950559400172));
#57411=CARTESIAN_POINT('Ctrl Pts',(4.11686478264545,1.,-0.212483491087068));
#57412=CARTESIAN_POINT('Ctrl Pts',(4.12376943492249,1.,-0.216052116898425));
#57413=CARTESIAN_POINT('Ctrl Pts',(4.13066558698156,1.,-0.219656126701852));
#57414=CARTESIAN_POINT('Ctrl Pts',(4.13755320553563,1.,-0.223295201038384));
#57415=CARTESIAN_POINT('Ctrl Pts',(4.14443220607733,1.,-0.226969025061244));
#57416=CARTESIAN_POINT('Ctrl Pts',(4.15130247435029,1.,-0.230677299028738));
#57417=CARTESIAN_POINT('Ctrl Pts',(4.1581638926525,1.,-0.234419749543143));
#57418=CARTESIAN_POINT('Ctrl Pts',(4.1650163665385,1.,-0.238196140933977));
#57419=CARTESIAN_POINT('Ctrl Pts',(4.17185984409533,1.,-0.242006283923912));
#57420=CARTESIAN_POINT('Ctrl Pts',(4.17869430192868,1.,-0.245850033418584));
#57421=CARTESIAN_POINT('Ctrl Pts',(4.18415464959491,1.,-0.248951836910964));
#57422=CARTESIAN_POINT('Ctrl Pts',(4.18824585244066,1.,-0.251293239837693));
#57423=CARTESIAN_POINT('Ctrl Pts',(4.19097151819241,1.,-0.252860861572566));
#57424=CARTESIAN_POINT('Ctrl Pts',(4.1923339003649,1.,-0.253646344052521));
#57425=CARTESIAN_POINT('Ctrl Pts',(4.18039834341342,-1.,-0.40530197431835));
#57426=CARTESIAN_POINT('Ctrl Pts',(4.18039834341342,1.,-0.40530197431835));
#57427=CARTESIAN_POINT('Ctrl Pts',(4.17892985789908,-1.,-0.405864662679631));
#57428=CARTESIAN_POINT('Ctrl Pts',(4.17892985789908,1.,-0.405864662679631));
#57429=CARTESIAN_POINT('Ctrl Pts',(4.17599251955585,-1.,-0.406986596326603));
#57430=CARTESIAN_POINT('Ctrl Pts',(4.17599251955585,1.,-0.406986596326603));
#57431=CARTESIAN_POINT('Ctrl Pts',(4.17158541009947,-1.,-0.408659167570153));
#57432=CARTESIAN_POINT('Ctrl Pts',(4.17158541009947,1.,-0.408659167570153));
#57433=CARTESIAN_POINT('Ctrl Pts',(4.16570705940731,-1.,-0.410868596148614));
#57434=CARTESIAN_POINT('Ctrl Pts',(4.16570705940731,1.,-0.410868596148614));
#57435=CARTESIAN_POINT('Ctrl Pts',(4.1583554501909,-1.,-0.413595877953269));
#57436=CARTESIAN_POINT('Ctrl Pts',(4.1583554501909,1.,-0.413595877953269));
#57437=CARTESIAN_POINT('Ctrl Pts',(4.15100018950989,-1.,-0.416288556008986));
#57438=CARTESIAN_POINT('Ctrl Pts',(4.15100018950989,1.,-0.416288556008986));
#57439=CARTESIAN_POINT('Ctrl Pts',(4.14364132317223,-1.,-0.4189464906678));
#57440=CARTESIAN_POINT('Ctrl Pts',(4.14364132317223,1.,-0.4189464906678));
#57441=CARTESIAN_POINT('Ctrl Pts',(4.13627893206433,-1.,-0.421569503103971));
#57442=CARTESIAN_POINT('Ctrl Pts',(4.13627893206433,1.,-0.421569503103971));
#57443=CARTESIAN_POINT('Ctrl Pts',(4.1289131463371,-1.,-0.424157375323155));
#57444=CARTESIAN_POINT('Ctrl Pts',(4.1289131463371,1.,-0.424157375323155));
#57445=CARTESIAN_POINT('Ctrl Pts',(4.1215441250121,-1.,-0.426709855706243));
#57446=CARTESIAN_POINT('Ctrl Pts',(4.1215441250121,1.,-0.426709855706243));
#57447=CARTESIAN_POINT('Ctrl Pts',(4.1141720278277,-1.,-0.429226666075373));
#57448=CARTESIAN_POINT('Ctrl Pts',(4.1141720278277,1.,-0.429226666075373));
#57449=CARTESIAN_POINT('Ctrl Pts',(4.10679698750219,-1.,-0.431707508679772));
#57450=CARTESIAN_POINT('Ctrl Pts',(4.10679698750219,1.,-0.431707508679772));
#57451=CARTESIAN_POINT('Ctrl Pts',(4.09941908688567,-1.,-0.434152073200643));
#57452=CARTESIAN_POINT('Ctrl Pts',(4.09941908688567,1.,-0.434152073200643));
#57453=CARTESIAN_POINT('Ctrl Pts',(4.09203832139439,-1.,-0.436560044913814));
#57454=CARTESIAN_POINT('Ctrl Pts',(4.09203832139439,1.,-0.436560044913814));
#57455=CARTESIAN_POINT('Ctrl Pts',(4.08465462294625,-1.,-0.438931108931614));
#57456=CARTESIAN_POINT('Ctrl Pts',(4.08465462294625,1.,-0.438931108931614));
#57457=CARTESIAN_POINT('Ctrl Pts',(4.07726792490256,-1.,-0.441264951396587));
#57458=CARTESIAN_POINT('Ctrl Pts',(4.07726792490256,1.,-0.441264951396587));
#57459=CARTESIAN_POINT('Ctrl Pts',(4.0698782192577,-1.,-0.443561262395408));
#57460=CARTESIAN_POINT('Ctrl Pts',(4.0698782192577,1.,-0.443561262395408));
#57461=CARTESIAN_POINT('Ctrl Pts',(4.06248560760596,-1.,-0.445819737468478));
#57462=CARTESIAN_POINT('Ctrl Pts',(4.06248560760596,1.,-0.445819737468478));
#57463=CARTESIAN_POINT('Ctrl Pts',(4.05509037796815,-1.,-0.448040082683977));
#57464=CARTESIAN_POINT('Ctrl Pts',(4.05509037796815,1.,-0.448040082683977));
#57465=CARTESIAN_POINT('Ctrl Pts',(4.0476929901797,-1.,-0.450222009543774));
#57466=CARTESIAN_POINT('Ctrl Pts',(4.0476929901797,1.,-0.450222009543774));
#57467=CARTESIAN_POINT('Ctrl Pts',(4.0402939222793,-1.,-0.452365214748779));
#57468=CARTESIAN_POINT('Ctrl Pts',(4.0402939222793,1.,-0.452365214748779));
#57469=CARTESIAN_POINT('Ctrl Pts',(4.03289354362745,-1.,-0.454469363020496));
#57470=CARTESIAN_POINT('Ctrl Pts',(4.03289354362745,1.,-0.454469363020496));
#57471=CARTESIAN_POINT('Ctrl Pts',(4.02549199038414,-1.,-0.456534070784968));
#57472=CARTESIAN_POINT('Ctrl Pts',(4.02549199038414,1.,-0.456534070784968));
#57473=CARTESIAN_POINT('Ctrl Pts',(4.01808900827647,-1.,-0.458558885637001));
#57474=CARTESIAN_POINT('Ctrl Pts',(4.01808900827647,1.,-0.458558885637001));
#57475=CARTESIAN_POINT('Ctrl Pts',(4.01068390573469,-1.,-0.460543280768577));
#57476=CARTESIAN_POINT('Ctrl Pts',(4.01068390573469,1.,-0.460543280768577));
#57477=CARTESIAN_POINT('Ctrl Pts',(4.00327590659129,-1.,-0.462486702616252));
#57478=CARTESIAN_POINT('Ctrl Pts',(4.00327590659129,1.,-0.462486702616252));
#57479=CARTESIAN_POINT('Ctrl Pts',(3.99586444320134,-1.,-0.464388610938995));
#57480=CARTESIAN_POINT('Ctrl Pts',(3.99586444320134,1.,-0.464388610938995));
#57481=CARTESIAN_POINT('Ctrl Pts',(3.98844946363258,-1.,-0.466248520883035));
#57482=CARTESIAN_POINT('Ctrl Pts',(3.98844946363258,1.,-0.466248520883035));
#57483=CARTESIAN_POINT('Ctrl Pts',(3.98103175589349,-1.,-0.46806604792014));
#57484=CARTESIAN_POINT('Ctrl Pts',(3.98103175589349,1.,-0.46806604792014));
#57485=CARTESIAN_POINT('Ctrl Pts',(3.97361320212413,-1.,-0.469840942829878));
#57486=CARTESIAN_POINT('Ctrl Pts',(3.97361320212413,1.,-0.469840942829878));
#57487=CARTESIAN_POINT('Ctrl Pts',(3.96619600864626,-1.,-0.471572978413494));
#57488=CARTESIAN_POINT('Ctrl Pts',(3.96619600864626,1.,-0.471572978413494));
#57489=CARTESIAN_POINT('Ctrl Pts',(3.95878201038332,-1.,-0.473261847236296));
#57490=CARTESIAN_POINT('Ctrl Pts',(3.95878201038332,1.,-0.473261847236296));
#57491=CARTESIAN_POINT('Ctrl Pts',(3.95137192932898,-1.,-0.474907053021791));
#57492=CARTESIAN_POINT('Ctrl Pts',(3.95137192932898,1.,-0.474907053021791));
#57493=CARTESIAN_POINT('Ctrl Pts',(3.94396469119385,-1.,-0.476507810658535));
#57494=CARTESIAN_POINT('Ctrl Pts',(3.94396469119385,1.,-0.476507810658535));
#57495=CARTESIAN_POINT('Ctrl Pts',(3.93655660689819,-1.,-0.478062927140957));
#57496=CARTESIAN_POINT('Ctrl Pts',(3.93655660689819,1.,-0.478062927140957));
#57497=CARTESIAN_POINT('Ctrl Pts',(3.92914297392067,-1.,-0.479571028525566));
#57498=CARTESIAN_POINT('Ctrl Pts',(3.92914297392067,1.,-0.479571028525566));
#57499=CARTESIAN_POINT('Ctrl Pts',(3.92171976072334,-1.,-0.481030798910735));
#57500=CARTESIAN_POINT('Ctrl Pts',(3.92171976072334,1.,-0.481030798910735));
#57501=CARTESIAN_POINT('Ctrl Pts',(3.91428536373749,-1.,-0.482441230340709));
#57502=CARTESIAN_POINT('Ctrl Pts',(3.91428536373749,1.,-0.482441230340709));
#57503=CARTESIAN_POINT('Ctrl Pts',(3.90684210358063,-1.,-0.483801835089161));
#57504=CARTESIAN_POINT('Ctrl Pts',(3.90684210358063,1.,-0.483801835089161));
#57505=CARTESIAN_POINT('Ctrl Pts',(3.89939844658529,-1.,-0.485112963522246));
#57506=CARTESIAN_POINT('Ctrl Pts',(3.89939844658529,1.,-0.485112963522246));
#57507=CARTESIAN_POINT('Ctrl Pts',(3.89196582437574,-1.,-0.486375337854134));
#57508=CARTESIAN_POINT('Ctrl Pts',(3.89196582437574,1.,-0.486375337854134));
#57509=CARTESIAN_POINT('Ctrl Pts',(3.88455453328156,-1.,-0.487589452275179));
#57510=CARTESIAN_POINT('Ctrl Pts',(3.88455453328156,1.,-0.487589452275179));
#57511=CARTESIAN_POINT('Ctrl Pts',(3.87716963231115,-1.,-0.488754973798281));
#57512=CARTESIAN_POINT('Ctrl Pts',(3.87716963231115,1.,-0.488754973798281));
#57513=CARTESIAN_POINT('Ctrl Pts',(3.86980755613694,-1.,-0.4898702457049));
#57514=CARTESIAN_POINT('Ctrl Pts',(3.86980755613694,1.,-0.4898702457049));
#57515=CARTESIAN_POINT('Ctrl Pts',(3.86245057319215,-1.,-0.490931482170849));
#57516=CARTESIAN_POINT('Ctrl Pts',(3.86245057319215,1.,-0.490931482170849));
#57517=CARTESIAN_POINT('Ctrl Pts',(3.85507287020223,-1.,-0.49193363108376));
#57518=CARTESIAN_POINT('Ctrl Pts',(3.85507287020223,1.,-0.49193363108376));
#57519=CARTESIAN_POINT('Ctrl Pts',(3.84765051147965,-1.,-0.492871792414095));
#57520=CARTESIAN_POINT('Ctrl Pts',(3.84765051147965,1.,-0.492871792414095));
#57521=CARTESIAN_POINT('Ctrl Pts',(3.84017095578438,-1.,-0.493742574629117));
#57522=CARTESIAN_POINT('Ctrl Pts',(3.84017095578438,1.,-0.493742574629117));
#57523=CARTESIAN_POINT('Ctrl Pts',(3.8326409268245,-1.,-0.494545212256426));
#57524=CARTESIAN_POINT('Ctrl Pts',(3.8326409268245,1.,-0.494545212256426));
#57525=CARTESIAN_POINT('Ctrl Pts',(3.82509963594156,-1.,-0.495283458893903));
#57526=CARTESIAN_POINT('Ctrl Pts',(3.82509963594156,1.,-0.495283458893903));
#57527=CARTESIAN_POINT('Ctrl Pts',(3.81760756144099,-1.,-0.495963937875572));
#57528=CARTESIAN_POINT('Ctrl Pts',(3.81760756144099,1.,-0.495963937875572));
#57529=CARTESIAN_POINT('Ctrl Pts',(3.81022254090909,-1.,-0.496592643443789));
#57530=CARTESIAN_POINT('Ctrl Pts',(3.81022254090909,1.,-0.496592643443789));
#57531=CARTESIAN_POINT('Ctrl Pts',(3.80297788298545,-1.,-0.497171756201091));
#57532=CARTESIAN_POINT('Ctrl Pts',(3.80297788298545,1.,-0.497171756201091));
#57533=CARTESIAN_POINT('Ctrl Pts',(3.79586380669959,-1.,-0.497696892100581));
#57534=CARTESIAN_POINT('Ctrl Pts',(3.79586380669959,1.,-0.497696892100581));
#57535=CARTESIAN_POINT('Ctrl Pts',(3.78879701661152,-1.,-0.498152751800819));
#57536=CARTESIAN_POINT('Ctrl Pts',(3.78879701661152,1.,-0.498152751800819));
#57537=CARTESIAN_POINT('Ctrl Pts',(3.78163975337189,-1.,-0.498515471679379));
#57538=CARTESIAN_POINT('Ctrl Pts',(3.78163975337189,1.,-0.498515471679379));
#57539=CARTESIAN_POINT('Ctrl Pts',(3.77425499225089,-1.,-0.498759900365687));
#57540=CARTESIAN_POINT('Ctrl Pts',(3.77425499225089,1.,-0.498759900365687));
#57541=CARTESIAN_POINT('Ctrl Pts',(3.76655401191144,-1.,-0.498865792335185));
#57542=CARTESIAN_POINT('Ctrl Pts',(3.76655401191144,1.,-0.498865792335185));
#57543=CARTESIAN_POINT('Ctrl Pts',(3.75854082221127,-1.,-0.498823681615513));
#57544=CARTESIAN_POINT('Ctrl Pts',(3.75854082221127,1.,-0.498823681615513));
#57545=CARTESIAN_POINT('Ctrl Pts',(3.75037362168103,-1.,-0.498642802042929));
#57546=CARTESIAN_POINT('Ctrl Pts',(3.75037362168103,1.,-0.498642802042929));
#57547=CARTESIAN_POINT('Ctrl Pts',(3.74235701735109,-1.,-0.498350586058176));
#57548=CARTESIAN_POINT('Ctrl Pts',(3.74235701735109,1.,-0.498350586058176));
#57549=CARTESIAN_POINT('Ctrl Pts',(3.73486914372834,-1.,-0.497984209510496));
#57550=CARTESIAN_POINT('Ctrl Pts',(3.73486914372834,1.,-0.497984209510496));
#57551=CARTESIAN_POINT('Ctrl Pts',(3.72830430904794,-1.,-0.49758406715328));
#57552=CARTESIAN_POINT('Ctrl Pts',(3.72830430904794,1.,-0.49758406715328));
#57553=CARTESIAN_POINT('Ctrl Pts',(3.72301489774241,-1.,-0.497187079575795));
#57554=CARTESIAN_POINT('Ctrl Pts',(3.72301489774241,1.,-0.497187079575795));
#57555=CARTESIAN_POINT('Ctrl Pts',(3.71923995965807,-1.,-0.496818574419989));
#57556=CARTESIAN_POINT('Ctrl Pts',(3.71923995965807,1.,-0.496818574419989));
#57557=CARTESIAN_POINT('Ctrl Pts',(3.71752134136931,-1.,-0.496556137603856));
#57558=CARTESIAN_POINT('Ctrl Pts',(3.71752134136931,1.,-0.496556137603856));
#57559=CARTESIAN_POINT('Ctrl Pts',(3.71698153685229,-1.,-0.496379397992182));
#57560=CARTESIAN_POINT('Ctrl Pts',(3.71698153685229,1.,-0.496379397992182));
#57561=CARTESIAN_POINT('Ctrl Pts',(3.71695438995598,-1.,-0.496270484166233));
#57562=CARTESIAN_POINT('Ctrl Pts',(3.71695438995598,1.,-0.496270484166233));
#57563=CARTESIAN_POINT('Ctrl Pts',(3.71702400346349,-1.,-0.496218256089212));
#57564=CARTESIAN_POINT('Ctrl Pts',(3.71702400346349,1.,-0.496218256089212));
#57565=CARTESIAN_POINT('',(4.18039834341342,1.,-0.40530197431835));
#57566=CARTESIAN_POINT('Ctrl Pts',(4.18039834341342,1.,-0.40530197431835));
#57567=CARTESIAN_POINT('Ctrl Pts',(4.17892985789908,1.,-0.405864662679631));
#57568=CARTESIAN_POINT('Ctrl Pts',(4.17599251955585,1.,-0.406986596326603));
#57569=CARTESIAN_POINT('Ctrl Pts',(4.17158541009947,1.,-0.408659167570153));
#57570=CARTESIAN_POINT('Ctrl Pts',(4.16570705940731,1.,-0.410868596148614));
#57571=CARTESIAN_POINT('Ctrl Pts',(4.1583554501909,1.,-0.413595877953269));
#57572=CARTESIAN_POINT('Ctrl Pts',(4.15100018950989,1.,-0.416288556008986));
#57573=CARTESIAN_POINT('Ctrl Pts',(4.14364132317223,1.,-0.4189464906678));
#57574=CARTESIAN_POINT('Ctrl Pts',(4.13627893206433,1.,-0.421569503103971));
#57575=CARTESIAN_POINT('Ctrl Pts',(4.1289131463371,1.,-0.424157375323155));
#57576=CARTESIAN_POINT('Ctrl Pts',(4.1215441250121,1.,-0.426709855706243));
#57577=CARTESIAN_POINT('Ctrl Pts',(4.1141720278277,1.,-0.429226666075373));
#57578=CARTESIAN_POINT('Ctrl Pts',(4.10679698750219,1.,-0.431707508679772));
#57579=CARTESIAN_POINT('Ctrl Pts',(4.09941908688567,1.,-0.434152073200643));
#57580=CARTESIAN_POINT('Ctrl Pts',(4.09203832139439,1.,-0.436560044913814));
#57581=CARTESIAN_POINT('Ctrl Pts',(4.08465462294625,1.,-0.438931108931614));
#57582=CARTESIAN_POINT('Ctrl Pts',(4.07726792490256,1.,-0.441264951396587));
#57583=CARTESIAN_POINT('Ctrl Pts',(4.0698782192577,1.,-0.443561262395408));
#57584=CARTESIAN_POINT('Ctrl Pts',(4.06248560760596,1.,-0.445819737468478));
#57585=CARTESIAN_POINT('Ctrl Pts',(4.05509037796815,1.,-0.448040082683977));
#57586=CARTESIAN_POINT('Ctrl Pts',(4.0476929901797,1.,-0.450222009543774));
#57587=CARTESIAN_POINT('Ctrl Pts',(4.0402939222793,1.,-0.452365214748779));
#57588=CARTESIAN_POINT('Ctrl Pts',(4.03289354362745,1.,-0.454469363020496));
#57589=CARTESIAN_POINT('Ctrl Pts',(4.02549199038414,1.,-0.456534070784968));
#57590=CARTESIAN_POINT('Ctrl Pts',(4.01808900827647,1.,-0.458558885637001));
#57591=CARTESIAN_POINT('Ctrl Pts',(4.01068390573469,1.,-0.460543280768577));
#57592=CARTESIAN_POINT('Ctrl Pts',(4.00327590659129,1.,-0.462486702616252));
#57593=CARTESIAN_POINT('Ctrl Pts',(3.99586444320134,1.,-0.464388610938995));
#57594=CARTESIAN_POINT('Ctrl Pts',(3.98844946363258,1.,-0.466248520883035));
#57595=CARTESIAN_POINT('Ctrl Pts',(3.98103175589349,1.,-0.46806604792014));
#57596=CARTESIAN_POINT('Ctrl Pts',(3.97361320212413,1.,-0.469840942829878));
#57597=CARTESIAN_POINT('Ctrl Pts',(3.96619600864626,1.,-0.471572978413494));
#57598=CARTESIAN_POINT('Ctrl Pts',(3.95878201038332,1.,-0.473261847236296));
#57599=CARTESIAN_POINT('Ctrl Pts',(3.95137192932898,1.,-0.474907053021791));
#57600=CARTESIAN_POINT('Ctrl Pts',(3.94396469119385,1.,-0.476507810658535));
#57601=CARTESIAN_POINT('Ctrl Pts',(3.93655660689819,1.,-0.478062927140957));
#57602=CARTESIAN_POINT('Ctrl Pts',(3.92914297392067,1.,-0.479571028525566));
#57603=CARTESIAN_POINT('Ctrl Pts',(3.92171976072334,1.,-0.481030798910735));
#57604=CARTESIAN_POINT('Ctrl Pts',(3.91428536373749,1.,-0.482441230340709));
#57605=CARTESIAN_POINT('Ctrl Pts',(3.90684210358063,1.,-0.483801835089161));
#57606=CARTESIAN_POINT('Ctrl Pts',(3.89939844658529,1.,-0.485112963522246));
#57607=CARTESIAN_POINT('Ctrl Pts',(3.89196582437574,1.,-0.486375337854134));
#57608=CARTESIAN_POINT('Ctrl Pts',(3.88455453328156,1.,-0.487589452275179));
#57609=CARTESIAN_POINT('Ctrl Pts',(3.87716963231115,1.,-0.488754973798281));
#57610=CARTESIAN_POINT('Ctrl Pts',(3.86980755613694,1.,-0.4898702457049));
#57611=CARTESIAN_POINT('Ctrl Pts',(3.86245057319215,1.,-0.490931482170849));
#57612=CARTESIAN_POINT('Ctrl Pts',(3.85507287020223,1.,-0.49193363108376));
#57613=CARTESIAN_POINT('Ctrl Pts',(3.84765051147965,1.,-0.492871792414095));
#57614=CARTESIAN_POINT('Ctrl Pts',(3.84017095578438,1.,-0.493742574629117));
#57615=CARTESIAN_POINT('Ctrl Pts',(3.8326409268245,1.,-0.494545212256426));
#57616=CARTESIAN_POINT('Ctrl Pts',(3.82509963594156,1.,-0.495283458893903));
#57617=CARTESIAN_POINT('Ctrl Pts',(3.81760756144099,1.,-0.495963937875572));
#57618=CARTESIAN_POINT('Ctrl Pts',(3.81022254090909,1.,-0.496592643443789));
#57619=CARTESIAN_POINT('Ctrl Pts',(3.80297788298545,1.,-0.497171756201091));
#57620=CARTESIAN_POINT('Ctrl Pts',(3.79586380669959,1.,-0.497696892100581));
#57621=CARTESIAN_POINT('Ctrl Pts',(3.78879701661152,1.,-0.498152751800819));
#57622=CARTESIAN_POINT('Ctrl Pts',(3.78163975337189,1.,-0.498515471679379));
#57623=CARTESIAN_POINT('Ctrl Pts',(3.77425499225089,1.,-0.498759900365687));
#57624=CARTESIAN_POINT('Ctrl Pts',(3.76655401191144,1.,-0.498865792335185));
#57625=CARTESIAN_POINT('Ctrl Pts',(3.75854082221127,1.,-0.498823681615513));
#57626=CARTESIAN_POINT('Ctrl Pts',(3.75037362168103,1.,-0.498642802042929));
#57627=CARTESIAN_POINT('Ctrl Pts',(3.74235701735109,1.,-0.498350586058176));
#57628=CARTESIAN_POINT('Ctrl Pts',(3.73486914372834,1.,-0.497984209510496));
#57629=CARTESIAN_POINT('Ctrl Pts',(3.72830430904794,1.,-0.49758406715328));
#57630=CARTESIAN_POINT('Ctrl Pts',(3.72301489774241,1.,-0.497187079575795));
#57631=CARTESIAN_POINT('Ctrl Pts',(3.7195232082259,1.,-0.496846224822535));
#57632=CARTESIAN_POINT('Ctrl Pts',(3.71785517607694,1.,-0.496605651526314));
#57633=CARTESIAN_POINT('Ctrl Pts',(3.71721917030465,1.,-0.496446644158827));
#57634=CARTESIAN_POINT('Ctrl Pts',(3.71704500630521,1.,-0.496354087925646));
#57635=CARTESIAN_POINT('Ctrl Pts',(3.71701050416802,1.,-0.496319364829374));
#57636=CARTESIAN_POINT('',(4.18039834341342,0.,-0.40530197431835));
#57637=CARTESIAN_POINT('Origin',(4.1923339003649,0.,-0.253646344052521));
#57638=CARTESIAN_POINT('',(4.18039834341342,1.,-0.40530197431835));
#57639=CARTESIAN_POINT('Origin',(0.,1.,0.));
#57640=CARTESIAN_POINT('Origin',(0.,1.,0.));
#57641=CARTESIAN_POINT('Origin',(0.,0.,0.));
#57642=CARTESIAN_POINT('',(0.,0.,0.));
#57643=CARTESIAN_POINT('Origin',(0.0866025403784439,-0.4,-0.15));
#57644=CARTESIAN_POINT('',(0.173205080756888,-0.4,0.));
#57645=CARTESIAN_POINT('',(0.0866025403784439,-0.4,-0.15));
#57646=CARTESIAN_POINT('',(0.173205080756888,-0.4,0.));
#57647=CARTESIAN_POINT('',(0.0866025403784439,-0.64,-0.15));
#57648=CARTESIAN_POINT('',(0.0866025403784439,-0.4,-0.15));
#57649=CARTESIAN_POINT('',(0.173205080756888,-0.64,0.));
#57650=CARTESIAN_POINT('',(0.173205080756888,-0.64,0.));
#57651=CARTESIAN_POINT('',(0.173205080756888,-0.4,0.));
#57652=CARTESIAN_POINT('Origin',(-0.0866025403784438,-0.4,-0.15));
#57653=CARTESIAN_POINT('',(-0.0866025403784438,-0.4,-0.15));
#57654=CARTESIAN_POINT('',(0.0866025403784439,-0.4,-0.15));
#57655=CARTESIAN_POINT('',(-0.0866025403784438,-0.64,-0.15));
#57656=CARTESIAN_POINT('',(-0.0866025403784438,-0.4,-0.15));
#57657=CARTESIAN_POINT('',(0.0866025403784439,-0.64,-0.15));
#57658=CARTESIAN_POINT('Origin',(-0.173205080756888,-0.4,-2.77555756156289E-17));
#57659=CARTESIAN_POINT('',(-0.173205080756888,-0.4,-2.12115047744981E-17));
#57660=CARTESIAN_POINT('',(-0.0866025403784438,-0.4,-0.15));
#57661=CARTESIAN_POINT('',(-0.173205080756888,-0.64,-2.77555756156289E-17));
#57662=CARTESIAN_POINT('',(-0.173205080756888,-0.4,-2.12115047744981E-17));
#57663=CARTESIAN_POINT('',(-0.0866025403784438,-0.64,-0.15));
#57664=CARTESIAN_POINT('Origin',(-0.0866025403784439,-0.4,0.15));
#57665=CARTESIAN_POINT('',(-0.0866025403784439,-0.4,0.15));
#57666=CARTESIAN_POINT('',(-0.173205080756888,-0.4,-2.12115047744981E-17));
#57667=CARTESIAN_POINT('',(-0.0866025403784439,-0.64,0.15));
#57668=CARTESIAN_POINT('',(-0.0866025403784439,-0.4,0.15));
#57669=CARTESIAN_POINT('',(-0.173205080756888,-0.64,-2.12115047744981E-17));
#57670=CARTESIAN_POINT('Origin',(0.0866025403784439,-0.4,0.15));
#57671=CARTESIAN_POINT('',(0.0866025403784439,-0.4,0.15));
#57672=CARTESIAN_POINT('',(-0.0866025403784439,-0.4,0.15));
#57673=CARTESIAN_POINT('',(0.0866025403784439,-0.64,0.15));
#57674=CARTESIAN_POINT('',(0.0866025403784439,-0.4,0.15));
#57675=CARTESIAN_POINT('',(-0.0866025403784439,-0.64,0.15));
#57676=CARTESIAN_POINT('Origin',(0.173205080756888,-0.4,0.));
#57677=CARTESIAN_POINT('',(0.0866025403784439,-0.4,0.15));
#57678=CARTESIAN_POINT('',(0.0866025403784439,-0.64,0.15));
#57679=CARTESIAN_POINT('Origin',(0.,-0.4,-2.77555756156289E-17));
#57680=CARTESIAN_POINT('Origin',(0.,-0.64,-2.77555756156289E-17));
#57681=CARTESIAN_POINT('Origin',(0.,-1.,0.));
#57682=CARTESIAN_POINT('',(-0.1954,-1.,2.39295984553393E-17));
#57683=CARTESIAN_POINT('Origin',(0.,-1.,0.));
#57684=CARTESIAN_POINT('Origin',(0.3,0.4,0.));
#57685=CARTESIAN_POINT('',(-0.3,0.4,-3.67394039744206E-17));
#57686=CARTESIAN_POINT('Origin',(0.,0.4,0.));
#57687=CARTESIAN_POINT('Origin',(0.,0.375,0.));
#57688=CARTESIAN_POINT('',(-0.35,0.35,-4.28626379701573E-17));
#57689=CARTESIAN_POINT('Origin',(0.,0.35,0.));
#57690=CARTESIAN_POINT('',(-0.325,0.375,-3.9801020972289E-17));
#57691=CARTESIAN_POINT('Origin',(0.,0.19,0.));
#57692=CARTESIAN_POINT('',(-0.35,0.03,-4.28626379701574E-17));
#57693=CARTESIAN_POINT('Origin',(0.,0.03,0.));
#57694=CARTESIAN_POINT('',(-0.35,0.19,-4.28626379701574E-17));
#57695=CARTESIAN_POINT('Origin',(0.,0.0149999999999999,0.));
#57696=CARTESIAN_POINT('',(-0.32,-3.29597460435593E-17,-3.91886975727153E-17));
#57697=CARTESIAN_POINT('Origin',(0.,0.,0.));
#57698=CARTESIAN_POINT('',(-0.335,0.0149999999999999,-4.10256677714363E-17));
#57699=CARTESIAN_POINT('Origin',(0.22,0.,0.));
#57700=CARTESIAN_POINT('',(-0.22,-6.93889390390723E-18,-2.69422295812418E-17));
#57701=CARTESIAN_POINT('Origin',(0.,0.,0.));
#57702=CARTESIAN_POINT('Origin',(0.,-0.02,0.));
#57703=CARTESIAN_POINT('',(-0.1954,-0.0492,2.39295984553393E-17));
#57704=CARTESIAN_POINT('Origin',(0.,-0.0492,0.));
#57705=CARTESIAN_POINT('',(-0.21,-0.02,-2.57175827820944E-17));
#57706=CARTESIAN_POINT('Origin',(0.,-0.8,0.));
#57707=CARTESIAN_POINT('',(-0.1954,-0.8,-2.39295984553393E-17));
#57708=CARTESIAN_POINT('',(0.,0.,0.));
#57709=CARTESIAN_POINT('',(0.,0.,0.));
#57710=CARTESIAN_POINT('',(0.,0.,0.));
#57711=CARTESIAN_POINT('',(0.,0.,0.));
#57712=CARTESIAN_POINT('',(0.,0.,0.));
#57713=CARTESIAN_POINT('',(0.,0.,0.));
#57714=CARTESIAN_POINT('',(0.,0.,0.));
#57715=CARTESIAN_POINT('',(0.,0.,0.));
#57716=CARTESIAN_POINT('',(0.,0.,0.));
#57717=CARTESIAN_POINT('',(0.,0.,0.));
#57718=CARTESIAN_POINT('',(0.,0.,0.));
#57719=CARTESIAN_POINT('',(-1.5,6.,0.));
#57720=CARTESIAN_POINT('',(0.5,6.,0.97));
#57721=CARTESIAN_POINT('',(6.5,6.,0.97));
#57722=CARTESIAN_POINT('',(12.5,6.,0.97));
#57723=CARTESIAN_POINT('',(18.5,6.,0.97));
#57724=CARTESIAN_POINT('',(1.76776695296637,1.76776695296637,0.8));
#57725=CARTESIAN_POINT('',(-1.76776695296637,1.76776695296637,0.8));
#57726=CARTESIAN_POINT('',(-1.76776695296637,-1.76776695296637,0.8));
#57727=CARTESIAN_POINT('',(1.76776695296637,-1.76776695296637,0.8));
#57728=CARTESIAN_POINT('',(0.,0.,6.5));
#57729=CARTESIAN_POINT('',(0.,0.,8.5));
#57730=CARTESIAN_POINT('',(1.4142135623731,1.41421356237309,9.6));
#57731=CARTESIAN_POINT('',(-1.41421356237309,1.4142135623731,9.6));
#57732=CARTESIAN_POINT('',(-1.4142135623731,-1.41421356237309,9.6));
#57733=CARTESIAN_POINT('',(1.41421356237309,-1.4142135623731,9.6));
#57734=CARTESIAN_POINT('',(12.8131727983645,9.81317279836453,0.8));
#57735=CARTESIAN_POINT('',(11.1868272016355,9.81317279836453,0.8));
#57736=CARTESIAN_POINT('',(11.1868272016355,8.18682720163547,0.8));
#57737=CARTESIAN_POINT('',(12.8131727983645,8.18682720163547,0.8));
#57738=CARTESIAN_POINT('',(13.2,9.,12.));
#57739=CARTESIAN_POINT('',(0.,0.,0.));
#57740=CARTESIAN_POINT('',(0.,0.,0.));
#57741=CARTESIAN_POINT('',(0.,0.,0.));
#57742=CARTESIAN_POINT('',(0.,0.,0.));
#57743=CARTESIAN_POINT('',(0.,0.,0.));
#57744=CARTESIAN_POINT('',(6.,6.,0.));
#57745=CARTESIAN_POINT('',(4.5,4.1,3.2));
#57746=CARTESIAN_POINT('',(4.5,7.9,3.2));
#57747=CARTESIAN_POINT('',(7.5,4.1,3.2));
#57748=CARTESIAN_POINT('',(7.5,7.9,3.2));
#57749=CARTESIAN_POINT('',(9.5,7.8,1.1));
#57750=CARTESIAN_POINT('',(8.1920310216783,2.1920310216783,4.));
#57751=CARTESIAN_POINT('',(3.8079689783217,2.1920310216783,4.));
#57752=CARTESIAN_POINT('',(3.8079689783217,-2.1920310216783,4.));
#57753=CARTESIAN_POINT('',(8.1920310216783,-2.1920310216783,4.));
#57754=CARTESIAN_POINT('',(6.,0.,6.5));
#57755=CARTESIAN_POINT('',(6.,0.,8.5));
#57756=CARTESIAN_POINT('',(7.94454364826301,1.94454364826301,9.6));
#57757=CARTESIAN_POINT('',(4.05545635173699,1.94454364826301,9.6));
#57758=CARTESIAN_POINT('',(4.05545635173699,-1.94454364826301,9.6));
#57759=CARTESIAN_POINT('',(7.944543648263,-1.94454364826301,9.6));
#57760=CARTESIAN_POINT('',(0.,0.,0.));
#57761=CARTESIAN_POINT('',(0.,0.,0.));
#57762=CARTESIAN_POINT('',(0.,0.,0.));
#57763=CARTESIAN_POINT('',(0.,0.,0.));
#57764=CARTESIAN_POINT('',(0.,0.,0.));
#57765=CARTESIAN_POINT('',(0.,0.,0.));
#57766=CARTESIAN_POINT('',(0.,0.,0.));
#57767=CARTESIAN_POINT('',(1.,0.,5.4));
#57768=CARTESIAN_POINT('',(0.,0.,12.));
#57769=CARTESIAN_POINT('',(0.,2.22044604925031E-16,15.2));
#57770=CARTESIAN_POINT('',(0.,0.,0.));
#57771=CARTESIAN_POINT('',(0.,0.,0.));
#57772=CARTESIAN_POINT('',(0.,0.,0.));
#57773=CARTESIAN_POINT('',(0.,0.,0.));
#57774=CARTESIAN_POINT('',(0.,0.,0.));
#57775=CARTESIAN_POINT('',(0.,0.,0.));
#57776=CARTESIAN_POINT('',(7.4,0.,5.4));
#57777=CARTESIAN_POINT('',(6.,0.,12.));
#57778=CARTESIAN_POINT('',(6.,2.22044604925031E-16,15.2));
#57779=CARTESIAN_POINT('',(0.,0.,0.));
#57780=CARTESIAN_POINT('',(0.,0.,0.));
#57781=CARTESIAN_POINT('',(0.,0.,0.));
#57782=CARTESIAN_POINT('',(0.,0.,0.));
#57783=UNCERTAINTY_MEASURE_WITH_UNIT(LENGTH_MEASURE(0.001),#57901,
'DISTANCE_ACCURACY_VALUE',
'Maximum model space distance between geometric entities at asserted c
onnectivities');
#57784=UNCERTAINTY_MEASURE_WITH_UNIT(LENGTH_MEASURE(0.001),#57901,
'DISTANCE_ACCURACY_VALUE',
'Maximum model space distance between geometric entities at asserted c
onnectivities');
#57785=UNCERTAINTY_MEASURE_WITH_UNIT(LENGTH_MEASURE(0.001),#57901,
'DISTANCE_ACCURACY_VALUE',
'Maximum model space distance between geometric entities at asserted c
onnectivities');
#57786=UNCERTAINTY_MEASURE_WITH_UNIT(LENGTH_MEASURE(0.001),#57901,
'DISTANCE_ACCURACY_VALUE',
'Maximum model space distance between geometric entities at asserted c
onnectivities');
#57787=UNCERTAINTY_MEASURE_WITH_UNIT(LENGTH_MEASURE(0.001),#57901,
'DISTANCE_ACCURACY_VALUE',
'Maximum model space distance between geometric entities at asserted c
onnectivities');
#57788=UNCERTAINTY_MEASURE_WITH_UNIT(LENGTH_MEASURE(0.001),#57901,
'DISTANCE_ACCURACY_VALUE',
'Maximum model space distance between geometric entities at asserted c
onnectivities');
#57789=UNCERTAINTY_MEASURE_WITH_UNIT(LENGTH_MEASURE(0.001),#57901,
'DISTANCE_ACCURACY_VALUE',
'Maximum model space distance between geometric entities at asserted c
onnectivities');
#57790=UNCERTAINTY_MEASURE_WITH_UNIT(LENGTH_MEASURE(0.001),#57901,
'DISTANCE_ACCURACY_VALUE',
'Maximum model space distance between geometric entities at asserted c
onnectivities');
#57791=UNCERTAINTY_MEASURE_WITH_UNIT(LENGTH_MEASURE(0.001),#57901,
'DISTANCE_ACCURACY_VALUE',
'Maximum model space distance between geometric entities at asserted c
onnectivities');
#57792=UNCERTAINTY_MEASURE_WITH_UNIT(LENGTH_MEASURE(0.001),#57901,
'DISTANCE_ACCURACY_VALUE',
'Maximum model space distance between geometric entities at asserted c
onnectivities');
#57793=UNCERTAINTY_MEASURE_WITH_UNIT(LENGTH_MEASURE(0.001),#57901,
'DISTANCE_ACCURACY_VALUE',
'Maximum model space distance between geometric entities at asserted c
onnectivities');
#57794=UNCERTAINTY_MEASURE_WITH_UNIT(LENGTH_MEASURE(0.001),#57901,
'DISTANCE_ACCURACY_VALUE',
'Maximum model space distance between geometric entities at asserted c
onnectivities');
#57795=UNCERTAINTY_MEASURE_WITH_UNIT(LENGTH_MEASURE(0.001),#57901,
'DISTANCE_ACCURACY_VALUE',
'Maximum model space distance between geometric entities at asserted c
onnectivities');
#57796=UNCERTAINTY_MEASURE_WITH_UNIT(LENGTH_MEASURE(0.001),#57901,
'DISTANCE_ACCURACY_VALUE',
'Maximum model space distance between geometric entities at asserted c
onnectivities');
#57797=UNCERTAINTY_MEASURE_WITH_UNIT(LENGTH_MEASURE(0.001),#57901,
'DISTANCE_ACCURACY_VALUE',
'Maximum model space distance between geometric entities at asserted c
onnectivities');
#57798=UNCERTAINTY_MEASURE_WITH_UNIT(LENGTH_MEASURE(0.001),#57901,
'DISTANCE_ACCURACY_VALUE',
'Maximum model space distance between geometric entities at asserted c
onnectivities');
#57799=UNCERTAINTY_MEASURE_WITH_UNIT(LENGTH_MEASURE(0.001),#57901,
'DISTANCE_ACCURACY_VALUE',
'Maximum model space distance between geometric entities at asserted c
onnectivities');
#57800=UNCERTAINTY_MEASURE_WITH_UNIT(LENGTH_MEASURE(0.001),#57901,
'DISTANCE_ACCURACY_VALUE',
'Maximum model space distance between geometric entities at asserted c
onnectivities');
#57801=UNCERTAINTY_MEASURE_WITH_UNIT(LENGTH_MEASURE(0.001),#57901,
'DISTANCE_ACCURACY_VALUE',
'Maximum model space distance between geometric entities at asserted c
onnectivities');
#57802=UNCERTAINTY_MEASURE_WITH_UNIT(LENGTH_MEASURE(0.001),#57901,
'DISTANCE_ACCURACY_VALUE',
'Maximum model space distance between geometric entities at asserted c
onnectivities');
#57803=UNCERTAINTY_MEASURE_WITH_UNIT(LENGTH_MEASURE(0.001),#57901,
'DISTANCE_ACCURACY_VALUE',
'Maximum model space distance between geometric entities at asserted c
onnectivities');
#57804=UNCERTAINTY_MEASURE_WITH_UNIT(LENGTH_MEASURE(0.001),#57901,
'DISTANCE_ACCURACY_VALUE',
'Maximum model space distance between geometric entities at asserted c
onnectivities');
#57805=UNCERTAINTY_MEASURE_WITH_UNIT(LENGTH_MEASURE(0.001),#57901,
'DISTANCE_ACCURACY_VALUE',
'Maximum model space distance between geometric entities at asserted c
onnectivities');
#57806=UNCERTAINTY_MEASURE_WITH_UNIT(LENGTH_MEASURE(0.001),#57901,
'DISTANCE_ACCURACY_VALUE',
'Maximum model space distance between geometric entities at asserted c
onnectivities');
#57807=UNCERTAINTY_MEASURE_WITH_UNIT(LENGTH_MEASURE(0.001),#57901,
'DISTANCE_ACCURACY_VALUE',
'Maximum model space distance between geometric entities at asserted c
onnectivities');
#57808=UNCERTAINTY_MEASURE_WITH_UNIT(LENGTH_MEASURE(0.001),#57901,
'DISTANCE_ACCURACY_VALUE',
'Maximum model space distance between geometric entities at asserted c
onnectivities');
#57809=UNCERTAINTY_MEASURE_WITH_UNIT(LENGTH_MEASURE(0.001),#57901,
'DISTANCE_ACCURACY_VALUE',
'Maximum model space distance between geometric entities at asserted c
onnectivities');
#57810=UNCERTAINTY_MEASURE_WITH_UNIT(LENGTH_MEASURE(0.001),#57901,
'DISTANCE_ACCURACY_VALUE',
'Maximum model space distance between geometric entities at asserted c
onnectivities');
#57811=UNCERTAINTY_MEASURE_WITH_UNIT(LENGTH_MEASURE(0.001),#57901,
'DISTANCE_ACCURACY_VALUE',
'Maximum model space distance between geometric entities at asserted c
onnectivities');
#57812=UNCERTAINTY_MEASURE_WITH_UNIT(LENGTH_MEASURE(0.001),#57901,
'DISTANCE_ACCURACY_VALUE',
'Maximum model space distance between geometric entities at asserted c
onnectivities');
#57813=UNCERTAINTY_MEASURE_WITH_UNIT(LENGTH_MEASURE(0.001),#57901,
'DISTANCE_ACCURACY_VALUE',
'Maximum model space distance between geometric entities at asserted c
onnectivities');
#57814=UNCERTAINTY_MEASURE_WITH_UNIT(LENGTH_MEASURE(0.001),#57901,
'DISTANCE_ACCURACY_VALUE',
'Maximum model space distance between geometric entities at asserted c
onnectivities');
#57815=UNCERTAINTY_MEASURE_WITH_UNIT(LENGTH_MEASURE(0.001),#57901,
'DISTANCE_ACCURACY_VALUE',
'Maximum model space distance between geometric entities at asserted c
onnectivities');
#57816=UNCERTAINTY_MEASURE_WITH_UNIT(LENGTH_MEASURE(0.001),#57901,
'DISTANCE_ACCURACY_VALUE',
'Maximum model space distance between geometric entities at asserted c
onnectivities');
#57817=UNCERTAINTY_MEASURE_WITH_UNIT(LENGTH_MEASURE(0.001),#57901,
'DISTANCE_ACCURACY_VALUE',
'Maximum model space distance between geometric entities at asserted c
onnectivities');
#57818=UNCERTAINTY_MEASURE_WITH_UNIT(LENGTH_MEASURE(0.001),#57901,
'DISTANCE_ACCURACY_VALUE',
'Maximum model space distance between geometric entities at asserted c
onnectivities');
#57819=UNCERTAINTY_MEASURE_WITH_UNIT(LENGTH_MEASURE(0.001),#57901,
'DISTANCE_ACCURACY_VALUE',
'Maximum model space distance between geometric entities at asserted c
onnectivities');
#57820=UNCERTAINTY_MEASURE_WITH_UNIT(LENGTH_MEASURE(0.001),#57901,
'DISTANCE_ACCURACY_VALUE',
'Maximum model space distance between geometric entities at asserted c
onnectivities');
#57821=UNCERTAINTY_MEASURE_WITH_UNIT(LENGTH_MEASURE(0.001),#57901,
'DISTANCE_ACCURACY_VALUE',
'Maximum model space distance between geometric entities at asserted c
onnectivities');
#57822=UNCERTAINTY_MEASURE_WITH_UNIT(LENGTH_MEASURE(0.001),#57901,
'DISTANCE_ACCURACY_VALUE',
'Maximum model space distance between geometric entities at asserted c
onnectivities');
#57823=UNCERTAINTY_MEASURE_WITH_UNIT(LENGTH_MEASURE(0.001),#57901,
'DISTANCE_ACCURACY_VALUE',
'Maximum model space distance between geometric entities at asserted c
onnectivities');
#57824=UNCERTAINTY_MEASURE_WITH_UNIT(LENGTH_MEASURE(0.001),#57901,
'DISTANCE_ACCURACY_VALUE',
'Maximum model space distance between geometric entities at asserted c
onnectivities');
#57825=UNCERTAINTY_MEASURE_WITH_UNIT(LENGTH_MEASURE(0.001),#57901,
'DISTANCE_ACCURACY_VALUE',
'Maximum model space distance between geometric entities at asserted c
onnectivities');
#57826=UNCERTAINTY_MEASURE_WITH_UNIT(LENGTH_MEASURE(0.001),#57901,
'DISTANCE_ACCURACY_VALUE',
'Maximum model space distance between geometric entities at asserted c
onnectivities');
#57827=UNCERTAINTY_MEASURE_WITH_UNIT(LENGTH_MEASURE(0.001),#57901,
'DISTANCE_ACCURACY_VALUE',
'Maximum model space distance between geometric entities at asserted c
onnectivities');
#57828=UNCERTAINTY_MEASURE_WITH_UNIT(LENGTH_MEASURE(0.001),#57901,
'DISTANCE_ACCURACY_VALUE',
'Maximum model space distance between geometric entities at asserted c
onnectivities');
#57829=UNCERTAINTY_MEASURE_WITH_UNIT(LENGTH_MEASURE(0.001),#57901,
'DISTANCE_ACCURACY_VALUE',
'Maximum model space distance between geometric entities at asserted c
onnectivities');
#57830=UNCERTAINTY_MEASURE_WITH_UNIT(LENGTH_MEASURE(0.001),#57901,
'DISTANCE_ACCURACY_VALUE',
'Maximum model space distance between geometric entities at asserted c
onnectivities');
#57831=UNCERTAINTY_MEASURE_WITH_UNIT(LENGTH_MEASURE(0.001),#57901,
'DISTANCE_ACCURACY_VALUE',
'Maximum model space distance between geometric entities at asserted c
onnectivities');
#57832=UNCERTAINTY_MEASURE_WITH_UNIT(LENGTH_MEASURE(0.001),#57901,
'DISTANCE_ACCURACY_VALUE',
'Maximum model space distance between geometric entities at asserted c
onnectivities');
#57833=UNCERTAINTY_MEASURE_WITH_UNIT(LENGTH_MEASURE(0.001),#57901,
'DISTANCE_ACCURACY_VALUE',
'Maximum model space distance between geometric entities at asserted c
onnectivities');
#57834=UNCERTAINTY_MEASURE_WITH_UNIT(LENGTH_MEASURE(0.001),#57901,
'DISTANCE_ACCURACY_VALUE',
'Maximum model space distance between geometric entities at asserted c
onnectivities');
#57835=UNCERTAINTY_MEASURE_WITH_UNIT(LENGTH_MEASURE(0.001),#57901,
'DISTANCE_ACCURACY_VALUE',
'Maximum model space distance between geometric entities at asserted c
onnectivities');
#57836=UNCERTAINTY_MEASURE_WITH_UNIT(LENGTH_MEASURE(0.001),#57901,
'DISTANCE_ACCURACY_VALUE',
'Maximum model space distance between geometric entities at asserted c
onnectivities');
#57837=UNCERTAINTY_MEASURE_WITH_UNIT(LENGTH_MEASURE(0.001),#57901,
'DISTANCE_ACCURACY_VALUE',
'Maximum model space distance between geometric entities at asserted c
onnectivities');
#57838=UNCERTAINTY_MEASURE_WITH_UNIT(LENGTH_MEASURE(0.001),#57901,
'DISTANCE_ACCURACY_VALUE',
'Maximum model space distance between geometric entities at asserted c
onnectivities');
#57839=UNCERTAINTY_MEASURE_WITH_UNIT(LENGTH_MEASURE(0.001),#57901,
'DISTANCE_ACCURACY_VALUE',
'Maximum model space distance between geometric entities at asserted c
onnectivities');
#57840=UNCERTAINTY_MEASURE_WITH_UNIT(LENGTH_MEASURE(0.001),#57901,
'DISTANCE_ACCURACY_VALUE',
'Maximum model space distance between geometric entities at asserted c
onnectivities');
#57841=UNCERTAINTY_MEASURE_WITH_UNIT(LENGTH_MEASURE(0.001),#57901,
'DISTANCE_ACCURACY_VALUE',
'Maximum model space distance between geometric entities at asserted c
onnectivities');
#57842=(
GEOMETRIC_REPRESENTATION_CONTEXT(3)
GLOBAL_UNCERTAINTY_ASSIGNED_CONTEXT((#57783))
GLOBAL_UNIT_ASSIGNED_CONTEXT((#57901,#57903,#57904))
REPRESENTATION_CONTEXT('','3D')
);
#57843=(
GEOMETRIC_REPRESENTATION_CONTEXT(3)
GLOBAL_UNCERTAINTY_ASSIGNED_CONTEXT((#57784))
GLOBAL_UNIT_ASSIGNED_CONTEXT((#57901,#57903,#57904))
REPRESENTATION_CONTEXT('','3D')
);
#57844=(
GEOMETRIC_REPRESENTATION_CONTEXT(3)
GLOBAL_UNCERTAINTY_ASSIGNED_CONTEXT((#57785))
GLOBAL_UNIT_ASSIGNED_CONTEXT((#57901,#57903,#57904))
REPRESENTATION_CONTEXT('','3D')
);
#57845=(
GEOMETRIC_REPRESENTATION_CONTEXT(3)
GLOBAL_UNCERTAINTY_ASSIGNED_CONTEXT((#57786))
GLOBAL_UNIT_ASSIGNED_CONTEXT((#57901,#57903,#57904))
REPRESENTATION_CONTEXT('','3D')
);
#57846=(
GEOMETRIC_REPRESENTATION_CONTEXT(3)
GLOBAL_UNCERTAINTY_ASSIGNED_CONTEXT((#57787))
GLOBAL_UNIT_ASSIGNED_CONTEXT((#57901,#57903,#57904))
REPRESENTATION_CONTEXT('','3D')
);
#57847=(
GEOMETRIC_REPRESENTATION_CONTEXT(3)
GLOBAL_UNCERTAINTY_ASSIGNED_CONTEXT((#57788))
GLOBAL_UNIT_ASSIGNED_CONTEXT((#57901,#57903,#57904))
REPRESENTATION_CONTEXT('','3D')
);
#57848=(
GEOMETRIC_REPRESENTATION_CONTEXT(3)
GLOBAL_UNCERTAINTY_ASSIGNED_CONTEXT((#57789))
GLOBAL_UNIT_ASSIGNED_CONTEXT((#57901,#57903,#57904))
REPRESENTATION_CONTEXT('','3D')
);
#57849=(
GEOMETRIC_REPRESENTATION_CONTEXT(3)
GLOBAL_UNCERTAINTY_ASSIGNED_CONTEXT((#57790))
GLOBAL_UNIT_ASSIGNED_CONTEXT((#57901,#57903,#57904))
REPRESENTATION_CONTEXT('','3D')
);
#57850=(
GEOMETRIC_REPRESENTATION_CONTEXT(3)
GLOBAL_UNCERTAINTY_ASSIGNED_CONTEXT((#57791))
GLOBAL_UNIT_ASSIGNED_CONTEXT((#57901,#57903,#57904))
REPRESENTATION_CONTEXT('','3D')
);
#57851=(
GEOMETRIC_REPRESENTATION_CONTEXT(3)
GLOBAL_UNCERTAINTY_ASSIGNED_CONTEXT((#57792))
GLOBAL_UNIT_ASSIGNED_CONTEXT((#57901,#57903,#57904))
REPRESENTATION_CONTEXT('','3D')
);
#57852=(
GEOMETRIC_REPRESENTATION_CONTEXT(3)
GLOBAL_UNCERTAINTY_ASSIGNED_CONTEXT((#57793))
GLOBAL_UNIT_ASSIGNED_CONTEXT((#57901,#57903,#57904))
REPRESENTATION_CONTEXT('','3D')
);
#57853=(
GEOMETRIC_REPRESENTATION_CONTEXT(3)
GLOBAL_UNCERTAINTY_ASSIGNED_CONTEXT((#57794))
GLOBAL_UNIT_ASSIGNED_CONTEXT((#57901,#57903,#57904))
REPRESENTATION_CONTEXT('','3D')
);
#57854=(
GEOMETRIC_REPRESENTATION_CONTEXT(3)
GLOBAL_UNCERTAINTY_ASSIGNED_CONTEXT((#57795))
GLOBAL_UNIT_ASSIGNED_CONTEXT((#57901,#57903,#57904))
REPRESENTATION_CONTEXT('','3D')
);
#57855=(
GEOMETRIC_REPRESENTATION_CONTEXT(3)
GLOBAL_UNCERTAINTY_ASSIGNED_CONTEXT((#57796))
GLOBAL_UNIT_ASSIGNED_CONTEXT((#57901,#57903,#57904))
REPRESENTATION_CONTEXT('','3D')
);
#57856=(
GEOMETRIC_REPRESENTATION_CONTEXT(3)
GLOBAL_UNCERTAINTY_ASSIGNED_CONTEXT((#57797))
GLOBAL_UNIT_ASSIGNED_CONTEXT((#57901,#57903,#57904))
REPRESENTATION_CONTEXT('','3D')
);
#57857=(
GEOMETRIC_REPRESENTATION_CONTEXT(3)
GLOBAL_UNCERTAINTY_ASSIGNED_CONTEXT((#57798))
GLOBAL_UNIT_ASSIGNED_CONTEXT((#57901,#57903,#57904))
REPRESENTATION_CONTEXT('','3D')
);
#57858=(
GEOMETRIC_REPRESENTATION_CONTEXT(3)
GLOBAL_UNCERTAINTY_ASSIGNED_CONTEXT((#57799))
GLOBAL_UNIT_ASSIGNED_CONTEXT((#57901,#57903,#57904))
REPRESENTATION_CONTEXT('','3D')
);
#57859=(
GEOMETRIC_REPRESENTATION_CONTEXT(3)
GLOBAL_UNCERTAINTY_ASSIGNED_CONTEXT((#57800))
GLOBAL_UNIT_ASSIGNED_CONTEXT((#57901,#57903,#57904))
REPRESENTATION_CONTEXT('','3D')
);
#57860=(
GEOMETRIC_REPRESENTATION_CONTEXT(3)
GLOBAL_UNCERTAINTY_ASSIGNED_CONTEXT((#57801))
GLOBAL_UNIT_ASSIGNED_CONTEXT((#57901,#57903,#57904))
REPRESENTATION_CONTEXT('','3D')
);
#57861=(
GEOMETRIC_REPRESENTATION_CONTEXT(3)
GLOBAL_UNCERTAINTY_ASSIGNED_CONTEXT((#57802))
GLOBAL_UNIT_ASSIGNED_CONTEXT((#57901,#57903,#57904))
REPRESENTATION_CONTEXT('','3D')
);
#57862=(
GEOMETRIC_REPRESENTATION_CONTEXT(3)
GLOBAL_UNCERTAINTY_ASSIGNED_CONTEXT((#57803))
GLOBAL_UNIT_ASSIGNED_CONTEXT((#57901,#57903,#57904))
REPRESENTATION_CONTEXT('','3D')
);
#57863=(
GEOMETRIC_REPRESENTATION_CONTEXT(3)
GLOBAL_UNCERTAINTY_ASSIGNED_CONTEXT((#57804))
GLOBAL_UNIT_ASSIGNED_CONTEXT((#57901,#57903,#57904))
REPRESENTATION_CONTEXT('','3D')
);
#57864=(
GEOMETRIC_REPRESENTATION_CONTEXT(3)
GLOBAL_UNCERTAINTY_ASSIGNED_CONTEXT((#57805))
GLOBAL_UNIT_ASSIGNED_CONTEXT((#57901,#57903,#57904))
REPRESENTATION_CONTEXT('','3D')
);
#57865=(
GEOMETRIC_REPRESENTATION_CONTEXT(3)
GLOBAL_UNCERTAINTY_ASSIGNED_CONTEXT((#57806))
GLOBAL_UNIT_ASSIGNED_CONTEXT((#57901,#57903,#57904))
REPRESENTATION_CONTEXT('','3D')
);
#57866=(
GEOMETRIC_REPRESENTATION_CONTEXT(3)
GLOBAL_UNCERTAINTY_ASSIGNED_CONTEXT((#57807))
GLOBAL_UNIT_ASSIGNED_CONTEXT((#57901,#57903,#57904))
REPRESENTATION_CONTEXT('','3D')
);
#57867=(
GEOMETRIC_REPRESENTATION_CONTEXT(3)
GLOBAL_UNCERTAINTY_ASSIGNED_CONTEXT((#57808))
GLOBAL_UNIT_ASSIGNED_CONTEXT((#57901,#57903,#57904))
REPRESENTATION_CONTEXT('','3D')
);
#57868=(
GEOMETRIC_REPRESENTATION_CONTEXT(3)
GLOBAL_UNCERTAINTY_ASSIGNED_CONTEXT((#57809))
GLOBAL_UNIT_ASSIGNED_CONTEXT((#57901,#57903,#57904))
REPRESENTATION_CONTEXT('','3D')
);
#57869=(
GEOMETRIC_REPRESENTATION_CONTEXT(3)
GLOBAL_UNCERTAINTY_ASSIGNED_CONTEXT((#57810))
GLOBAL_UNIT_ASSIGNED_CONTEXT((#57901,#57903,#57904))
REPRESENTATION_CONTEXT('','3D')
);
#57870=(
GEOMETRIC_REPRESENTATION_CONTEXT(3)
GLOBAL_UNCERTAINTY_ASSIGNED_CONTEXT((#57811))
GLOBAL_UNIT_ASSIGNED_CONTEXT((#57901,#57903,#57904))
REPRESENTATION_CONTEXT('','3D')
);
#57871=(
GEOMETRIC_REPRESENTATION_CONTEXT(3)
GLOBAL_UNCERTAINTY_ASSIGNED_CONTEXT((#57812))
GLOBAL_UNIT_ASSIGNED_CONTEXT((#57901,#57903,#57904))
REPRESENTATION_CONTEXT('','3D')
);
#57872=(
GEOMETRIC_REPRESENTATION_CONTEXT(3)
GLOBAL_UNCERTAINTY_ASSIGNED_CONTEXT((#57813))
GLOBAL_UNIT_ASSIGNED_CONTEXT((#57901,#57903,#57904))
REPRESENTATION_CONTEXT('','3D')
);
#57873=(
GEOMETRIC_REPRESENTATION_CONTEXT(3)
GLOBAL_UNCERTAINTY_ASSIGNED_CONTEXT((#57814))
GLOBAL_UNIT_ASSIGNED_CONTEXT((#57901,#57903,#57904))
REPRESENTATION_CONTEXT('','3D')
);
#57874=(
GEOMETRIC_REPRESENTATION_CONTEXT(3)
GLOBAL_UNCERTAINTY_ASSIGNED_CONTEXT((#57815))
GLOBAL_UNIT_ASSIGNED_CONTEXT((#57901,#57903,#57904))
REPRESENTATION_CONTEXT('','3D')
);
#57875=(
GEOMETRIC_REPRESENTATION_CONTEXT(3)
GLOBAL_UNCERTAINTY_ASSIGNED_CONTEXT((#57816))
GLOBAL_UNIT_ASSIGNED_CONTEXT((#57901,#57903,#57904))
REPRESENTATION_CONTEXT('','3D')
);
#57876=(
GEOMETRIC_REPRESENTATION_CONTEXT(3)
GLOBAL_UNCERTAINTY_ASSIGNED_CONTEXT((#57817))
GLOBAL_UNIT_ASSIGNED_CONTEXT((#57901,#57903,#57904))
REPRESENTATION_CONTEXT('','3D')
);
#57877=(
GEOMETRIC_REPRESENTATION_CONTEXT(3)
GLOBAL_UNCERTAINTY_ASSIGNED_CONTEXT((#57818))
GLOBAL_UNIT_ASSIGNED_CONTEXT((#57901,#57903,#57904))
REPRESENTATION_CONTEXT('','3D')
);
#57878=(
GEOMETRIC_REPRESENTATION_CONTEXT(3)
GLOBAL_UNCERTAINTY_ASSIGNED_CONTEXT((#57819))
GLOBAL_UNIT_ASSIGNED_CONTEXT((#57901,#57903,#57904))
REPRESENTATION_CONTEXT('','3D')
);
#57879=(
GEOMETRIC_REPRESENTATION_CONTEXT(3)
GLOBAL_UNCERTAINTY_ASSIGNED_CONTEXT((#57820))
GLOBAL_UNIT_ASSIGNED_CONTEXT((#57901,#57903,#57904))
REPRESENTATION_CONTEXT('','3D')
);
#57880=(
GEOMETRIC_REPRESENTATION_CONTEXT(3)
GLOBAL_UNCERTAINTY_ASSIGNED_CONTEXT((#57821))
GLOBAL_UNIT_ASSIGNED_CONTEXT((#57901,#57903,#57904))
REPRESENTATION_CONTEXT('','3D')
);
#57881=(
GEOMETRIC_REPRESENTATION_CONTEXT(3)
GLOBAL_UNCERTAINTY_ASSIGNED_CONTEXT((#57822))
GLOBAL_UNIT_ASSIGNED_CONTEXT((#57901,#57903,#57904))
REPRESENTATION_CONTEXT('','3D')
);
#57882=(
GEOMETRIC_REPRESENTATION_CONTEXT(3)
GLOBAL_UNCERTAINTY_ASSIGNED_CONTEXT((#57823))
GLOBAL_UNIT_ASSIGNED_CONTEXT((#57901,#57903,#57904))
REPRESENTATION_CONTEXT('','3D')
);
#57883=(
GEOMETRIC_REPRESENTATION_CONTEXT(3)
GLOBAL_UNCERTAINTY_ASSIGNED_CONTEXT((#57824))
GLOBAL_UNIT_ASSIGNED_CONTEXT((#57901,#57903,#57904))
REPRESENTATION_CONTEXT('','3D')
);
#57884=(
GEOMETRIC_REPRESENTATION_CONTEXT(3)
GLOBAL_UNCERTAINTY_ASSIGNED_CONTEXT((#57825))
GLOBAL_UNIT_ASSIGNED_CONTEXT((#57901,#57903,#57904))
REPRESENTATION_CONTEXT('','3D')
);
#57885=(
GEOMETRIC_REPRESENTATION_CONTEXT(3)
GLOBAL_UNCERTAINTY_ASSIGNED_CONTEXT((#57826))
GLOBAL_UNIT_ASSIGNED_CONTEXT((#57901,#57903,#57904))
REPRESENTATION_CONTEXT('','3D')
);
#57886=(
GEOMETRIC_REPRESENTATION_CONTEXT(3)
GLOBAL_UNCERTAINTY_ASSIGNED_CONTEXT((#57827))
GLOBAL_UNIT_ASSIGNED_CONTEXT((#57901,#57903,#57904))
REPRESENTATION_CONTEXT('','3D')
);
#57887=(
GEOMETRIC_REPRESENTATION_CONTEXT(3)
GLOBAL_UNCERTAINTY_ASSIGNED_CONTEXT((#57828))
GLOBAL_UNIT_ASSIGNED_CONTEXT((#57901,#57903,#57904))
REPRESENTATION_CONTEXT('','3D')
);
#57888=(
GEOMETRIC_REPRESENTATION_CONTEXT(3)
GLOBAL_UNCERTAINTY_ASSIGNED_CONTEXT((#57829))
GLOBAL_UNIT_ASSIGNED_CONTEXT((#57901,#57903,#57904))
REPRESENTATION_CONTEXT('','3D')
);
#57889=(
GEOMETRIC_REPRESENTATION_CONTEXT(3)
GLOBAL_UNCERTAINTY_ASSIGNED_CONTEXT((#57830))
GLOBAL_UNIT_ASSIGNED_CONTEXT((#57901,#57903,#57904))
REPRESENTATION_CONTEXT('','3D')
);
#57890=(
GEOMETRIC_REPRESENTATION_CONTEXT(3)
GLOBAL_UNCERTAINTY_ASSIGNED_CONTEXT((#57831))
GLOBAL_UNIT_ASSIGNED_CONTEXT((#57901,#57903,#57904))
REPRESENTATION_CONTEXT('','3D')
);
#57891=(
GEOMETRIC_REPRESENTATION_CONTEXT(3)
GLOBAL_UNCERTAINTY_ASSIGNED_CONTEXT((#57832))
GLOBAL_UNIT_ASSIGNED_CONTEXT((#57901,#57903,#57904))
REPRESENTATION_CONTEXT('','3D')
);
#57892=(
GEOMETRIC_REPRESENTATION_CONTEXT(3)
GLOBAL_UNCERTAINTY_ASSIGNED_CONTEXT((#57833))
GLOBAL_UNIT_ASSIGNED_CONTEXT((#57901,#57903,#57904))
REPRESENTATION_CONTEXT('','3D')
);
#57893=(
GEOMETRIC_REPRESENTATION_CONTEXT(3)
GLOBAL_UNCERTAINTY_ASSIGNED_CONTEXT((#57834))
GLOBAL_UNIT_ASSIGNED_CONTEXT((#57901,#57903,#57904))
REPRESENTATION_CONTEXT('','3D')
);
#57894=(
GEOMETRIC_REPRESENTATION_CONTEXT(3)
GLOBAL_UNCERTAINTY_ASSIGNED_CONTEXT((#57835))
GLOBAL_UNIT_ASSIGNED_CONTEXT((#57901,#57903,#57904))
REPRESENTATION_CONTEXT('','3D')
);
#57895=(
GEOMETRIC_REPRESENTATION_CONTEXT(3)
GLOBAL_UNCERTAINTY_ASSIGNED_CONTEXT((#57836))
GLOBAL_UNIT_ASSIGNED_CONTEXT((#57901,#57903,#57904))
REPRESENTATION_CONTEXT('','3D')
);
#57896=(
GEOMETRIC_REPRESENTATION_CONTEXT(3)
GLOBAL_UNCERTAINTY_ASSIGNED_CONTEXT((#57837))
GLOBAL_UNIT_ASSIGNED_CONTEXT((#57901,#57903,#57904))
REPRESENTATION_CONTEXT('','3D')
);
#57897=(
GEOMETRIC_REPRESENTATION_CONTEXT(3)
GLOBAL_UNCERTAINTY_ASSIGNED_CONTEXT((#57838))
GLOBAL_UNIT_ASSIGNED_CONTEXT((#57901,#57903,#57904))
REPRESENTATION_CONTEXT('','3D')
);
#57898=(
GEOMETRIC_REPRESENTATION_CONTEXT(3)
GLOBAL_UNCERTAINTY_ASSIGNED_CONTEXT((#57839))
GLOBAL_UNIT_ASSIGNED_CONTEXT((#57901,#57903,#57904))
REPRESENTATION_CONTEXT('','3D')
);
#57899=(
GEOMETRIC_REPRESENTATION_CONTEXT(3)
GLOBAL_UNCERTAINTY_ASSIGNED_CONTEXT((#57840))
GLOBAL_UNIT_ASSIGNED_CONTEXT((#57901,#57903,#57904))
REPRESENTATION_CONTEXT('','3D')
);
#57900=(
GEOMETRIC_REPRESENTATION_CONTEXT(3)
GLOBAL_UNCERTAINTY_ASSIGNED_CONTEXT((#57841))
GLOBAL_UNIT_ASSIGNED_CONTEXT((#57901,#57903,#57904))
REPRESENTATION_CONTEXT('','3D')
);
#57901=(
LENGTH_UNIT()
NAMED_UNIT(*)
SI_UNIT(.CENTI.,.METRE.)
);
#57902=(
LENGTH_UNIT()
NAMED_UNIT(*)
SI_UNIT($,.METRE.)
);
#57903=(
NAMED_UNIT(*)
PLANE_ANGLE_UNIT()
SI_UNIT($,.RADIAN.)
);
#57904=(
NAMED_UNIT(*)
SI_UNIT($,.STERADIAN.)
SOLID_ANGLE_UNIT()
);
#57905=SHAPE_DEFINITION_REPRESENTATION(#57963,#58109);
#57906=SHAPE_DEFINITION_REPRESENTATION(#57964,#58110);
#57907=SHAPE_DEFINITION_REPRESENTATION(#57965,#58111);
#57908=SHAPE_DEFINITION_REPRESENTATION(#57966,#58112);
#57909=SHAPE_DEFINITION_REPRESENTATION(#57967,#58113);
#57910=SHAPE_DEFINITION_REPRESENTATION(#57968,#58114);
#57911=SHAPE_DEFINITION_REPRESENTATION(#57969,#58115);
#57912=SHAPE_DEFINITION_REPRESENTATION(#57970,#58116);
#57913=SHAPE_DEFINITION_REPRESENTATION(#57971,#58117);
#57914=SHAPE_DEFINITION_REPRESENTATION(#57972,#58118);
#57915=SHAPE_DEFINITION_REPRESENTATION(#57973,#58119);
#57916=SHAPE_DEFINITION_REPRESENTATION(#57974,#58120);
#57917=SHAPE_DEFINITION_REPRESENTATION(#57975,#58121);
#57918=SHAPE_DEFINITION_REPRESENTATION(#57976,#58122);
#57919=SHAPE_DEFINITION_REPRESENTATION(#57977,#58123);
#57920=SHAPE_DEFINITION_REPRESENTATION(#57978,#58124);
#57921=SHAPE_DEFINITION_REPRESENTATION(#57979,#58125);
#57922=SHAPE_DEFINITION_REPRESENTATION(#57980,#58126);
#57923=SHAPE_DEFINITION_REPRESENTATION(#57981,#58127);
#57924=SHAPE_DEFINITION_REPRESENTATION(#57982,#58128);
#57925=SHAPE_DEFINITION_REPRESENTATION(#57988,#58129);
#57926=SHAPE_DEFINITION_REPRESENTATION(#57989,#58130);
#57927=SHAPE_DEFINITION_REPRESENTATION(#57990,#58131);
#57928=SHAPE_DEFINITION_REPRESENTATION(#57991,#58132);
#57929=SHAPE_DEFINITION_REPRESENTATION(#57992,#58133);
#57930=SHAPE_DEFINITION_REPRESENTATION(#57993,#58134);
#57931=SHAPE_DEFINITION_REPRESENTATION(#57994,#58135);
#57932=SHAPE_DEFINITION_REPRESENTATION(#57995,#58136);
#57933=SHAPE_DEFINITION_REPRESENTATION(#57996,#58137);
#57934=SHAPE_DEFINITION_REPRESENTATION(#57997,#58138);
#57935=SHAPE_DEFINITION_REPRESENTATION(#57998,#58139);
#57936=SHAPE_DEFINITION_REPRESENTATION(#58002,#58140);
#57937=SHAPE_DEFINITION_REPRESENTATION(#58003,#58141);
#57938=SHAPE_DEFINITION_REPRESENTATION(#58004,#58142);
#57939=SHAPE_DEFINITION_REPRESENTATION(#58005,#58143);
#57940=SHAPE_DEFINITION_REPRESENTATION(#58006,#58144);
#57941=SHAPE_DEFINITION_REPRESENTATION(#58007,#58145);
#57942=SHAPE_DEFINITION_REPRESENTATION(#58008,#58146);
#57943=SHAPE_DEFINITION_REPRESENTATION(#58009,#58147);
#57944=SHAPE_DEFINITION_REPRESENTATION(#58015,#58148);
#57945=SHAPE_DEFINITION_REPRESENTATION(#58016,#58149);
#57946=SHAPE_DEFINITION_REPRESENTATION(#58017,#58150);
#57947=SHAPE_DEFINITION_REPRESENTATION(#58018,#58151);
#57948=SHAPE_DEFINITION_REPRESENTATION(#58019,#58152);
#57949=SHAPE_DEFINITION_REPRESENTATION(#58020,#58153);
#57950=SHAPE_DEFINITION_REPRESENTATION(#58021,#58154);
#57951=SHAPE_DEFINITION_REPRESENTATION(#58022,#58155);
#57952=SHAPE_DEFINITION_REPRESENTATION(#58023,#58156);
#57953=SHAPE_DEFINITION_REPRESENTATION(#58024,#58157);
#57954=SHAPE_DEFINITION_REPRESENTATION(#58025,#58158);
#57955=SHAPE_DEFINITION_REPRESENTATION(#58026,#58159);
#57956=SHAPE_DEFINITION_REPRESENTATION(#58027,#58160);
#57957=SHAPE_DEFINITION_REPRESENTATION(#58028,#58161);
#57958=SHAPE_DEFINITION_REPRESENTATION(#58029,#58162);
#57959=SHAPE_DEFINITION_REPRESENTATION(#58030,#58163);
#57960=SHAPE_DEFINITION_REPRESENTATION(#58031,#58164);
#57961=SHAPE_DEFINITION_REPRESENTATION(#58032,#58165);
#57962=SHAPE_DEFINITION_REPRESENTATION(#58033,#58166);
#57963=PRODUCT_DEFINITION_SHAPE('',$,#58168);
#57964=PRODUCT_DEFINITION_SHAPE('',$,#58169);
#57965=PRODUCT_DEFINITION_SHAPE('',$,#58170);
#57966=PRODUCT_DEFINITION_SHAPE('',$,#58171);
#57967=PRODUCT_DEFINITION_SHAPE('',$,#58172);
#57968=PRODUCT_DEFINITION_SHAPE('',$,#58173);
#57969=PRODUCT_DEFINITION_SHAPE('',$,#58174);
#57970=PRODUCT_DEFINITION_SHAPE('',$,#58175);
#57971=PRODUCT_DEFINITION_SHAPE('',$,#58176);
#57972=PRODUCT_DEFINITION_SHAPE('',$,#58177);
#57973=PRODUCT_DEFINITION_SHAPE('',$,#58178);
#57974=PRODUCT_DEFINITION_SHAPE('',$,#58179);
#57975=PRODUCT_DEFINITION_SHAPE('',$,#58180);
#57976=PRODUCT_DEFINITION_SHAPE('',$,#58181);
#57977=PRODUCT_DEFINITION_SHAPE('',$,#58182);
#57978=PRODUCT_DEFINITION_SHAPE('',$,#58183);
#57979=PRODUCT_DEFINITION_SHAPE('',$,#58184);
#57980=PRODUCT_DEFINITION_SHAPE('',$,#58185);
#57981=PRODUCT_DEFINITION_SHAPE('',$,#58186);
#57982=PRODUCT_DEFINITION_SHAPE('',$,#58187);
#57983=PRODUCT_DEFINITION_SHAPE($,$,#641);
#57984=PRODUCT_DEFINITION_SHAPE($,$,#642);
#57985=PRODUCT_DEFINITION_SHAPE($,$,#643);
#57986=PRODUCT_DEFINITION_SHAPE($,$,#644);
#57987=PRODUCT_DEFINITION_SHAPE($,$,#645);
#57988=PRODUCT_DEFINITION_SHAPE('',$,#58188);
#57989=PRODUCT_DEFINITION_SHAPE('',$,#58189);
#57990=PRODUCT_DEFINITION_SHAPE('',$,#58190);
#57991=PRODUCT_DEFINITION_SHAPE('',$,#58191);
#57992=PRODUCT_DEFINITION_SHAPE('',$,#58192);
#57993=PRODUCT_DEFINITION_SHAPE('',$,#58193);
#57994=PRODUCT_DEFINITION_SHAPE('',$,#58194);
#57995=PRODUCT_DEFINITION_SHAPE('',$,#58195);
#57996=PRODUCT_DEFINITION_SHAPE('',$,#58196);
#57997=PRODUCT_DEFINITION_SHAPE('',$,#58197);
#57998=PRODUCT_DEFINITION_SHAPE('',$,#58198);
#57999=PRODUCT_DEFINITION_SHAPE($,$,#646);
#58000=PRODUCT_DEFINITION_SHAPE($,$,#647);
#58001=PRODUCT_DEFINITION_SHAPE($,$,#648);
#58002=PRODUCT_DEFINITION_SHAPE('',$,#58199);
#58003=PRODUCT_DEFINITION_SHAPE('',$,#58200);
#58004=PRODUCT_DEFINITION_SHAPE('',$,#58201);
#58005=PRODUCT_DEFINITION_SHAPE('',$,#58202);
#58006=PRODUCT_DEFINITION_SHAPE('',$,#58203);
#58007=PRODUCT_DEFINITION_SHAPE('',$,#58204);
#58008=PRODUCT_DEFINITION_SHAPE('',$,#58205);
#58009=PRODUCT_DEFINITION_SHAPE('',$,#58206);
#58010=PRODUCT_DEFINITION_SHAPE($,$,#649);
#58011=PRODUCT_DEFINITION_SHAPE($,$,#650);
#58012=PRODUCT_DEFINITION_SHAPE($,$,#651);
#58013=PRODUCT_DEFINITION_SHAPE($,$,#652);
#58014=PRODUCT_DEFINITION_SHAPE($,$,#653);
#58015=PRODUCT_DEFINITION_SHAPE('',$,#58207);
#58016=PRODUCT_DEFINITION_SHAPE('',$,#58208);
#58017=PRODUCT_DEFINITION_SHAPE('',$,#58209);
#58018=PRODUCT_DEFINITION_SHAPE('',$,#58210);
#58019=PRODUCT_DEFINITION_SHAPE('',$,#58211);
#58020=PRODUCT_DEFINITION_SHAPE('',$,#58212);
#58021=PRODUCT_DEFINITION_SHAPE('',$,#58213);
#58022=PRODUCT_DEFINITION_SHAPE('',$,#58214);
#58023=PRODUCT_DEFINITION_SHAPE('',$,#58215);
#58024=PRODUCT_DEFINITION_SHAPE('',$,#58216);
#58025=PRODUCT_DEFINITION_SHAPE('',$,#58217);
#58026=PRODUCT_DEFINITION_SHAPE('',$,#58218);
#58027=PRODUCT_DEFINITION_SHAPE('',$,#58219);
#58028=PRODUCT_DEFINITION_SHAPE('',$,#58220);
#58029=PRODUCT_DEFINITION_SHAPE('',$,#58221);
#58030=PRODUCT_DEFINITION_SHAPE('',$,#58222);
#58031=PRODUCT_DEFINITION_SHAPE('',$,#58223);
#58032=PRODUCT_DEFINITION_SHAPE('',$,#58224);
#58033=PRODUCT_DEFINITION_SHAPE('',$,#58225);
#58034=PRODUCT_DEFINITION_SHAPE($,$,#654);
#58035=PRODUCT_DEFINITION_SHAPE($,$,#655);
#58036=PRODUCT_DEFINITION_SHAPE($,$,#656);
#58037=PRODUCT_DEFINITION_SHAPE($,$,#657);
#58038=PRODUCT_DEFINITION_SHAPE($,$,#658);
#58039=PRODUCT_DEFINITION_SHAPE($,$,#659);
#58040=PRODUCT_DEFINITION_SHAPE($,$,#660);
#58041=PRODUCT_DEFINITION_SHAPE($,$,#661);
#58042=PRODUCT_DEFINITION_SHAPE($,$,#662);
#58043=PRODUCT_DEFINITION_SHAPE($,$,#663);
#58044=PRODUCT_DEFINITION_SHAPE($,$,#664);
#58045=PRODUCT_DEFINITION_SHAPE($,$,#665);
#58046=PRODUCT_DEFINITION_SHAPE($,$,#666);
#58047=PRODUCT_DEFINITION_SHAPE($,$,#667);
#58048=PRODUCT_DEFINITION_SHAPE($,$,#668);
#58049=PRODUCT_DEFINITION_SHAPE($,$,#669);
#58050=PRODUCT_DEFINITION_SHAPE($,$,#670);
#58051=PRODUCT_DEFINITION_SHAPE($,$,#671);
#58052=PRODUCT_DEFINITION_SHAPE($,$,#672);
#58053=PRODUCT_DEFINITION_SHAPE($,$,#673);
#58054=PRODUCT_DEFINITION_SHAPE($,$,#674);
#58055=PRODUCT_DEFINITION_SHAPE($,$,#675);
#58056=PRODUCT_DEFINITION_SHAPE($,$,#676);
#58057=PRODUCT_DEFINITION_SHAPE($,$,#677);
#58058=PRODUCT_DEFINITION_SHAPE($,$,#678);
#58059=PRODUCT_DEFINITION_SHAPE($,$,#679);
#58060=PRODUCT_DEFINITION_SHAPE($,$,#680);
#58061=PRODUCT_DEFINITION_SHAPE($,$,#681);
#58062=PRODUCT_DEFINITION_SHAPE($,$,#682);
#58063=PRODUCT_DEFINITION_SHAPE($,$,#683);
#58064=PRODUCT_DEFINITION_SHAPE($,$,#684);
#58065=PRODUCT_DEFINITION_SHAPE($,$,#685);
#58066=PRODUCT_DEFINITION_SHAPE($,$,#686);
#58067=PRODUCT_DEFINITION_SHAPE($,$,#687);
#58068=PRODUCT_DEFINITION_SHAPE($,$,#688);
#58069=PRODUCT_DEFINITION_SHAPE($,$,#689);
#58070=PRODUCT_DEFINITION_SHAPE($,$,#690);
#58071=PRODUCT_DEFINITION_SHAPE($,$,#691);
#58072=PRODUCT_DEFINITION_SHAPE($,$,#692);
#58073=PRODUCT_DEFINITION_SHAPE($,$,#693);
#58074=PRODUCT_DEFINITION_SHAPE($,$,#694);
#58075=PRODUCT_DEFINITION_SHAPE($,$,#695);
#58076=PRODUCT_DEFINITION_SHAPE($,$,#696);
#58077=PRODUCT_DEFINITION_SHAPE($,$,#697);
#58078=PRODUCT_DEFINITION_SHAPE($,$,#698);
#58079=PRODUCT_DEFINITION_SHAPE($,$,#699);
#58080=PRODUCT_DEFINITION_SHAPE($,$,#700);
#58081=PRODUCT_DEFINITION_SHAPE($,$,#701);
#58082=PRODUCT_DEFINITION_SHAPE($,$,#702);
#58083=PRODUCT_DEFINITION_SHAPE($,$,#703);
#58084=PRODUCT_DEFINITION_SHAPE($,$,#704);
#58085=PRODUCT_DEFINITION_SHAPE($,$,#705);
#58086=PRODUCT_DEFINITION_SHAPE($,$,#706);
#58087=PRODUCT_DEFINITION_SHAPE($,$,#707);
#58088=PRODUCT_DEFINITION_SHAPE($,$,#708);
#58089=PRODUCT_DEFINITION_SHAPE($,$,#709);
#58090=PRODUCT_DEFINITION_SHAPE($,$,#710);
#58091=PRODUCT_DEFINITION_SHAPE($,$,#711);
#58092=PRODUCT_DEFINITION_SHAPE($,$,#712);
#58093=PRODUCT_DEFINITION_SHAPE($,$,#713);
#58094=PRODUCT_DEFINITION_SHAPE($,$,#714);
#58095=PRODUCT_DEFINITION_SHAPE($,$,#715);
#58096=PRODUCT_DEFINITION_SHAPE($,$,#716);
#58097=PRODUCT_DEFINITION_SHAPE($,$,#717);
#58098=PRODUCT_DEFINITION_SHAPE($,$,#718);
#58099=PRODUCT_DEFINITION_SHAPE($,$,#719);
#58100=PRODUCT_DEFINITION_SHAPE($,$,#720);
#58101=PRODUCT_DEFINITION_SHAPE($,$,#721);
#58102=PRODUCT_DEFINITION_SHAPE($,$,#722);
#58103=PRODUCT_DEFINITION_SHAPE($,$,#723);
#58104=PRODUCT_DEFINITION_SHAPE($,$,#724);
#58105=PRODUCT_DEFINITION_SHAPE($,$,#725);
#58106=PRODUCT_DEFINITION_SHAPE($,$,#726);
#58107=PRODUCT_DEFINITION_SHAPE($,$,#727);
#58108=PRODUCT_DEFINITION_SHAPE($,$,#728);
#58109=SHAPE_REPRESENTATION('',(#14195,#15574,#15575,#15576,#15577),#57842);
#58110=SHAPE_REPRESENTATION('',(#14196,#15503,#15504,#15505,#15506,#15507,
#15508,#15509,#15510,#15511,#15512,#15513,#15514,#15515,#15516,#15517,#15518,
#15519,#15520,#15521,#15522,#15523,#15524,#15525,#15526,#15527,#15528,#15529,
#15530,#15531,#15532,#15533),#57843);
#58111=SHAPE_REPRESENTATION('',(#14197),#57844);
#58112=SHAPE_REPRESENTATION('',(#14240),#57845);
#58113=SHAPE_REPRESENTATION('',(#14247),#57846);
#58114=SHAPE_REPRESENTATION('',(#14254),#57847);
#58115=SHAPE_REPRESENTATION('',(#14324),#57848);
#58116=SHAPE_REPRESENTATION('',(#14333),#57849);
#58117=SHAPE_REPRESENTATION('',(#14367),#57850);
#58118=SHAPE_REPRESENTATION('',(#14389),#57851);
#58119=SHAPE_REPRESENTATION('',(#14432),#57852);
#58120=SHAPE_REPRESENTATION('',(#14441),#57853);
#58121=SHAPE_REPRESENTATION('',(#14447),#57854);
#58122=SHAPE_REPRESENTATION('',(#14453),#57855);
#58123=SHAPE_REPRESENTATION('',(#14496,#14619,#14620,#14621,#14622,#14623),
#57856);
#58124=SHAPE_REPRESENTATION('',(#14497),#57857);
#58125=SHAPE_REPRESENTATION('',(#14517),#57858);
#58126=SHAPE_REPRESENTATION('',(#14537),#57859);
#58127=SHAPE_REPRESENTATION('',(#14552),#57860);
#58128=SHAPE_REPRESENTATION('',(#14602),#57861);
#58129=SHAPE_REPRESENTATION('',(#14624),#57862);
#58130=SHAPE_REPRESENTATION('',(#14650,#15534,#15535,#15536,#15537,#15538,
#15539,#15540,#15541,#15542,#15543,#15544,#15545,#15546,#15547,#15548,#15549,
#15550,#15551,#15552,#15553,#15554),#57863);
#58131=SHAPE_REPRESENTATION('',(#14651),#57864);
#58132=SHAPE_REPRESENTATION('',(#14694),#57865);
#58133=SHAPE_REPRESENTATION('',(#14701),#57866);
#58134=SHAPE_REPRESENTATION('',(#14771),#57867);
#58135=SHAPE_REPRESENTATION('',(#14780),#57868);
#58136=SHAPE_REPRESENTATION('',(#14801,#14863,#14864,#14865),#57869);
#58137=SHAPE_REPRESENTATION('',(#14802),#57870);
#58138=SHAPE_REPRESENTATION('',(#14841),#57871);
#58139=SHAPE_REPRESENTATION('',(#14852),#57872);
#58140=SHAPE_REPRESENTATION('',(#14866),#57873);
#58141=SHAPE_REPRESENTATION('',(#14883),#57874);
#58142=SHAPE_REPRESENTATION('',(#14907,#15036,#15037,#15038,#15039,#15040),
#57875);
#58143=SHAPE_REPRESENTATION('',(#14908),#57876);
#58144=SHAPE_REPRESENTATION('',(#14928),#57877);
#58145=SHAPE_REPRESENTATION('',(#14948),#57878);
#58146=SHAPE_REPRESENTATION('',(#14965),#57879);
#58147=SHAPE_REPRESENTATION('',(#15019),#57880);
#58148=SHAPE_REPRESENTATION('',(#15041,#15555,#15556,#15557,#15558,#15559,
#15560,#15561,#15562,#15563,#15564),#57881);
#58149=SHAPE_REPRESENTATION('',(#15042),#57882);
#58150=SHAPE_REPRESENTATION('',(#15067),#57883);
#58151=SHAPE_REPRESENTATION('',(#15076),#57884);
#58152=SHAPE_REPRESENTATION('',(#15085),#57885);
#58153=SHAPE_REPRESENTATION('',(#15094),#57886);
#58154=SHAPE_REPRESENTATION('',(#15112),#57887);
#58155=SHAPE_REPRESENTATION('',(#15119),#57888);
#58156=SHAPE_REPRESENTATION('',(#15128),#57889);
#58157=SHAPE_REPRESENTATION('',(#15221,#15565,#15566,#15567,#15568,#15569,
#15570,#15571,#15572,#15573),#57890);
#58158=SHAPE_REPRESENTATION('',(#15222),#57891);
#58159=SHAPE_REPRESENTATION('',(#15247),#57892);
#58160=SHAPE_REPRESENTATION('',(#15256),#57893);
#58161=SHAPE_REPRESENTATION('',(#15265),#57894);
#58162=SHAPE_REPRESENTATION('',(#15275),#57895);
#58163=SHAPE_REPRESENTATION('',(#15282),#57896);
#58164=SHAPE_REPRESENTATION('',(#15291),#57897);
#58165=SHAPE_REPRESENTATION('',(#15306),#57898);
#58166=SHAPE_REPRESENTATION('',(#15479),#57899);
#58167=PRODUCT_DEFINITION_CONTEXT('part definition',#58343,'design');
#58168=PRODUCT_DEFINITION('PAT-046','PAT-046',#58226,
#58167);
#58169=PRODUCT_DEFINITION('Base and indicator stand',
'Base and indicator stand',#58227,#58167);
#58170=PRODUCT_DEFINITION('Base','Base',#58228,#58167);
#58171=PRODUCT_DEFINITION('Foot strip','Foot strip',#58229,#58167);
#58172=PRODUCT_DEFINITION('Foot strip (1)','Foot strip (1)',#58230,#58167);
#58173=PRODUCT_DEFINITION('Input bearing post','Input bearing post',#58231,
#58167);
#58174=PRODUCT_DEFINITION('Input outer race spacer',
'Input outer race spacer',#58232,#58167);
#58175=PRODUCT_DEFINITION('Input bearing cap','Input bearing cap',#58233,
#58167);
#58176=PRODUCT_DEFINITION('Indicator stand','Indicator stand',#58234,#58167);
#58177=PRODUCT_DEFINITION('Indicator arm','Indicator arm',#58235,#58167);
#58178=PRODUCT_DEFINITION('Indicator body envelope',
'Indicator body envelope',#58236,#58167);
#58179=PRODUCT_DEFINITION('Indicator face','Indicator face',#58237,#58167);
#58180=PRODUCT_DEFINITION('Retracted indicator probe',
'Retracted indicator probe',#58238,#58167);
#58181=PRODUCT_DEFINITION('Linear Guide Rail - 15 mm, 220 mm Long',
'Linear Guide Rail - 15 mm, 220 mm Long',#58239,#58167);
#58182=PRODUCT_DEFINITION('Sealed Ball Bearing - 12 x 32 x 10 mm',
'Sealed Ball Bearing - 12 x 32 x 10 mm',#58240,#58167);
#58183=PRODUCT_DEFINITION('Inner ring','Inner ring',#58241,#58167);
#58184=PRODUCT_DEFINITION('Outer ring','Outer ring',#58242,#58167);
#58185=PRODUCT_DEFINITION('Balls','Balls',#58243,#58167);
#58186=PRODUCT_DEFINITION('Cage','Cage',#58244,#58167);
#58187=PRODUCT_DEFINITION('Seals 2RS','Seals 2RS',#58245,#58167);
#58188=PRODUCT_DEFINITION('Cap Screw - M4x16','Cap Screw - M4x16',#58246,
#58167);
#58189=PRODUCT_DEFINITION('Sliding bearing carrier',
'Sliding bearing carrier',#58247,#58167);
#58190=PRODUCT_DEFINITION('Carrier plate','Carrier plate',#58248,#58167);
#58191=PRODUCT_DEFINITION('Retracted rail lock pad',
'Retracted rail lock pad',#58249,#58167);
#58192=PRODUCT_DEFINITION('Output bearing post','Output bearing post',#58250,
#58167);
#58193=PRODUCT_DEFINITION('Output outer race spacer',
'Output outer race spacer',#58251,#58167);
#58194=PRODUCT_DEFINITION('Output bearing cap','Output bearing cap',#58252,
#58167);
#58195=PRODUCT_DEFINITION('Flanged Linear Guide Carriage - 15 mm',
'Flanged Linear Guide Carriage - 15 mm',#58253,#58167);
#58196=PRODUCT_DEFINITION('Block','Block',#58254,#58167);
#58197=PRODUCT_DEFINITION('End cap +','End cap +',#58255,#58167);
#58198=PRODUCT_DEFINITION('End cap','End cap',#58256,#58167);
#58199=PRODUCT_DEFINITION('Socket Set Screw - M4x6',
'Socket Set Screw - M4x6',#58257,#58167);
#58200=PRODUCT_DEFINITION('M5x14 Cap Screw','M5x14 Cap Screw',#58258,#58167);
#58201=PRODUCT_DEFINITION('Sealed Ball Bearing - 20 x 47 x 14 mm',
'Sealed Ball Bearing - 20 x 47 x 14 mm',#58259,#58167);
#58202=PRODUCT_DEFINITION('Inner ring (1)','Inner ring (1)',#58260,#58167);
#58203=PRODUCT_DEFINITION('Outer ring (1)','Outer ring (1)',#58261,#58167);
#58204=PRODUCT_DEFINITION('Balls (1)','Balls (1)',#58262,#58167);
#58205=PRODUCT_DEFINITION('Cage (1)','Cage (1)',#58263,#58167);
#58206=PRODUCT_DEFINITION('Seals 2RS (1)','Seals 2RS (1)',#58264,#58167);
#58207=PRODUCT_DEFINITION('Input gear and arbor','Input gear and arbor',
#58265,#58167);
#58208=PRODUCT_DEFINITION('Input arbor','Input arbor',#58266,#58167);
#58209=PRODUCT_DEFINITION('Input inner sleeve 10 mm',
'Input inner sleeve 10 mm',#58267,#58167);
#58210=PRODUCT_DEFINITION('Input inner sleeve 8 mm',
'Input inner sleeve 8 mm',#58268,#58167);
#58211=PRODUCT_DEFINITION('Input lower sleeve','Input lower sleeve',#58269,
#58167);
#58212=PRODUCT_DEFINITION('Input collar','Input collar',#58270,#58167);
#58213=PRODUCT_DEFINITION('Input parallel key','Input parallel key',#58271,
#58167);
#58214=PRODUCT_DEFINITION('Input keeper','Input keeper',#58272,#58167);
#58215=PRODUCT_DEFINITION('Spur Gear - Module 2, 20 Teeth, 12 mm Bore',
'Spur Gear - Module 2, 20 Teeth, 12 mm Bore',#58273,#58167);
#58216=PRODUCT_DEFINITION('Output gear and arbor',
'Output gear and arbor',#58274,#58167);
#58217=PRODUCT_DEFINITION('Output arbor','Output arbor',#58275,#58167);
#58218=PRODUCT_DEFINITION('Output inner sleeve 6 mm',
'Output inner sleeve 6 mm',#58276,#58167);
#58219=PRODUCT_DEFINITION('Output inner sleeve 8 mm',
'Output inner sleeve 8 mm',#58277,#58167);
#58220=PRODUCT_DEFINITION('Output collar','Output collar',#58278,#58167);
#58221=PRODUCT_DEFINITION('Output parallel key','Output parallel key',#58279,
#58167);
#58222=PRODUCT_DEFINITION('Output keeper','Output keeper',#58280,#58167);
#58223=PRODUCT_DEFINITION('M4x4 collar screw','M4x4 collar screw',#58281,
#58167);
#58224=PRODUCT_DEFINITION('Spur Gear - Module 2, 40 Teeth, 20 mm Bore',
'Spur Gear - Module 2, 40 Teeth, 20 mm Bore',#58282,#58167);
#58225=PRODUCT_DEFINITION('M4x10 Cap Screw','M4x10 Cap Screw',#58283,#58167);
#58226=PRODUCT_DEFINITION_FORMATION('',$,#58345);
#58227=PRODUCT_DEFINITION_FORMATION('',$,#58346);
#58228=PRODUCT_DEFINITION_FORMATION('',$,#58347);
#58229=PRODUCT_DEFINITION_FORMATION('',$,#58348);
#58230=PRODUCT_DEFINITION_FORMATION('',$,#58349);
#58231=PRODUCT_DEFINITION_FORMATION('',$,#58350);
#58232=PRODUCT_DEFINITION_FORMATION('',$,#58351);
#58233=PRODUCT_DEFINITION_FORMATION('',$,#58352);
#58234=PRODUCT_DEFINITION_FORMATION('',$,#58353);
#58235=PRODUCT_DEFINITION_FORMATION('',$,#58354);
#58236=PRODUCT_DEFINITION_FORMATION('',$,#58355);
#58237=PRODUCT_DEFINITION_FORMATION('',$,#58356);
#58238=PRODUCT_DEFINITION_FORMATION('',$,#58357);
#58239=PRODUCT_DEFINITION_FORMATION('',$,#58358);
#58240=PRODUCT_DEFINITION_FORMATION('',$,#58359);
#58241=PRODUCT_DEFINITION_FORMATION('',$,#58360);
#58242=PRODUCT_DEFINITION_FORMATION('',$,#58361);
#58243=PRODUCT_DEFINITION_FORMATION('',$,#58362);
#58244=PRODUCT_DEFINITION_FORMATION('',$,#58363);
#58245=PRODUCT_DEFINITION_FORMATION('',$,#58364);
#58246=PRODUCT_DEFINITION_FORMATION('',$,#58365);
#58247=PRODUCT_DEFINITION_FORMATION('',$,#58366);
#58248=PRODUCT_DEFINITION_FORMATION('',$,#58367);
#58249=PRODUCT_DEFINITION_FORMATION('',$,#58368);
#58250=PRODUCT_DEFINITION_FORMATION('',$,#58369);
#58251=PRODUCT_DEFINITION_FORMATION('',$,#58370);
#58252=PRODUCT_DEFINITION_FORMATION('',$,#58371);
#58253=PRODUCT_DEFINITION_FORMATION('',$,#58372);
#58254=PRODUCT_DEFINITION_FORMATION('',$,#58373);
#58255=PRODUCT_DEFINITION_FORMATION('',$,#58374);
#58256=PRODUCT_DEFINITION_FORMATION('',$,#58375);
#58257=PRODUCT_DEFINITION_FORMATION('',$,#58376);
#58258=PRODUCT_DEFINITION_FORMATION('',$,#58377);
#58259=PRODUCT_DEFINITION_FORMATION('',$,#58378);
#58260=PRODUCT_DEFINITION_FORMATION('',$,#58379);
#58261=PRODUCT_DEFINITION_FORMATION('',$,#58380);
#58262=PRODUCT_DEFINITION_FORMATION('',$,#58381);
#58263=PRODUCT_DEFINITION_FORMATION('',$,#58382);
#58264=PRODUCT_DEFINITION_FORMATION('',$,#58383);
#58265=PRODUCT_DEFINITION_FORMATION('',$,#58384);
#58266=PRODUCT_DEFINITION_FORMATION('',$,#58385);
#58267=PRODUCT_DEFINITION_FORMATION('',$,#58386);
#58268=PRODUCT_DEFINITION_FORMATION('',$,#58387);
#58269=PRODUCT_DEFINITION_FORMATION('',$,#58388);
#58270=PRODUCT_DEFINITION_FORMATION('',$,#58389);
#58271=PRODUCT_DEFINITION_FORMATION('',$,#58390);
#58272=PRODUCT_DEFINITION_FORMATION('',$,#58391);
#58273=PRODUCT_DEFINITION_FORMATION('',$,#58392);
#58274=PRODUCT_DEFINITION_FORMATION('',$,#58393);
#58275=PRODUCT_DEFINITION_FORMATION('',$,#58394);
#58276=PRODUCT_DEFINITION_FORMATION('',$,#58395);
#58277=PRODUCT_DEFINITION_FORMATION('',$,#58396);
#58278=PRODUCT_DEFINITION_FORMATION('',$,#58397);
#58279=PRODUCT_DEFINITION_FORMATION('',$,#58398);
#58280=PRODUCT_DEFINITION_FORMATION('',$,#58399);
#58281=PRODUCT_DEFINITION_FORMATION('',$,#58400);
#58282=PRODUCT_DEFINITION_FORMATION('',$,#58401);
#58283=PRODUCT_DEFINITION_FORMATION('',$,#58402);
#58284=PRODUCT_RELATED_PRODUCT_CATEGORY('PAT-046','PAT-046',(#58345));
#58285=PRODUCT_RELATED_PRODUCT_CATEGORY('Base and indicator stand',
'Base and indicator stand',(#58346));
#58286=PRODUCT_RELATED_PRODUCT_CATEGORY('Base','Base',(#58347));
#58287=PRODUCT_RELATED_PRODUCT_CATEGORY('Foot strip','Foot strip',(#58348));
#58288=PRODUCT_RELATED_PRODUCT_CATEGORY('Foot strip (1)',
'Foot strip (1)',(#58349));
#58289=PRODUCT_RELATED_PRODUCT_CATEGORY('Input bearing post',
'Input bearing post',(#58350));
#58290=PRODUCT_RELATED_PRODUCT_CATEGORY('Input outer race spacer',
'Input outer race spacer',(#58351));
#58291=PRODUCT_RELATED_PRODUCT_CATEGORY('Input bearing cap',
'Input bearing cap',(#58352));
#58292=PRODUCT_RELATED_PRODUCT_CATEGORY('Indicator stand',
'Indicator stand',(#58353));
#58293=PRODUCT_RELATED_PRODUCT_CATEGORY('Indicator arm','Indicator arm',
(#58354));
#58294=PRODUCT_RELATED_PRODUCT_CATEGORY('Indicator body envelope',
'Indicator body envelope',(#58355));
#58295=PRODUCT_RELATED_PRODUCT_CATEGORY('Indicator face',
'Indicator face',(#58356));
#58296=PRODUCT_RELATED_PRODUCT_CATEGORY('Retracted indicator probe',
'Retracted indicator probe',(#58357));
#58297=PRODUCT_RELATED_PRODUCT_CATEGORY(
'Linear Guide Rail - 15 mm, 220 mm Long',
'Linear Guide Rail - 15 mm, 220 mm Long',(#58358));
#58298=PRODUCT_RELATED_PRODUCT_CATEGORY(
'Sealed Ball Bearing - 12 x 32 x 10 mm',
'Sealed Ball Bearing - 12 x 32 x 10 mm',(#58359));
#58299=PRODUCT_RELATED_PRODUCT_CATEGORY('Inner ring','Inner ring',(#58360));
#58300=PRODUCT_RELATED_PRODUCT_CATEGORY('Outer ring','Outer ring',(#58361));
#58301=PRODUCT_RELATED_PRODUCT_CATEGORY('Balls','Balls',(#58362));
#58302=PRODUCT_RELATED_PRODUCT_CATEGORY('Cage','Cage',(#58363));
#58303=PRODUCT_RELATED_PRODUCT_CATEGORY('Seals 2RS','Seals 2RS',(#58364));
#58304=PRODUCT_RELATED_PRODUCT_CATEGORY('Cap Screw - M4x16',
'Cap Screw - M4x16',(#58365));
#58305=PRODUCT_RELATED_PRODUCT_CATEGORY('Sliding bearing carrier',
'Sliding bearing carrier',(#58366));
#58306=PRODUCT_RELATED_PRODUCT_CATEGORY('Carrier plate','Carrier plate',
(#58367));
#58307=PRODUCT_RELATED_PRODUCT_CATEGORY('Retracted rail lock pad',
'Retracted rail lock pad',(#58368));
#58308=PRODUCT_RELATED_PRODUCT_CATEGORY('Output bearing post',
'Output bearing post',(#58369));
#58309=PRODUCT_RELATED_PRODUCT_CATEGORY('Output outer race spacer',
'Output outer race spacer',(#58370));
#58310=PRODUCT_RELATED_PRODUCT_CATEGORY('Output bearing cap',
'Output bearing cap',(#58371));
#58311=PRODUCT_RELATED_PRODUCT_CATEGORY(
'Flanged Linear Guide Carriage - 15 mm',
'Flanged Linear Guide Carriage - 15 mm',(#58372));
#58312=PRODUCT_RELATED_PRODUCT_CATEGORY('Block','Block',(#58373));
#58313=PRODUCT_RELATED_PRODUCT_CATEGORY('End cap +','End cap +',(#58374));
#58314=PRODUCT_RELATED_PRODUCT_CATEGORY('End cap','End cap',(#58375));
#58315=PRODUCT_RELATED_PRODUCT_CATEGORY('Socket Set Screw - M4x6',
'Socket Set Screw - M4x6',(#58376));
#58316=PRODUCT_RELATED_PRODUCT_CATEGORY('M5x14 Cap Screw',
'M5x14 Cap Screw',(#58377));
#58317=PRODUCT_RELATED_PRODUCT_CATEGORY(
'Sealed Ball Bearing - 20 x 47 x 14 mm',
'Sealed Ball Bearing - 20 x 47 x 14 mm',(#58378));
#58318=PRODUCT_RELATED_PRODUCT_CATEGORY('Inner ring (1)',
'Inner ring (1)',(#58379));
#58319=PRODUCT_RELATED_PRODUCT_CATEGORY('Outer ring (1)',
'Outer ring (1)',(#58380));
#58320=PRODUCT_RELATED_PRODUCT_CATEGORY('Balls (1)','Balls (1)',(#58381));
#58321=PRODUCT_RELATED_PRODUCT_CATEGORY('Cage (1)','Cage (1)',(#58382));
#58322=PRODUCT_RELATED_PRODUCT_CATEGORY('Seals 2RS (1)','Seals 2RS (1)',
(#58383));
#58323=PRODUCT_RELATED_PRODUCT_CATEGORY('Input gear and arbor',
'Input gear and arbor',(#58384));
#58324=PRODUCT_RELATED_PRODUCT_CATEGORY('Input arbor','Input arbor',(#58385));
#58325=PRODUCT_RELATED_PRODUCT_CATEGORY('Input inner sleeve 10 mm',
'Input inner sleeve 10 mm',(#58386));
#58326=PRODUCT_RELATED_PRODUCT_CATEGORY('Input inner sleeve 8 mm',
'Input inner sleeve 8 mm',(#58387));
#58327=PRODUCT_RELATED_PRODUCT_CATEGORY('Input lower sleeve',
'Input lower sleeve',(#58388));
#58328=PRODUCT_RELATED_PRODUCT_CATEGORY('Input collar','Input collar',(#58389));
#58329=PRODUCT_RELATED_PRODUCT_CATEGORY('Input parallel key',
'Input parallel key',(#58390));
#58330=PRODUCT_RELATED_PRODUCT_CATEGORY('Input keeper','Input keeper',(#58391));
#58331=PRODUCT_RELATED_PRODUCT_CATEGORY(
'Spur Gear - Module 2, 20 Teeth, 12 mm Bore',
'Spur Gear - Module 2, 20 Teeth, 12 mm Bore',(#58392));
#58332=PRODUCT_RELATED_PRODUCT_CATEGORY('Output gear and arbor',
'Output gear and arbor',(#58393));
#58333=PRODUCT_RELATED_PRODUCT_CATEGORY('Output arbor','Output arbor',(#58394));
#58334=PRODUCT_RELATED_PRODUCT_CATEGORY('Output inner sleeve 6 mm',
'Output inner sleeve 6 mm',(#58395));
#58335=PRODUCT_RELATED_PRODUCT_CATEGORY('Output inner sleeve 8 mm',
'Output inner sleeve 8 mm',(#58396));
#58336=PRODUCT_RELATED_PRODUCT_CATEGORY('Output collar','Output collar',
(#58397));
#58337=PRODUCT_RELATED_PRODUCT_CATEGORY('Output parallel key',
'Output parallel key',(#58398));
#58338=PRODUCT_RELATED_PRODUCT_CATEGORY('Output keeper','Output keeper',
(#58399));
#58339=PRODUCT_RELATED_PRODUCT_CATEGORY('M4x4 collar screw',
'M4x4 collar screw',(#58400));
#58340=PRODUCT_RELATED_PRODUCT_CATEGORY(
'Spur Gear - Module 2, 40 Teeth, 20 mm Bore',
'Spur Gear - Module 2, 40 Teeth, 20 mm Bore',(#58401));
#58341=PRODUCT_RELATED_PRODUCT_CATEGORY('M4x10 Cap Screw',
'M4x10 Cap Screw',(#58402));
#58342=APPLICATION_PROTOCOL_DEFINITION('international standard',
'automotive_design',2009,#58343);
#58343=APPLICATION_CONTEXT(
'Core Data for Automotive Mechanical Design Process');
#58344=PRODUCT_CONTEXT('part definition',#58343,'mechanical');
#58345=PRODUCT('PAT-046','PAT-046',
'PAT-046',(#58344));
#58346=PRODUCT('Base and indicator stand','Base and indicator stand',
'Base and indicator stand',(#58344));
#58347=PRODUCT('Base','Base','Base',(#58344));
#58348=PRODUCT('Foot strip','Foot strip','Foot strip',(#58344));
#58349=PRODUCT('Foot strip (1)','Foot strip (1)','Foot strip (1)',(#58344));
#58350=PRODUCT('Input bearing post','Input bearing post',
'Input bearing post',(#58344));
#58351=PRODUCT('Input outer race spacer','Input outer race spacer',
'Input outer race spacer',(#58344));
#58352=PRODUCT('Input bearing cap','Input bearing cap',
'Input bearing cap',(#58344));
#58353=PRODUCT('Indicator stand','Indicator stand','Indicator stand',(#58344));
#58354=PRODUCT('Indicator arm','Indicator arm','Indicator arm',(#58344));
#58355=PRODUCT('Indicator body envelope','Indicator body envelope',
'Indicator body envelope',(#58344));
#58356=PRODUCT('Indicator face','Indicator face','Indicator face',(#58344));
#58357=PRODUCT('Retracted indicator probe','Retracted indicator probe',
'Retracted indicator probe',(#58344));
#58358=PRODUCT('Linear Guide Rail - 15 mm, 220 mm Long',
'Linear Guide Rail - 15 mm, 220 mm Long',
'Linear Guide Rail - 15 mm, 220 mm Long',(#58344));
#58359=PRODUCT('Sealed Ball Bearing - 12 x 32 x 10 mm',
'Sealed Ball Bearing - 12 x 32 x 10 mm',
'Sealed Ball Bearing - 12 x 32 x 10 mm',(#58344));
#58360=PRODUCT('Inner ring','Inner ring','Inner ring',(#58344));
#58361=PRODUCT('Outer ring','Outer ring','Outer ring',(#58344));
#58362=PRODUCT('Balls','Balls','Balls',(#58344));
#58363=PRODUCT('Cage','Cage','Cage',(#58344));
#58364=PRODUCT('Seals 2RS','Seals 2RS','Seals 2RS',(#58344));
#58365=PRODUCT('Cap Screw - M4x16','Cap Screw - M4x16',
'Cap Screw - M4x16',(#58344));
#58366=PRODUCT('Sliding bearing carrier','Sliding bearing carrier',
'Sliding bearing carrier',(#58344));
#58367=PRODUCT('Carrier plate','Carrier plate','Carrier plate',(#58344));
#58368=PRODUCT('Retracted rail lock pad','Retracted rail lock pad',
'Retracted rail lock pad',(#58344));
#58369=PRODUCT('Output bearing post','Output bearing post',
'Output bearing post',(#58344));
#58370=PRODUCT('Output outer race spacer','Output outer race spacer',
'Output outer race spacer',(#58344));
#58371=PRODUCT('Output bearing cap','Output bearing cap',
'Output bearing cap',(#58344));
#58372=PRODUCT('Flanged Linear Guide Carriage - 15 mm',
'Flanged Linear Guide Carriage - 15 mm',
'Flanged Linear Guide Carriage - 15 mm',(#58344));
#58373=PRODUCT('Block','Block','Block',(#58344));
#58374=PRODUCT('End cap +','End cap +','End cap +',(#58344));
#58375=PRODUCT('End cap','End cap','End cap',(#58344));
#58376=PRODUCT('Socket Set Screw - M4x6','Socket Set Screw - M4x6',
'Socket Set Screw - M4x6',(#58344));
#58377=PRODUCT('M5x14 Cap Screw','M5x14 Cap Screw','M5x14 Cap Screw',(#58344));
#58378=PRODUCT('Sealed Ball Bearing - 20 x 47 x 14 mm',
'Sealed Ball Bearing - 20 x 47 x 14 mm',
'Sealed Ball Bearing - 20 x 47 x 14 mm',(#58344));
#58379=PRODUCT('Inner ring (1)','Inner ring (1)','Inner ring (1)',(#58344));
#58380=PRODUCT('Outer ring (1)','Outer ring (1)','Outer ring (1)',(#58344));
#58381=PRODUCT('Balls (1)','Balls (1)','Balls (1)',(#58344));
#58382=PRODUCT('Cage (1)','Cage (1)','Cage (1)',(#58344));
#58383=PRODUCT('Seals 2RS (1)','Seals 2RS (1)','Seals 2RS (1)',(#58344));
#58384=PRODUCT('Input gear and arbor','Input gear and arbor',
'Input gear and arbor',(#58344));
#58385=PRODUCT('Input arbor','Input arbor','Input arbor',(#58344));
#58386=PRODUCT('Input inner sleeve 10 mm','Input inner sleeve 10 mm',
'Input inner sleeve 10 mm',(#58344));
#58387=PRODUCT('Input inner sleeve 8 mm','Input inner sleeve 8 mm',
'Input inner sleeve 8 mm',(#58344));
#58388=PRODUCT('Input lower sleeve','Input lower sleeve',
'Input lower sleeve',(#58344));
#58389=PRODUCT('Input collar','Input collar','Input collar',(#58344));
#58390=PRODUCT('Input parallel key','Input parallel key',
'Input parallel key',(#58344));
#58391=PRODUCT('Input keeper','Input keeper','Input keeper',(#58344));
#58392=PRODUCT('Spur Gear - Module 2, 20 Teeth, 12 mm Bore',
'Spur Gear - Module 2, 20 Teeth, 12 mm Bore',
'Spur Gear - Module 2, 20 Teeth, 12 mm Bore',(#58344));
#58393=PRODUCT('Output gear and arbor','Output gear and arbor',
'Output gear and arbor',(#58344));
#58394=PRODUCT('Output arbor','Output arbor','Output arbor',(#58344));
#58395=PRODUCT('Output inner sleeve 6 mm','Output inner sleeve 6 mm',
'Output inner sleeve 6 mm',(#58344));
#58396=PRODUCT('Output inner sleeve 8 mm','Output inner sleeve 8 mm',
'Output inner sleeve 8 mm',(#58344));
#58397=PRODUCT('Output collar','Output collar','Output collar',(#58344));
#58398=PRODUCT('Output parallel key','Output parallel key',
'Output parallel key',(#58344));
#58399=PRODUCT('Output keeper','Output keeper','Output keeper',(#58344));
#58400=PRODUCT('M4x4 collar screw','M4x4 collar screw',
'M4x4 collar screw',(#58344));
#58401=PRODUCT('Spur Gear - Module 2, 40 Teeth, 20 mm Bore',
'Spur Gear - Module 2, 40 Teeth, 20 mm Bore',
'Spur Gear - Module 2, 40 Teeth, 20 mm Bore',(#58344));
#58402=PRODUCT('M4x10 Cap Screw','M4x10 Cap Screw','M4x10 Cap Screw',(#58344));
#58403=PRESENTATION_STYLE_ASSIGNMENT((#58408));
#58404=PRESENTATION_STYLE_ASSIGNMENT((#58409));
#58405=PRESENTATION_STYLE_ASSIGNMENT((#58410));
#58406=PRESENTATION_STYLE_ASSIGNMENT((#58411));
#58407=PRESENTATION_STYLE_ASSIGNMENT((#58412));
#58408=SURFACE_STYLE_USAGE(.BOTH.,#58413);
#58409=SURFACE_STYLE_USAGE(.BOTH.,#58414);
#58410=SURFACE_STYLE_USAGE(.BOTH.,#58415);
#58411=SURFACE_STYLE_USAGE(.BOTH.,#58416);
#58412=SURFACE_STYLE_USAGE(.BOTH.,#58417);
#58413=SURFACE_SIDE_STYLE('',(#58418));
#58414=SURFACE_SIDE_STYLE('',(#58419));
#58415=SURFACE_SIDE_STYLE('',(#58420));
#58416=SURFACE_SIDE_STYLE('',(#58421));
#58417=SURFACE_SIDE_STYLE('',(#58422));
#58418=SURFACE_STYLE_FILL_AREA(#58423);
#58419=SURFACE_STYLE_FILL_AREA(#58424);
#58420=SURFACE_STYLE_FILL_AREA(#58425);
#58421=SURFACE_STYLE_FILL_AREA(#58426);
#58422=SURFACE_STYLE_FILL_AREA(#58427);
#58423=FILL_AREA_STYLE('Steel - Satin',(#58428));
#58424=FILL_AREA_STYLE('CAD Library Painted - Deep blue',(#58429));
#58425=FILL_AREA_STYLE('CAD Library Painted - Steel gray',(#58430));
#58426=FILL_AREA_STYLE('CAD Library Painted - Engineering blue',(#58431));
#58427=FILL_AREA_STYLE('CAD Library Painted - Graphite',(#58432));
#58428=FILL_AREA_STYLE_COLOUR('Steel - Satin',#58433);
#58429=FILL_AREA_STYLE_COLOUR('CAD Library Painted - Deep blue',#58434);
#58430=FILL_AREA_STYLE_COLOUR('CAD Library Painted - Steel gray',#58435);
#58431=FILL_AREA_STYLE_COLOUR('CAD Library Painted - Engineering blue',
#58436);
#58432=FILL_AREA_STYLE_COLOUR('CAD Library Painted - Graphite',#58437);
#58433=COLOUR_RGB('Steel - Satin',0.627450980392157,0.627450980392157,0.627450980392157);
#58434=COLOUR_RGB('CAD Library Painted - Deep blue',0.0784313725490196,
0.203921568627451,0.349019607843137);
#58435=COLOUR_RGB('CAD Library Painted - Steel gray',0.592156862745098,
0.631372549019608,0.67843137254902);
#58436=COLOUR_RGB('CAD Library Painted - Engineering blue',0.12156862745098,
0.356862745098039,0.6);
#58437=COLOUR_RGB('CAD Library Painted - Graphite',0.168627450980392,0.192156862745098,
0.231372549019608);
#58438=COLOUR_RGB('Dark Blue',0.08,0.2,0.34);
#58439=FILL_AREA_STYLE_COLOUR('',#58438);
#58440=FILL_AREA_STYLE('',(#58439));
#58441=SURFACE_STYLE_FILL_AREA(#58440);
#58442=SURFACE_SIDE_STYLE('',(#58441));
#58443=SURFACE_STYLE_USAGE(.BOTH.,#58442);
#58444=PRESENTATION_STYLE_ASSIGNMENT((#58443));
#58445=COLOUR_RGB('Light Blue',0.38,0.62,0.78);
#58446=FILL_AREA_STYLE_COLOUR('',#58445);
#58447=FILL_AREA_STYLE('',(#58446));
#58448=SURFACE_STYLE_FILL_AREA(#58447);
#58449=SURFACE_SIDE_STYLE('',(#58448));
#58450=SURFACE_STYLE_USAGE(.BOTH.,#58449);
#58451=PRESENTATION_STYLE_ASSIGNMENT((#58450));
#58452=COLOUR_RGB('Sky Blue',0.24,0.69,0.87);
#58453=FILL_AREA_STYLE_COLOUR('',#58452);
#58454=FILL_AREA_STYLE('',(#58453));
#58455=SURFACE_STYLE_FILL_AREA(#58454);
#58456=SURFACE_SIDE_STYLE('',(#58455));
#58457=SURFACE_STYLE_USAGE(.BOTH.,#58456);
#58458=PRESENTATION_STYLE_ASSIGNMENT((#58457));
#58459=COLOUR_RGB('Grey',0.48,0.52,0.57);
#58460=FILL_AREA_STYLE_COLOUR('',#58459);
#58461=FILL_AREA_STYLE('',(#58460));
#58462=SURFACE_STYLE_FILL_AREA(#58461);
#58463=SURFACE_SIDE_STYLE('',(#58462));
#58464=SURFACE_STYLE_USAGE(.BOTH.,#58463);
#58465=PRESENTATION_STYLE_ASSIGNMENT((#58464));
#58466=COLOUR_RGB('Black',0.12,0.14,0.17);
#58467=FILL_AREA_STYLE_COLOUR('',#58466);
#58468=FILL_AREA_STYLE('',(#58467));
#58469=SURFACE_STYLE_FILL_AREA(#58468);
#58470=SURFACE_SIDE_STYLE('',(#58469));
#58471=SURFACE_STYLE_USAGE(.BOTH.,#58470);
#58472=PRESENTATION_STYLE_ASSIGNMENT((#58471));
#58473=COLOUR_RGB('Off White',0.89,0.88,0.83);
#58474=FILL_AREA_STYLE_COLOUR('',#58473);
#58475=FILL_AREA_STYLE('',(#58474));
#58476=SURFACE_STYLE_FILL_AREA(#58475);
#58477=SURFACE_SIDE_STYLE('',(#58476));
#58478=SURFACE_STYLE_USAGE(.BOTH.,#58477);
#58479=PRESENTATION_STYLE_ASSIGNMENT((#58478));
ENDSEC;
END-ISO-10303-21;
